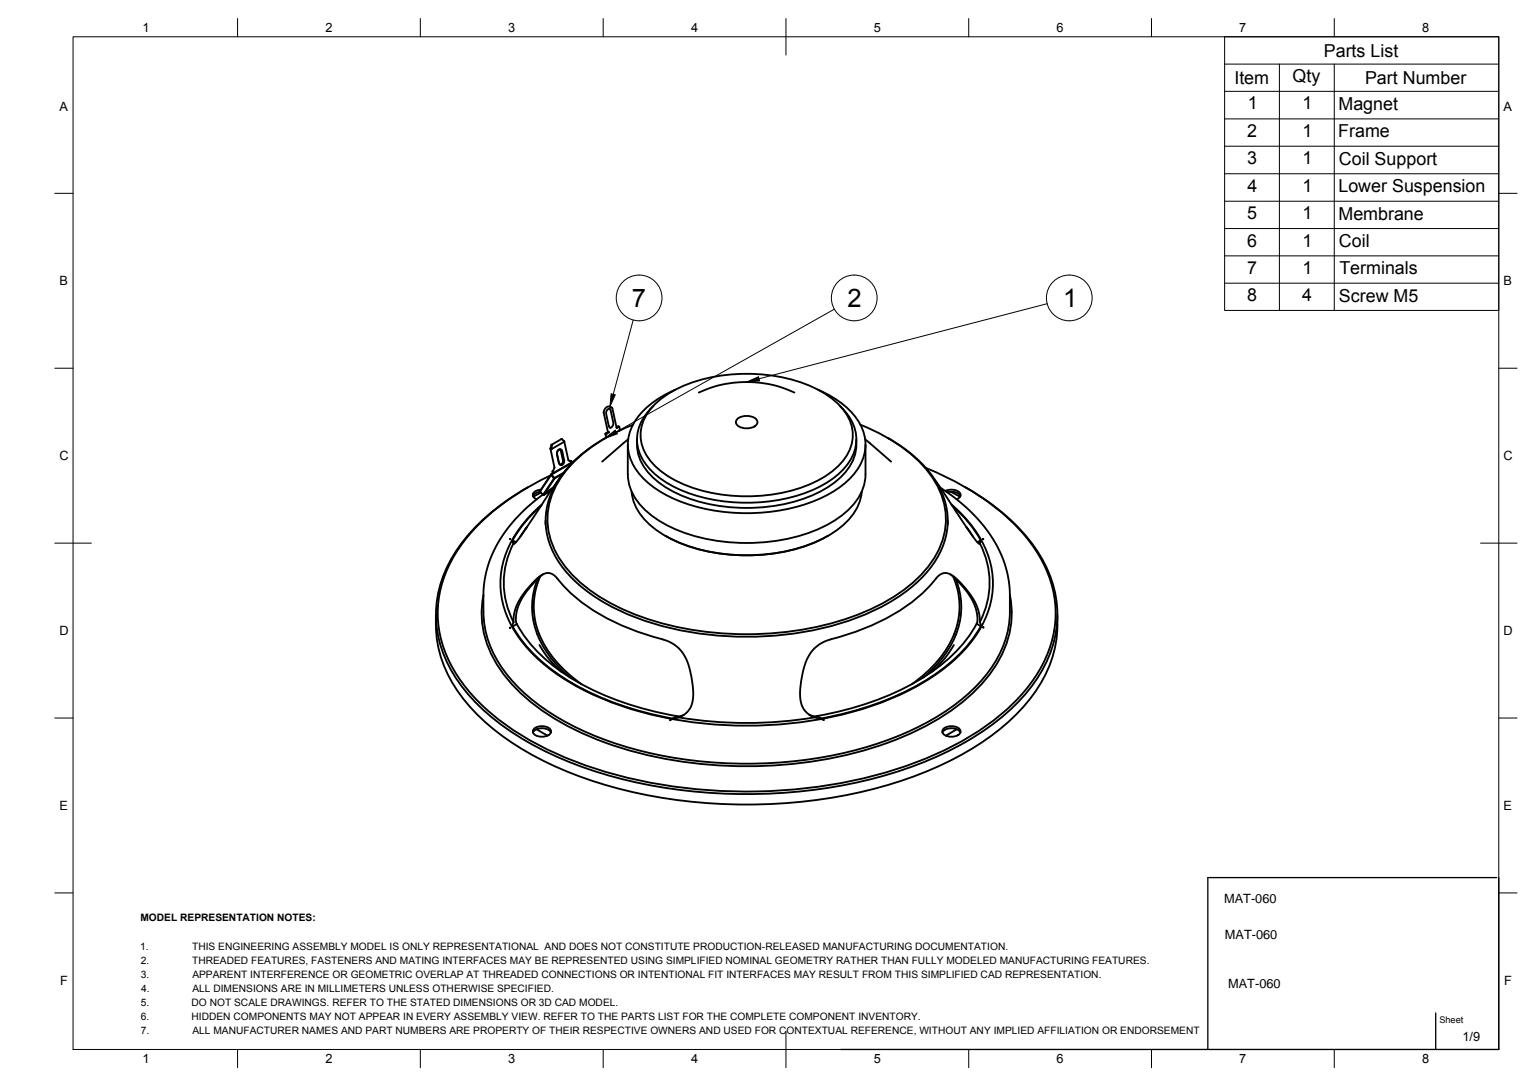
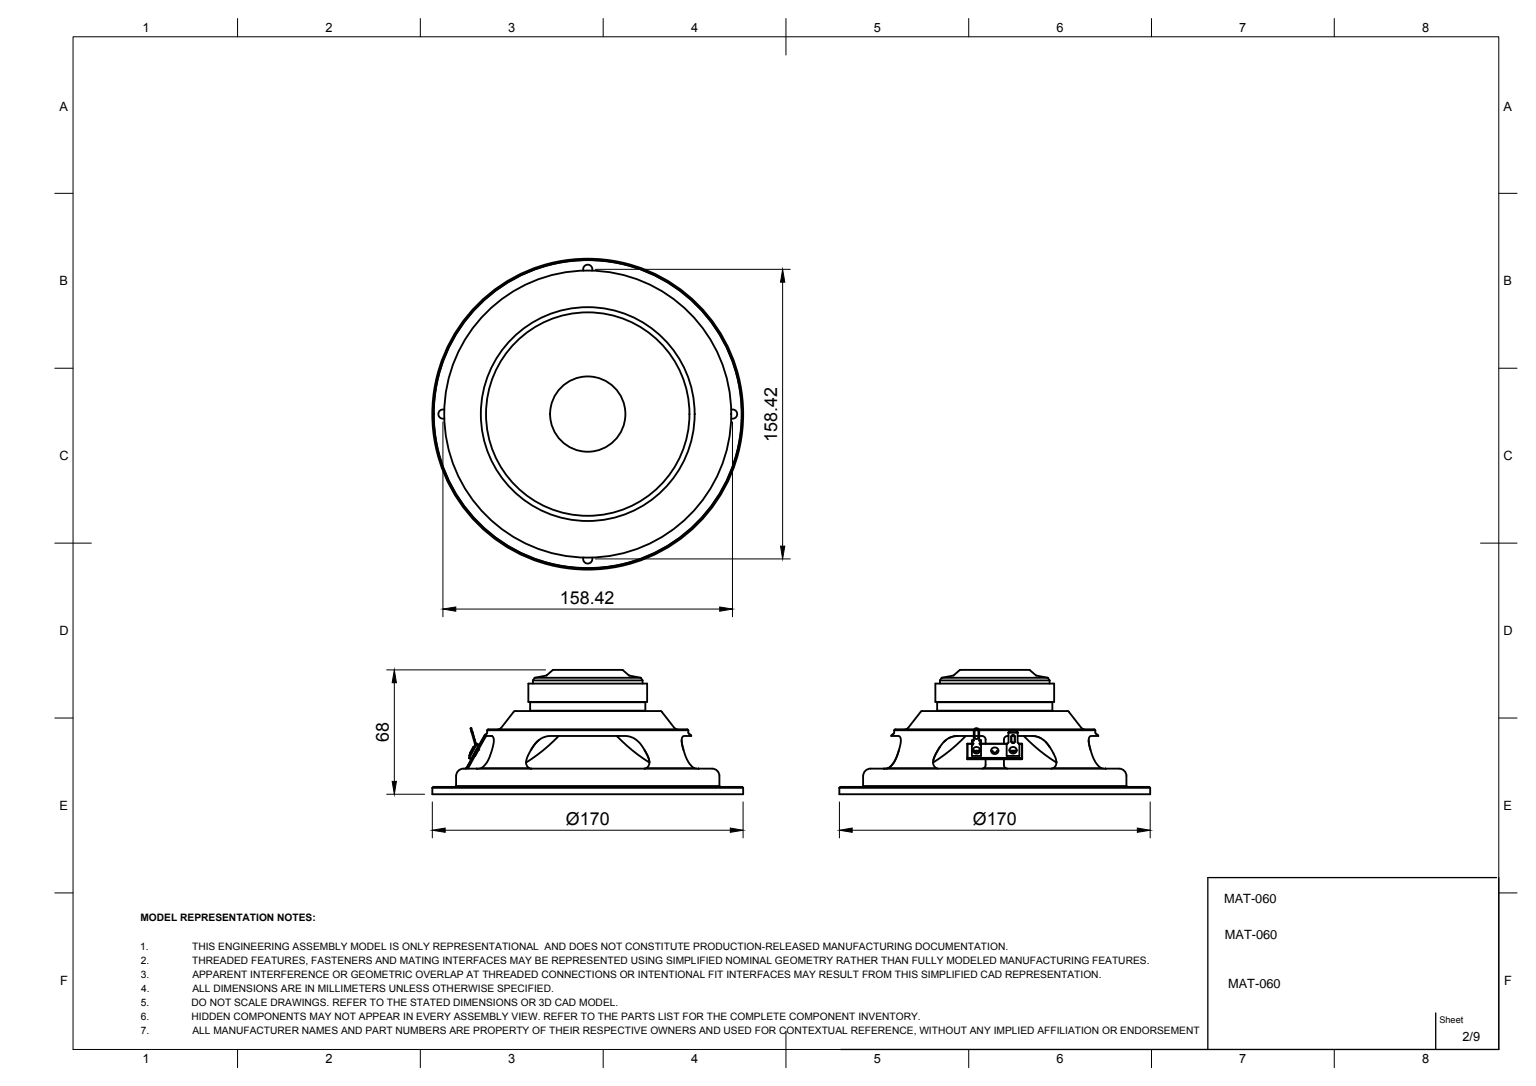
ISO-10303-21;
HEADER;
FILE_DESCRIPTION (('STEP AP214'),
    '1' );
FILE_NAME ('MAT-060',
    '2026-10-29T23:46:56',
    ( '' ),
    ( '' ),
    'SwSTEP 2.0',
    'SolidWorks 2020',
    '' );
FILE_SCHEMA (( 'AUTOMOTIVE_DESIGN' ));
ENDSEC;

DATA;
#1 = ADVANCED_FACE ( 'NONE', ( #23407 ), #603, .F. ) ;
#2 = VECTOR ( 'NONE', #10897, 1000.000000000000000 ) ;
#3 = CARTESIAN_POINT ( 'NONE',  ( -8.402144023942796025, 14.86454579224779948, 47.04930799450052348 ) ) ;
#4 = CIRCLE ( 'NONE', #18333, 0.1250000000000001110 ) ;
#5 = EDGE_CURVE ( 'NONE', #10473, #12904, #9508, .T. ) ;
#6 = ADVANCED_FACE ( 'NONE', ( #18472 ), #27339, .T. ) ;
#7 = DIRECTION ( 'NONE',  ( -0.000000000000000000, -1.000000000000000000, 0.000000000000000000 ) ) ;
#8 = ORIENTED_EDGE ( 'NONE', *, *, #21426, .T. ) ;
#9 = CARTESIAN_POINT ( 'NONE',  ( 52.18344119656808289, -5.936379232154279428, 107.4303245894588628 ) ) ;
#10 = ORIENTED_EDGE ( 'NONE', *, *, #17862, .T. ) ;
#11 = DIRECTION ( 'NONE',  ( 0.000000000000000000, 0.000000000000000000, -1.000000000000000000 ) ) ;
#12 = DIRECTION ( 'NONE',  ( -1.000000000000000000, 0.000000000000000000, 0.000000000000000000 ) ) ;
#13 = VECTOR ( 'NONE', #9862, 1000.000000000000000 ) ;
#14 = CONICAL_SURFACE ( 'NONE', #3681, 2.923537884824412014, 0.6981317007977324574 ) ;
#15 = CARTESIAN_POINT ( 'NONE',  ( 49.15300726216835159, 22.74928388133296764, 45.65942558980532340 ) ) ;
#16 = CIRCLE ( 'NONE', #21997, 37.50000000000000711 ) ;
#17 = AXIS2_PLACEMENT_3D ( 'NONE', #6109, #14151, #26614 ) ;
#18 = EDGE_CURVE ( 'NONE', #23289, #31921, #28501, .T. ) ;
#19 = AXIS2_PLACEMENT_3D ( 'NONE', #29892, #26933, #14470 ) ;
#20 = EDGE_LOOP ( 'NONE', ( #20639, #20304, #9074, #30153 ) ) ;
#21 = ORIENTED_EDGE ( 'NONE', *, *, #19854, .F. ) ;
#22 = DIRECTION ( 'NONE',  ( 7.588956326749211550E-18, -4.206627182996911684E-18, 1.000000000000000000 ) ) ;
#23 = DIRECTION ( 'NONE',  ( 0.000000000000000000, 0.000000000000000000, 1.000000000000000000 ) ) ;
#24 = CARTESIAN_POINT ( 'NONE',  ( 46.00908685603034343, 26.23284706826093071, 44.91496614357595263 ) ) ;
#25 = CONICAL_SURFACE ( 'NONE', #4214, 67.38776620500242132, 0.5061454830783623793 ) ;
#26 = VERTEX_POINT ( 'NONE', #18783 ) ;
#27 = DIRECTION ( 'NONE',  ( 0.9612616959383206705, 0.2756373558169926130, 8.795445018804289444E-19 ) ) ;
#28 = FACE_OUTER_BOUND ( 'NONE', #27332, .T. ) ;
#29 = CARTESIAN_POINT ( 'NONE',  ( -42.41019933908752648, 14.71530103803245915, 55.14139656020049785 ) ) ;
#30 = EDGE_CURVE ( 'NONE', #9758, #27591, #28910, .T. ) ;
#31 = DIRECTION ( 'NONE',  ( -1.101824276508909887E-16, 1.000000000000000000, -0.000000000000000000 ) ) ;
#32 = AXIS2_PLACEMENT_3D ( 'NONE', #27691, #3055, #609 ) ;
#33 = EDGE_CURVE ( 'NONE', #28622, #18652, #13708, .T. ) ;
#34 = CARTESIAN_POINT ( 'NONE',  ( 46.96819297411687444, 27.59253733014356058, 49.54594323136014822 ) ) ;
#35 = CARTESIAN_POINT ( 'NONE',  ( 49.62252444096254322, 24.84787913140503690, 48.68715535708000175 ) ) ;
#36 = DIRECTION ( 'NONE',  ( 0.9612616959383191162, 0.2756373558169986082, 8.795445018805098335E-19 ) ) ;
#37 = CARTESIAN_POINT ( 'NONE',  ( 44.79156314060809763, 22.80400562401889530, 46.92953032342012420 ) ) ;
#38 = FACE_OUTER_BOUND ( 'NONE', #16032, .T. ) ;
#39 = VECTOR ( 'NONE', #4275, 1000.000000000000000 ) ;
#40 = CARTESIAN_POINT ( 'NONE',  ( 21.09785597605719332, 12.26495659406217342, 47.04930799450051637 ) ) ;
#41 = AXIS2_PLACEMENT_3D ( 'NONE', #1077, #13253, #30795 ) ;
#42 = FILL_AREA_STYLE ('',( #30241 ) ) ;
#43 = ORIENTED_EDGE ( 'NONE', *, *, #17117, .T. ) ;
#44 = ORIENTED_EDGE ( 'NONE', *, *, #10247, .F. ) ;
#45 = AXIS2_PLACEMENT_3D ( 'NONE', #7239, #26769, #16743 ) ;
#46 = DIRECTION ( 'NONE',  ( -1.000000000000000000, 0.000000000000000000, 0.000000000000000000 ) ) ;
#47 = VECTOR ( 'NONE', #22684, 1000.000000000000114 ) ;
#48 = DIRECTION ( 'NONE',  ( 1.000000000000000000, -3.756723415560144304E-15, 0.000000000000000000 ) ) ;
#49 = EDGE_CURVE ( 'NONE', #29330, #16793, #26511, .T. ) ;
#50 = DIRECTION ( 'NONE',  ( -1.000000000000000000, 0.000000000000000000, 0.000000000000000000 ) ) ;
#51 = ADVANCED_FACE ( 'NONE', ( #19270 ), #7428, .T. ) ;
#52 = EDGE_LOOP ( 'NONE', ( #4319, #21732, #2975, #7082 ) ) ;
#53 = DIRECTION ( 'NONE',  ( -1.000000000000000000, 0.000000000000000000, 0.000000000000000000 ) ) ;
#54 = CARTESIAN_POINT ( 'NONE',  ( -41.75126335834794133, 15.45321085637654690, 35.55750462089839203 ) ) ;
#55 = ORIENTED_EDGE ( 'NONE', *, *, #8639, .T. ) ;
#56 = ORIENTED_EDGE ( 'NONE', *, *, #16072, .T. ) ;
#57 = CARTESIAN_POINT ( 'NONE',  ( -40.99628586177130529, 8.927770518203464789, 58.05249952744806308 ) ) ;
#58 = CARTESIAN_POINT ( 'NONE',  ( 44.70507715278255745, 27.74951373492759643, 46.92503878583764987 ) ) ;
#59 = AXIS2_PLACEMENT_3D ( 'NONE', #2818, #5773, #10865 ) ;
#60 = LINE ( 'NONE', #27627, #25175 ) ;
#61 = DIRECTION ( 'NONE',  ( -0.000000000000000000, -1.000000000000000000, 0.000000000000000000 ) ) ;
#62 = PLANE ( 'NONE',  #14629 ) ;
#63 = VERTEX_POINT ( 'NONE', #26669 ) ;
#64 = DIRECTION ( 'NONE',  ( -1.101824276508909887E-16, 1.000000000000000000, -0.000000000000000000 ) ) ;
#65 = AXIS2_PLACEMENT_3D ( 'NONE', #14177, #6132, #1197 ) ;
#66 = ORIENTED_EDGE ( 'NONE', *, *, #7414, .F. ) ;
#67 =( BOUNDED_CURVE ( )  B_SPLINE_CURVE ( 3, ( #13523, #18741, #20741, #23527 ),
 .UNSPECIFIED., .F., .F. ) 
 B_SPLINE_CURVE_WITH_KNOTS ( ( 4, 4 ),
 ( 1.099063246724957033, 1.220321128156881318 ),
 .UNSPECIFIED. ) 
 CURVE ( )  GEOMETRIC_REPRESENTATION_ITEM ( )  RATIONAL_B_SPLINE_CURVE ( ( 1.000000000000000000, 0.9987750858034805113, 0.9987750858034805113, 1.000000000000000000 ) ) 
 REPRESENTATION_ITEM ( '' )  );
#68 = FACE_OUTER_BOUND ( 'NONE', #23592, .T. ) ;
#69 = CARTESIAN_POINT ( 'NONE',  ( -40.69193635511749108, 9.347952559758585522, 39.44930799450052206 ) ) ;
#70 = CIRCLE ( 'NONE', #12126, 59.80962967564905597 ) ;
#71 = ORIENTED_EDGE ( 'NONE', *, *, #26696, .T. ) ;
#72 = CARTESIAN_POINT ( 'NONE',  ( -40.77849034781615956, 8.435947495041027366, 34.55508635502627612 ) ) ;
#73 = EDGE_LOOP ( 'NONE', ( #31161, #6796, #19023, #7064 ) ) ;
#74 = CARTESIAN_POINT ( 'NONE',  ( 21.09992658989238734, 38.56284415653841791, 47.04930799450051637 ) ) ;
#75 = CARTESIAN_POINT ( 'NONE',  ( -40.75848109938849717, 9.580021662090986823, 38.54930799450052348 ) ) ;
#76 = DIRECTION ( 'NONE',  ( 0.4848096202463429982, 0.8746197071393925215, 9.920727850371698576E-18 ) ) ;
#77 = ORIENTED_EDGE ( 'NONE', *, *, #10123, .F. ) ;
#78 = CARTESIAN_POINT ( 'NONE',  ( 21.09785597605719332, 15.24673779880127356, 47.04930799450051637 ) ) ;
#79 = DIRECTION ( 'NONE',  ( -1.000000000000000000, 0.000000000000000000, 0.000000000000000000 ) ) ;
#80 = DIRECTION ( 'NONE',  ( -1.000000000000000000, -1.101824276508909887E-16, 0.000000000000000000 ) ) ;
#81 = EDGE_CURVE ( 'NONE', #21567, #17692, #8244, .T. ) ;
#82 = CARTESIAN_POINT ( 'NONE',  ( -39.58809650894544774, 2.596771453999702661, 45.04930799450051637 ) ) ;
#83 = CONICAL_SURFACE ( 'NONE', #4821, 67.99999999999998579, 0.5061454830783623793 ) ;
#84 = ADVANCED_FACE ( 'NONE', ( #31282 ), #25012, .T. ) ;
#85 = DIRECTION ( 'NONE',  ( 0.000000000000000000, 1.000000000000000000, -0.000000000000000000 ) ) ;
#86 = ORIENTED_EDGE ( 'NONE', *, *, #14796, .T. ) ;
#87 = AXIS2_PLACEMENT_3D ( 'NONE', #1243, #25723, #26032 ) ;
#88 = DIRECTION ( 'NONE',  ( 0.000000000000000000, 1.000000000000000000, -0.000000000000000000 ) ) ;
#89 = DIRECTION ( 'NONE',  ( -1.000000000000000000, 0.000000000000000000, 0.000000000000000000 ) ) ;
#90 = VERTEX_POINT ( 'NONE', #16171 ) ;
#91 = AXIS2_PLACEMENT_3D ( 'NONE', #3983, #26796, #16125 ) ;
#92 = CARTESIAN_POINT ( 'NONE',  ( 21.09992658989239089, 30.34164230456639544, 47.04930799450051637 ) ) ;
#93 = APPLICATION_CONTEXT ( 'automotive_design' ) ;
#94 = DIRECTION ( 'NONE',  ( 0.000000000000000000, 0.000000000000000000, 1.000000000000000000 ) ) ;
#95 = ORIENTED_EDGE ( 'NONE', *, *, #26981, .T. ) ;
#96 = CARTESIAN_POINT ( 'NONE',  ( -35.64882101543633297, 9.925589859889722533, 42.04930799450051637 ) ) ;
#97 = ORIENTED_EDGE ( 'NONE', *, *, #2403, .T. ) ;
#98 = CONICAL_SURFACE ( 'NONE', #18421, 11.79999999999997762, 0.7853981633974786991 ) ;
#99 = EDGE_LOOP ( 'NONE', ( #29307, #17559, #4595, #27909 ) ) ;
#100 = VECTOR ( 'NONE', #2675, 1000.000000000000114 ) ;
#101 = LINE ( 'NONE', #30305, #23466 ) ;
#102 = DIRECTION ( 'NONE',  ( 1.000000000000000000, 0.000000000000000000, 0.000000000000000000 ) ) ;
#103 = ORIENTED_EDGE ( 'NONE', *, *, #27267, .F. ) ;
#104 = VERTEX_POINT ( 'NONE', #1886 ) ;
#105 = CYLINDRICAL_SURFACE ( 'NONE', #15721, 33.50000000000000000 ) ;
#106 = DIRECTION ( 'NONE',  ( 0.000000000000000000, 0.000000000000000000, 1.000000000000000000 ) ) ;
#107 = DIRECTION ( 'NONE',  ( 1.000000000000000000, 0.000000000000000000, 0.000000000000000000 ) ) ;
#108 = DIRECTION ( 'NONE',  ( 0.9612616959383206705, 0.2756373558169926130, 8.795445018804289444E-19 ) ) ;
#109 = FACE_OUTER_BOUND ( 'NONE', #5838, .T. ) ;
#110 = VERTEX_POINT ( 'NONE', #16495 ) ;
#111 = DIRECTION ( 'NONE',  ( -0.000000000000000000, 1.000000000000000000, -0.000000000000000000 ) ) ;
#112 = VERTEX_POINT ( 'NONE', #21899 ) ;
#113 = CARTESIAN_POINT ( 'NONE',  ( 8.732853799281732776, 24.72145308207319303, 47.04930799450051637 ) ) ;
#114 = CARTESIAN_POINT ( 'NONE',  ( 80.65492537559437380, -5.936611295272316902, 15.94352045161622655 ) ) ;
#115 = VECTOR ( 'NONE', #2052, 999.9999999999998863 ) ;
#116 = VERTEX_POINT ( 'NONE', #3866 ) ;
#117 = CARTESIAN_POINT ( 'NONE',  ( 8.732853799281729223, 24.47145308207319303, 47.04930799450051637 ) ) ;
#118 = SPHERICAL_SURFACE ( 'NONE', #22577, 0.1000000000000000056 ) ;
#119 = DIRECTION ( 'NONE',  ( -1.101824276508909887E-16, 1.000000000000000000, -0.000000000000000000 ) ) ;
#120 = CYLINDRICAL_SURFACE ( 'NONE', #5324, 12.36707279061065101 ) ;
#121 = FACE_OUTER_BOUND ( 'NONE', #7290, .T. ) ;
#122 = EDGE_CURVE ( 'NONE', #19617, #28878, #29198, .T. ) ;
#123 = EDGE_CURVE ( 'NONE', #13895, #2732, #897, .T. ) ;
#124 = TOROIDAL_SURFACE ( 'NONE', #25795, 12.40141737965280555, 0.1250000000000006939 ) ;
#125 = CARTESIAN_POINT ( 'NONE',  ( 44.70507715278255745, 28.36291119454914877, 46.92503878583765697 ) ) ;
#126 = EDGE_CURVE ( 'NONE', #12313, #19851, #23434, .T. ) ;
#127 = FACE_OUTER_BOUND ( 'NONE', #2532, .T. ) ;
#128 = DIRECTION ( 'NONE',  ( 0.000000000000000000, 0.000000000000000000, -1.000000000000000000 ) ) ;
#129 = ADVANCED_FACE ( 'NONE', ( #26182 ), #24211, .T. ) ;
#130 = ADVANCED_FACE ( 'NONE', ( #9112 ), #21404, .F. ) ;
#131 = EDGE_LOOP ( 'NONE', ( #2067, #16349, #32197, #29803 ) ) ;
#132 = DIRECTION ( 'NONE',  ( 0.000000000000000000, 0.000000000000000000, -1.000000000000000000 ) ) ;
#133 = CARTESIAN_POINT ( 'NONE',  ( 33.72499318558949710, 28.84143805560861296, 47.04930799450051637 ) ) ;
#134 = ORIENTED_EDGE ( 'NONE', *, *, #4627, .F. ) ;
#135 = AXIS2_PLACEMENT_3D ( 'NONE', #30752, #22633, #17877 ) ;
#136 = FACE_OUTER_BOUND ( 'NONE', #14776, .T. ) ;
#137 = ORIENTED_EDGE ( 'NONE', *, *, #30547, .F. ) ;
#138 = CIRCLE ( 'NONE', #18459, 2.500000000000003553 ) ;
#139 = EDGE_LOOP ( 'NONE', ( #10436, #9194, #21125, #26055 ) ) ;
#140 = CARTESIAN_POINT ( 'NONE',  ( 21.09992658989239089, 27.84164230456639544, 47.04930799450051637 ) ) ;
#141 = ORIENTED_EDGE ( 'NONE', *, *, #21145, .F. ) ;
#142 = CIRCLE ( 'NONE', #13264, 12.36707279061065101 ) ;
#143 = ORIENTED_EDGE ( 'NONE', *, *, #20256, .T. ) ;
#144 = AXIS2_PLACEMENT_3D ( 'NONE', #10705, #31040, #25937 ) ;
#145 = CARTESIAN_POINT ( 'NONE',  ( 46.44275705260056242, 23.09557481883486219, 47.38348660136355051 ) ) ;
#146 = EDGE_CURVE ( 'NONE', #7136, #25895, #22084, .T. ) ;
#147 = ORIENTED_EDGE ( 'NONE', *, *, #1574, .F. ) ;
#148 = DIRECTION ( 'NONE',  ( -1.000000000000000000, 0.000000000000000000, 0.000000000000000000 ) ) ;
#149 = AXIS2_PLACEMENT_3D ( 'NONE', #13743, #23739, #24058 ) ;
#150 = FACE_OUTER_BOUND ( 'NONE', #25843, .T. ) ;
#151 = CARTESIAN_POINT ( 'NONE',  ( -9.910881874767294875, -5.936607700120025477, -13.36061728824001804 ) ) ;
#152 = CARTESIAN_POINT ( 'NONE',  ( 45.79384627280941089, 24.97957786121582302, 49.05938063676249072 ) ) ;
#153 = ORIENTED_EDGE ( 'NONE', *, *, #20856, .F. ) ;
#154 = VERTEX_POINT ( 'NONE', #31766 ) ;
#155 = VERTEX_POINT ( 'NONE', #13728 ) ;
#156 = CARTESIAN_POINT ( 'NONE',  ( -40.54018958231235814, 7.005332542891154368, 35.02307665165292150 ) ) ;
#157 = DIRECTION ( 'NONE',  ( -1.000000000000000000, 0.000000000000000000, 0.000000000000000000 ) ) ;
#158 = CARTESIAN_POINT ( 'NONE',  ( -40.76199410932685652, 8.110698076655893374, 59.50788663826320146 ) ) ;
#159 = CARTESIAN_POINT ( 'NONE',  ( 21.09785597605720753, 14.86454579224779948, 47.04930799450052348 ) ) ;
#160 = CARTESIAN_POINT ( 'NONE',  ( 75.19785597605721250, 14.66454579224780019, 47.04930799450051637 ) ) ;
#161 = EDGE_CURVE ( 'NONE', #17230, #26186, #19107, .T. ) ;
#162 = PRODUCT_CONTEXT ( 'NONE', #1750, 'mechanical' ) ;
#163 = VERTEX_POINT ( 'NONE', #26839 ) ;
#164 = ORIENTED_EDGE ( 'NONE', *, *, #2840, .T. ) ;
#165 = DIRECTION ( 'NONE',  ( 0.8907924397839086517, 1.100109291107994064E-16, -0.4544104193609905251 ) ) ;
#166 = FACE_OUTER_BOUND ( 'NONE', #10063, .T. ) ;
#167 = DIRECTION ( 'NONE',  ( -0.000000000000000000, -1.000000000000000000, -0.000000000000000000 ) ) ;
#168 = VECTOR ( 'NONE', #18188, 1000.000000000000114 ) ;
#169 = ORIENTED_EDGE ( 'NONE', *, *, #20266, .F. ) ;
#170 = DIRECTION ( 'NONE',  ( -1.096245967261381435E-16, 0.000000000000000000, 1.000000000000000000 ) ) ;
#171 = AXIS2_PLACEMENT_3D ( 'NONE', #9638, #108, #19631 ) ;
#172 = EDGE_LOOP ( 'NONE', ( #1126, #13141, #16684, #10184 ) ) ;
#173 = CARTESIAN_POINT ( 'NONE',  ( 21.09992658989239089, 24.71664230456639899, 47.04930799450051637 ) ) ;
#174 = DIRECTION ( 'NONE',  ( -1.101824276508909887E-16, 1.000000000000000000, -0.000000000000000000 ) ) ;
#175 = DIRECTION ( 'NONE',  ( 0.3958453973320085195, 0.7141240004913234074, 0.5773502691896251759 ) ) ;
#176 = VECTOR ( 'NONE', #32272, 1000.000000000000114 ) ;
#177 = VECTOR ( 'NONE', #9320, 1000.000000000000114 ) ;
#178 = EDGE_CURVE ( 'NONE', #17205, #26283, #21557, .T. ) ;
#179 = EDGE_CURVE ( 'NONE', #22338, #15550, #10168, .T. ) ;
#180 = VERTEX_POINT ( 'NONE', #22065 ) ;
#181 = ORIENTED_EDGE ( 'NONE', *, *, #20445, .T. ) ;
#182 = DIRECTION ( 'NONE',  ( -1.000000000000000000, 0.000000000000000000, 0.000000000000000000 ) ) ;
#183 = ADVANCED_FACE ( 'NONE', ( #22228 ), #31147, .T. ) ;
#184 = DIRECTION ( 'NONE',  ( 0.8746197071393858602, -0.4848096202463547666, 0.000000000000000000 ) ) ;
#185 = CARTESIAN_POINT ( 'NONE',  ( 49.49063479933183629, 26.69951373492759927, 47.17357720316391578 ) ) ;
#186 = EDGE_CURVE ( 'NONE', #20059, #17152, #210, .T. ) ;
#187 = ORIENTED_EDGE ( 'NONE', *, *, #28945, .F. ) ;
#188 = AXIS2_PLACEMENT_3D ( 'NONE', #771, #25875, #3057 ) ;
#189 = CARTESIAN_POINT ( 'NONE',  ( -29.27613032885505007, 5.786704587343633577, 77.24891569812123748 ) ) ;
#190 = CARTESIAN_POINT ( 'NONE',  ( 21.09992658989238734, 38.56284415653841791, 47.04930799450051637 ) ) ;
#191 = CARTESIAN_POINT ( 'NONE',  ( 8.698509210239514289, 24.84164230456639544, 47.04930799450051637 ) ) ;
#192 = DIRECTION ( 'NONE',  ( -0.9612616959383207815, -0.2756373558169926685, -8.795445018804289444E-19 ) ) ;
#193 = DIRECTION ( 'NONE',  ( -1.000000000000000000, 0.000000000000000000, 0.000000000000000000 ) ) ;
#194 = CARTESIAN_POINT ( 'NONE',  ( 48.28214861297873028, 24.78954579807170333, 49.37090702980594870 ) ) ;
#196 = CIRCLE ( 'NONE', #709, 0.8928932188134561798 ) ;
#195 = CARTESIAN_POINT ( 'NONE',  ( -42.67844523361456766, 15.18734573188464765, 35.55750462089839203 ) ) ;
#197 = DIRECTION ( 'NONE',  ( -0.9612616959383183390, -0.2756373558170014948, -8.795445018805493151E-19 ) ) ;
#198 = CIRCLE ( 'NONE', #29008, 34.00000000000000000 ) ;
#199 = CARTESIAN_POINT ( 'NONE',  ( 42.60793425459065986, 11.86918370369814113, 98.63420711611333047 ) ) ;
#200 = DIRECTION ( 'NONE',  ( -1.000000000000000000, 0.000000000000000000, 0.000000000000000000 ) ) ;
#201 = EDGE_CURVE ( 'NONE', #31745, #29739, #32095, .T. ) ;
#202 = ORIENTED_EDGE ( 'NONE', *, *, #17749, .F. ) ;
#203 = ORIENTED_EDGE ( 'NONE', *, *, #32319, .T. ) ;
#204 = CARTESIAN_POINT ( 'NONE',  ( 33.46699938050303302, 38.56284415653841791, 47.04930799450051637 ) ) ;
#205 = CARTESIAN_POINT ( 'NONE',  ( 49.62266228875127183, 24.94631262459061105, 46.45121837018842825 ) ) ;
#206 = LINE ( 'NONE', #27459, #13028 ) ;
#207 = CARTESIAN_POINT ( 'NONE',  ( 48.66895200406656130, 27.18420399681022914, 44.62753372671561181 ) ) ;
#208 = ORIENTED_EDGE ( 'NONE', *, *, #19172, .F. ) ;
#209 = DIRECTION ( 'NONE',  ( 0.2756373558169961657, -0.9612616959383196713, -2.918609477355923238E-15 ) ) ;
#210 = CIRCLE ( 'NONE', #18531, 55.85791022362053582 ) ;
#211 = CARTESIAN_POINT ( 'NONE',  ( -43.29088418437023478, 1.073429008971243270, 39.44930799450052916 ) ) ;
#212 = CARTESIAN_POINT ( 'NONE',  ( 21.09785597605720753, 15.23835801850285776, 47.04930799450052348 ) ) ;
#213 = ORIENTED_EDGE ( 'NONE', *, *, #21228, .T. ) ;
#214 = ORIENTED_EDGE ( 'NONE', *, *, #14166, .F. ) ;
#215 = CARTESIAN_POINT ( 'NONE',  ( 8.732853799281732776, 31.97145308207317171, 47.04930799450051637 ) ) ;
#216 = CARTESIAN_POINT ( 'NONE',  ( 46.00908685603034343, 25.53284706826093498, 44.91496614357595263 ) ) ;
#217 = DIRECTION ( 'NONE',  ( -1.000000000000000000, 0.000000000000000000, 0.000000000000000000 ) ) ;
#218 = LINE ( 'NONE', #12381, #10663 ) ;
#219 = CARTESIAN_POINT ( 'NONE',  ( 8.823509210239564027, 29.84164230456639899, 47.04930799450051637 ) ) ;
#220 = ADVANCED_FACE ( 'NONE', ( #24531 ), #2050, .F. ) ;
#221 = EDGE_CURVE ( 'NONE', #14341, #26283, #20036, .T. ) ;
#222 = EDGE_LOOP ( 'NONE', ( #26928, #11446, #19601, #18830 ) ) ;
#223 = DIRECTION ( 'NONE',  ( -1.000000000000000000, 0.000000000000000000, 0.000000000000000000 ) ) ;
#224 = EDGE_CURVE ( 'NONE', #23081, #15904, #26859, .T. ) ;
#225 = ORIENTED_EDGE ( 'NONE', *, *, #23042, .T. ) ;
#226 = EDGE_CURVE ( 'NONE', #1958, #14944, #28442, .T. ) ;
#227 = FACE_OUTER_BOUND ( 'NONE', #31629, .T. ) ;
#228 = DIRECTION ( 'NONE',  ( -1.101824276508909887E-16, 1.000000000000000000, -0.000000000000000000 ) ) ;
#229 = VERTEX_POINT ( 'NONE', #19763 ) ;
#230 = CARTESIAN_POINT ( 'NONE',  ( 21.09992658989238734, 31.96183152705962272, 47.04930799450051637 ) ) ;
#231 = VERTEX_POINT ( 'NONE', #9774 ) ;
#232 = CARTESIAN_POINT ( 'NONE',  ( -40.60333149162104860, 7.557375771971046596, 56.04611646155296256 ) ) ;
#233 = DIRECTION ( 'NONE',  ( -1.000000000000000000, 0.000000000000000000, 0.000000000000000000 ) ) ;
#234 = AXIS2_PLACEMENT_3D ( 'NONE', #13203, #26134, #3648 ) ;
#235 = CARTESIAN_POINT ( 'NONE',  ( -3.126678918709510313, 11.18855628041951711, -3.738293121569808086 ) ) ;
#236 = AXIS2_PLACEMENT_3D ( 'NONE', #25222, #28009, #15050 ) ;
#237 = DIRECTION ( 'NONE',  ( -1.101824276508909887E-16, 1.000000000000000000, -0.000000000000000000 ) ) ;
#238 = ORIENTED_EDGE ( 'NONE', *, *, #2347, .F. ) ;
#239 = CARTESIAN_POINT ( 'NONE',  ( 75.35669764717297880, -2.578969365796030200, 80.79736519221168578 ) ) ;
#240 = CARTESIAN_POINT ( 'NONE',  ( -40.59758774925371938, 7.567737757495682338, 34.64930799450051779 ) ) ;
#241 = AXIS2_PLACEMENT_3D ( 'NONE', #30077, #17255, #27274 ) ;
#242 = AXIS2_PLACEMENT_3D ( 'NONE', #2741, #20287, #4883 ) ;
#243 = DIRECTION ( 'NONE',  ( 0.000000000000000000, 0.000000000000000000, 1.000000000000000000 ) ) ;
#244 = VECTOR ( 'NONE', #7734, 1000.000000000000114 ) ;
#245 = CARTESIAN_POINT ( 'NONE',  ( 75.84373340226019877, -1.823725651226874023, 80.73552270632580985 ) ) ;
#246 = ORIENTED_EDGE ( 'NONE', *, *, #15564, .T. ) ;
#247 = CARTESIAN_POINT ( 'NONE',  ( 42.59785597605719687, 13.86454579224779948, 47.04930799450052348 ) ) ;
#248 = DIRECTION ( 'NONE',  ( 0.000000000000000000, -0.000000000000000000, -1.000000000000000000 ) ) ;
#249 = ORIENTED_EDGE ( 'NONE', *, *, #29875, .T. ) ;
#250 = DIRECTION ( 'NONE',  ( -0.9612616959383205595, -0.2756373558169929461, 1.660411357259281952E-16 ) ) ;
#251 = DIRECTION ( 'NONE',  ( -0.000000000000000000, 1.000000000000000000, -0.000000000000000000 ) ) ;
#252 = LINE ( 'NONE', #27506, #6964 ) ;
#253 = VERTEX_POINT ( 'NONE', #29471 ) ;
#254 = DIRECTION ( 'NONE',  ( -1.101824276508909887E-16, 1.000000000000000000, -0.000000000000000000 ) ) ;
#255 = ORIENTED_EDGE ( 'NONE', *, *, #25304, .F. ) ;
#256 = EDGE_CURVE ( 'NONE', #10661, #20619, #16974, .T. ) ;
#257 = VERTEX_POINT ( 'NONE', #4514 ) ;
#258 = AXIS2_PLACEMENT_3D ( 'NONE', #29211, #16405, #11331 ) ;
#259 = CIRCLE ( 'NONE', #4453, 2.500000000000002220 ) ;
#260 = AXIS2_PLACEMENT_3D ( 'NONE', #19965, #12767, #2897 ) ;
#261 = TOROIDAL_SURFACE ( 'NONE', #15443, 0.2000000000000000111, 0.1000000000000000056 ) ;
#262 = EDGE_CURVE ( 'NONE', #32275, #3483, #1780, .T. ) ;
#263 = VECTOR ( 'NONE', #8856, 1000.000000000000000 ) ;
#264 = CARTESIAN_POINT ( 'NONE',  ( 8.732853799281732776, 30.71183152705961916, 47.04930799450051637 ) ) ;
#265 = FACE_OUTER_BOUND ( 'NONE', #5953, .T. ) ;
#266 = ORIENTED_EDGE ( 'NONE', *, *, #15415, .T. ) ;
#267 = ORIENTED_EDGE ( 'NONE', *, *, #8560, .T. ) ;
#268 = CARTESIAN_POINT ( 'NONE',  ( 21.09785597605719332, 14.58544108513610027, 34.31529089466609150 ) ) ;
#269 = DIRECTION ( 'NONE',  ( -1.000000000000000000, 0.000000000000000000, 0.000000000000000000 ) ) ;
#270 = LINE ( 'NONE', #3046, #13238 ) ;
#271 = DIRECTION ( 'NONE',  ( -0.2756373558170082672, 0.9612616959383162296, 0.000000000000000000 ) ) ;
#272 = VERTEX_POINT ( 'NONE', #8893 ) ;
#273 = DIRECTION ( 'NONE',  ( 1.234978253042719660E-16, -1.000000000000000000, -1.109335647967047851E-31 ) ) ;
#274 = ORIENTED_EDGE ( 'NONE', *, *, #5995, .T. ) ;
#275 = CARTESIAN_POINT ( 'NONE',  ( 64.59785597605720397, 13.86454579224779948, 47.04930799450051637 ) ) ;
#276 = CARTESIAN_POINT ( 'NONE',  ( -5.602943079677954685, 9.702389020015065313, -3.412202488244239884 ) ) ;
#277 = ORIENTED_EDGE ( 'NONE', *, *, #29434, .F. ) ;
#278 = CARTESIAN_POINT ( 'NONE',  ( 47.40417757965286683, 23.10527845304106620, 46.57712699531703038 ) ) ;
#279 = CARTESIAN_POINT ( 'NONE',  ( -35.36141981399792655, 11.69881320456492979, 53.11437157513250895 ) ) ;
#280 = DIRECTION ( 'NONE',  ( -0.8746197071393927436, 0.4848096202463423876, 1.277302113040827440E-17 ) ) ;
#281 = DIRECTION ( 'NONE',  ( -1.101824276508909887E-16, 1.000000000000000000, -0.000000000000000000 ) ) ;
#282 = CARTESIAN_POINT ( 'NONE',  ( 48.18662509608405031, 27.19624452788248803, 49.18364984542562013 ) ) ;
#283 = TOROIDAL_SURFACE ( 'NONE', #21230, 1.142135311067127068, 0.1000000000000000056 ) ;
#284 = CARTESIAN_POINT ( 'NONE',  ( -40.04869510400508403, 6.988917179839018168, 35.05065200723174001 ) ) ;
#285 = DIRECTION ( 'NONE',  ( -0.000000000000000000, -1.000000000000000000, 0.000000000000000000 ) ) ;
#286 = VERTEX_POINT ( 'NONE', #26777 ) ;
#287 = CARTESIAN_POINT ( 'NONE',  ( 21.09992658989239089, 24.84164230456639544, 47.04930799450051637 ) ) ;
#288 = AXIS2_PLACEMENT_3D ( 'NONE', #28339, #16328, #21250 ) ;
#289 = ORIENTED_EDGE ( 'NONE', *, *, #14454, .T. ) ;
#290 = VECTOR ( 'NONE', #23726, 1000.000000000000114 ) ;
#291 = AXIS2_PLACEMENT_3D ( 'NONE', #31241, #28293, #23031 ) ;
#292 = PLANE ( 'NONE',  #4320 ) ;
#293 = ORIENTED_EDGE ( 'NONE', *, *, #30810, .T. ) ;
#294 = VERTEX_POINT ( 'NONE', #26940 ) ;
#295 = DIRECTION ( 'NONE',  ( -1.101824276508909887E-16, 1.000000000000000000, -0.000000000000000000 ) ) ;
#296 = AXIS2_PLACEMENT_3D ( 'NONE', #20204, #23316, #10529 ) ;
#297 = ORIENTED_EDGE ( 'NONE', *, *, #25455, .T. ) ;
#298 = EDGE_CURVE ( 'NONE', #8568, #25382, #4926, .T. ) ;
#299 = ADVANCED_FACE ( 'NONE', ( #6919 ), #23984, .F. ) ;
#300 = EDGE_CURVE ( 'NONE', #14294, #4546, #9551, .T. ) ;
#301 = ADVANCED_FACE ( 'NONE', ( #4126 ), #31709, .T. ) ;
#302 = ORIENTED_EDGE ( 'NONE', *, *, #7357, .T. ) ;
#303 = EDGE_CURVE ( 'NONE', #15685, #10922, #5506, .T. ) ;
#304 = CARTESIAN_POINT ( 'NONE',  ( 45.37804019580246973, 22.89977464660286444, 47.76827453631080544 ) ) ;
#305 = CIRCLE ( 'NONE', #9213, 12.27641737965284996 ) ;
#306 = VERTEX_POINT ( 'NONE', #16918 ) ;
#307 = CARTESIAN_POINT ( 'NONE',  ( 21.09785597605720042, -16.63545420775220407, -31.35069200549948221 ) ) ;
#308 = CARTESIAN_POINT ( 'NONE',  ( -10.01358589504979513, -5.935454207834595763, -13.41617548937563598 ) ) ;
#309 = CARTESIAN_POINT ( 'NONE',  ( 45.38854177497844944, 29.72622849631042286, 45.94041160078741370 ) ) ;
#310 = ORIENTED_EDGE ( 'NONE', *, *, #2952, .T. ) ;
#311 = ORIENTED_EDGE ( 'NONE', *, *, #27048, .T. ) ;
#312 = CARTESIAN_POINT ( 'NONE',  ( 21.09992658989239089, 28.46183152705961206, 47.04930799450051637 ) ) ;
#313 = VERTEX_POINT ( 'NONE', #14149 ) ;
#314 = TOROIDAL_SURFACE ( 'NONE', #1339, 12.61792373059896377, 0.1249999999999977518 ) ;
#315 = DIRECTION ( 'NONE',  ( -0.000000000000000000, -1.000000000000000000, 0.000000000000000000 ) ) ;
#316 = CARTESIAN_POINT ( 'NONE',  ( 54.19940832515395357, -4.668720686625173144, 103.9826627183073668 ) ) ;
#317 = DIRECTION ( 'NONE',  ( 2.946248497964555786E-19, 3.001156285468303092E-19, 1.000000000000000000 ) ) ;
#318 = CARTESIAN_POINT ( 'NONE',  ( -40.58856461370174884, 7.499380836222963254, 53.94930799450052206 ) ) ;
#319 = DIRECTION ( 'NONE',  ( -1.224646799147353207E-16, 0.000000000000000000, -1.000000000000000000 ) ) ;
#320 = ORIENTED_EDGE ( 'NONE', *, *, #9164, .F. ) ;
#321 = VERTEX_POINT ( 'NONE', #31552 ) ;
#322 = LINE ( 'NONE', #29718, #31776 ) ;
#323 = CARTESIAN_POINT ( 'NONE',  ( 44.21498992391908445, 28.81753733014356200, 46.89958605635242606 ) ) ;
#324 = CARTESIAN_POINT ( 'NONE',  ( -9.765095477396084078, -5.936631694656546721, 107.5327929641237290 ) ) ;
#325 = CARTESIAN_POINT ( 'NONE',  ( 45.35708200440645044, 27.69118040159426286, 45.92000246470680480 ) ) ;
#326 = ORIENTED_EDGE ( 'NONE', *, *, #9341, .F. ) ;
#327 = CARTESIAN_POINT ( 'NONE',  ( 33.72499318558949710, 27.84184655352419568, 47.04930799450051637 ) ) ;
#328 = CYLINDRICAL_SURFACE ( 'NONE', #6747, 0.1000000000000020595 ) ;
#329 = EDGE_CURVE ( 'NONE', #6215, #18606, #11548, .T. ) ;
#330 = CIRCLE ( 'NONE', #8187, 12.27641737965285529 ) ;
#331 =( GEOMETRIC_REPRESENTATION_CONTEXT ( 3 ) GLOBAL_UNCERTAINTY_ASSIGNED_CONTEXT ( ( #30822 ) ) GLOBAL_UNIT_ASSIGNED_CONTEXT ( ( #10061, #30087, #12694 ) ) REPRESENTATION_CONTEXT ( 'NONE', 'WORKASPACE' ) );
#332 = DIRECTION ( 'NONE',  ( -0.000000000000000000, -1.000000000000000000, 0.000000000000000000 ) ) ;
#333 = ORIENTED_EDGE ( 'NONE', *, *, #7951, .F. ) ;
#334 = ADVANCED_FACE ( 'NONE', ( #16752 ), #23450, .T. ) ;
#335 = EDGE_CURVE ( 'NONE', #25296, #11753, #1955, .T. ) ;
#336 = ORIENTED_EDGE ( 'NONE', *, *, #3292, .T. ) ;
#337 = EDGE_CURVE ( 'NONE', #10189, #17291, #29573, .T. ) ;
#338 = DIRECTION ( 'NONE',  ( -1.101824276508909887E-16, 1.000000000000000000, -0.000000000000000000 ) ) ;
#339 = DIRECTION ( 'NONE',  ( -1.000000000000000000, 0.000000000000000000, 0.000000000000000000 ) ) ;
#340 = DIRECTION ( 'NONE',  ( -1.101824276508909887E-16, 1.000000000000000000, -0.000000000000000000 ) ) ;
#341 = ORIENTED_EDGE ( 'NONE', *, *, #19982, .F. ) ;
#342 = DIRECTION ( 'NONE',  ( 0.4848096202463636484, 0.8746197071393810862, 0.000000000000000000 ) ) ;
#343 = CARTESIAN_POINT ( 'NONE',  ( 81.50778125879762115, -5.936607700120028142, 16.04057014367610989 ) ) ;
#344 = DIRECTION ( 'NONE',  ( -0.000000000000000000, -1.000000000000000000, 0.000000000000000000 ) ) ;
#345 = AXIS2_PLACEMENT_3D ( 'NONE', #21627, #16382, #28696 ) ;
#346 = CARTESIAN_POINT ( 'NONE',  ( 8.698509210239533829, 26.84164230456639899, 47.04930799450051637 ) ) ;
#347 = DIRECTION ( 'NONE',  ( 0.000000000000000000, 0.000000000000000000, 1.000000000000000000 ) ) ;
#348 = DIRECTION ( 'NONE',  ( -0.000000000000000000, -1.000000000000000000, -0.000000000000000000 ) ) ;
#349 = CARTESIAN_POINT ( 'NONE',  ( 21.09992658989239089, 28.46183152705961206, 47.04930799450051637 ) ) ;
#350 = CARTESIAN_POINT ( 'NONE',  ( 44.96133376908166213, 22.84434098701873950, 47.26233605563525941 ) ) ;
#351 = DIRECTION ( 'NONE',  ( 1.000000000000000000, 0.000000000000000000, 0.000000000000000000 ) ) ;
#352 = DIRECTION ( 'NONE',  ( -1.000000000000000000, 0.000000000000000000, 0.000000000000000000 ) ) ;
#353 = CARTESIAN_POINT ( 'NONE',  ( 45.46000861347822308, 28.87287913140503548, 49.57397645940629616 ) ) ;
#354 = SURFACE_STYLE_FILL_AREA ( #4142 ) ;
#355 = ORIENTED_EDGE ( 'NONE', *, *, #11811, .F. ) ;
#356 = ORIENTED_EDGE ( 'NONE', *, *, #17245, .T. ) ;
#357 = CYLINDRICAL_SURFACE ( 'NONE', #3440, 2.000000000000001776 ) ;
#358 = DIRECTION ( 'NONE',  ( -1.101824276508909887E-16, 1.000000000000000000, -0.000000000000000000 ) ) ;
#359 = CARTESIAN_POINT ( 'NONE',  ( -33.78823724555357444, -3.447124724799344175, 13.40102877645825075 ) ) ;
#360 = AXIS2_PLACEMENT_3D ( 'NONE', #25134, #12675, #32035 ) ;
#361 = LINE ( 'NONE', #25479, #15657 ) ;
#362 = ORIENTED_EDGE ( 'NONE', *, *, #4106, .T. ) ;
#363 = CARTESIAN_POINT ( 'NONE',  ( 8.732853799281732776, 31.21183152705961206, 47.04930799450051637 ) ) ;
#364 = DIRECTION ( 'NONE',  ( -1.000000000000000000, 0.000000000000000000, 0.000000000000000000 ) ) ;
#365 = FACE_OUTER_BOUND ( 'NONE', #31359, .T. ) ;
#366 = ORIENTED_EDGE ( 'NONE', *, *, #2554, .T. ) ;
#367 = ORIENTED_EDGE ( 'NONE', *, *, #20650, .T. ) ;
#368 = DIRECTION ( 'NONE',  ( -1.101824276508909887E-16, 1.000000000000000000, -0.000000000000000000 ) ) ;
#369 = CARTESIAN_POINT ( 'NONE',  ( 47.20547626766766314, 27.57451373492759572, 44.97710074790751378 ) ) ;
#370 = EDGE_CURVE ( 'NONE', #26491, #3553, #7732, .T. ) ;
#371 = EDGE_CURVE ( 'NONE', #32203, #7136, #10883, .T. ) ;
#372 = CYLINDRICAL_SURFACE ( 'NONE', #24107, 0.1000000000000012962 ) ;
#373 = DIRECTION ( 'NONE',  ( -1.101824276508909887E-16, 1.000000000000000000, -0.000000000000000000 ) ) ;
#374 = CARTESIAN_POINT ( 'NONE',  ( -25.43703420551703687, 14.86454579224779948, 47.04930799450052348 ) ) ;
#375 = AXIS2_PLACEMENT_3D ( 'NONE', #26320, #1199, #3831 ) ;
#376 = ORIENTED_EDGE ( 'NONE', *, *, #20856, .T. ) ;
#377 = ADVANCED_FACE ( 'NONE', ( #14478 ), #21344, .F. ) ;
#378 = DIRECTION ( 'NONE',  ( 1.313185983435984691E-29, -1.000000000000000000, -3.761114140369702165E-15 ) ) ;
#379 = EDGE_LOOP ( 'NONE', ( #18763, #24620, #4258, #2283 ) ) ;
#380 = CARTESIAN_POINT ( 'NONE',  ( -33.00214402394279745, 14.56454579224780055, 47.04930799450052348 ) ) ;
#381 = LINE ( 'NONE', #32408, #22412 ) ;
#382 = VERTEX_POINT ( 'NONE', #1667 ) ;
#383 = LINE ( 'NONE', #20407, #27548 ) ;
#384 = VECTOR ( 'NONE', #5115, 1000.000000000000114 ) ;
#385 = DIRECTION ( 'NONE',  ( -0.000000000000000000, -1.000000000000000000, 0.000000000000000000 ) ) ;
#386 = CARTESIAN_POINT ( 'NONE',  ( 45.96182992765471909, 25.77822092656774799, 44.82232689504102296 ) ) ;
#387 = EDGE_CURVE ( 'NONE', #272, #6908, #900, .T. ) ;
#388 = CARTESIAN_POINT ( 'NONE',  ( 0.6836613156275053171, 11.92558985988973497, 99.90211174246701376 ) ) ;
#389 = FACE_OUTER_BOUND ( 'NONE', #5612, .T. ) ;
#390 = ORIENTED_EDGE ( 'NONE', *, *, #15587, .T. ) ;
#391 = DIRECTION ( 'NONE',  ( 1.234978253042719660E-16, -1.000000000000000000, -1.109335647967047851E-31 ) ) ;
#393 = DIRECTION ( 'NONE',  ( -0.000000000000000000, -1.000000000000000000, 0.000000000000000000 ) ) ;
#392 = AXIS2_PLACEMENT_3D ( 'NONE', #10385, #24997, #12533 ) ;
#394 = AXIS2_PLACEMENT_3D ( 'NONE', #24259, #4561, #23933 ) ;
#395 = CARTESIAN_POINT ( 'NONE',  ( -37.58300281841709989, 16.01180101885526597, 37.04930799450052348 ) ) ;
#396 = EDGE_CURVE ( 'NONE', #456, #16189, #14313, .T. ) ;
#397 = DIRECTION ( 'NONE',  ( -0.5849755626391566210, -0.8110509177080080789, 7.163884503654653530E-17 ) ) ;
#398 = CARTESIAN_POINT ( 'NONE',  ( 49.32483701613094240, 26.30322093266652672, 45.91328182968236860 ) ) ;
#399 = ORIENTED_EDGE ( 'NONE', *, *, #19336, .T. ) ;
#400 = CARTESIAN_POINT ( 'NONE',  ( -40.68422973805265030, 6.807290781432339344, 39.32248954417796227 ) ) ;
#401 = DIRECTION ( 'NONE',  ( -1.000000000000000000, -1.101824276508909764E-16, 0.000000000000000000 ) ) ;
#402 = VECTOR ( 'NONE', #29431, 1000.000000000000000 ) ;
#403 = ORIENTED_EDGE ( 'NONE', *, *, #28119, .T. ) ;
#404 = DIRECTION ( 'NONE',  ( -1.101824276508909887E-16, 1.000000000000000000, -0.000000000000000000 ) ) ;
#405 = DIRECTION ( 'NONE',  ( -1.000000000000000000, 0.000000000000000000, 0.000000000000000000 ) ) ;
#406 = ADVANCED_FACE ( 'NONE', ( #1831 ), #16107, .T. ) ;
#407 = EDGE_CURVE ( 'NONE', #2291, #14081, #6151, .T. ) ;
#408 = CARTESIAN_POINT ( 'NONE',  ( -38.57628410747783221, -4.281489722201563985, 13.63563177263803894 ) ) ;
#409 = AXIS2_PLACEMENT_3D ( 'NONE', #26501, #24355, #11732 ) ;
#410 = DIRECTION ( 'NONE',  ( -1.000000000000000000, 0.000000000000000000, 0.000000000000000000 ) ) ;
#411 = ADVANCED_FACE ( 'NONE', ( #1587 ), #6674, .T. ) ;
#412 = ORIENTED_EDGE ( 'NONE', *, *, #4110, .T. ) ;
#413 = CARTESIAN_POINT ( 'NONE',  ( -40.08841711228579641, 7.575633567407562552, 60.54930799450051637 ) ) ;
#414 = VERTEX_POINT ( 'NONE', #16673 ) ;
#415 = EDGE_LOOP ( 'NONE', ( #28557, #12550, #27414, #27034 ) ) ;
#416 = ADVANCED_FACE ( 'NONE', ( #13916 ), #14557, .T. ) ;
#417 = VECTOR ( 'NONE', #31540, 999.9999999999998863 ) ;
#418 = AXIS2_PLACEMENT_3D ( 'NONE', #18138, #28164, #5678 ) ;
#419 = CIRCLE ( 'NONE', #21369, 34.00000000000000000 ) ;
#420 = TOROIDAL_SURFACE ( 'NONE', #8282, 12.61792373059898154, 0.1249999999999967248 ) ;
#421 = CARTESIAN_POINT ( 'NONE',  ( 49.52052953415556402, 8.310461108307681144, -3.337848843846767721 ) ) ;
#422 = CARTESIAN_POINT ( 'NONE',  ( -9.880272688099118739, -5.935454078358227470, 107.6100695915628478 ) ) ;
#423 = CARTESIAN_POINT ( 'NONE',  ( -40.11967773290336226, 9.763195579837789850, 38.54930799450052348 ) ) ;
#424 = ORIENTED_EDGE ( 'NONE', *, *, #23042, .F. ) ;
#425 = ORIENTED_EDGE ( 'NONE', *, *, #23403, .T. ) ;
#426 = CARTESIAN_POINT ( 'NONE',  ( -14.15471437217249218, -3.295808585244886402, 97.43646483284780402 ) ) ;
#427 = DIRECTION ( 'NONE',  ( 0.000000000000000000, 0.000000000000000000, 1.000000000000000000 ) ) ;
#428 = CARTESIAN_POINT ( 'NONE',  ( -34.67891837790644871, -3.387818899234932513, 80.71006381137655694 ) ) ;
#429 = EDGE_CURVE ( 'NONE', #5692, #16617, #5104, .T. ) ;
#430 = CARTESIAN_POINT ( 'NONE',  ( 33.50134396954523197, 28.09164230456639544, 47.04930799450051637 ) ) ;
#431 = ORIENTED_EDGE ( 'NONE', *, *, #27668, .F. ) ;
#432 = CARTESIAN_POINT ( 'NONE',  ( -11.20938414847590003, 2.044662169668923113, 99.18612600487385578 ) ) ;
#433 = DIRECTION ( 'NONE',  ( -0.8746197071393805311, 0.4848096202463645921, 8.676864087101954631E-18 ) ) ;
#434 = DIRECTION ( 'NONE',  ( -1.101824276508909887E-16, 1.000000000000000000, -0.000000000000000000 ) ) ;
#435 = EDGE_LOOP ( 'NONE', ( #10154, #19210, #8973, #1783 ) ) ;
#436 = CARTESIAN_POINT ( 'NONE',  ( 47.74496780842034127, 22.93328494799376571, 45.45767897490919296 ) ) ;
#437 = EDGE_CURVE ( 'NONE', #1880, #13059, #22878, .T. ) ;
#438 = LINE ( 'NONE', #30167, #5287 ) ;
#439 = CARTESIAN_POINT ( 'NONE',  ( 21.09785597605719332, -5.986312001188950127, 47.04930799450051637 ) ) ;
#440 = CARTESIAN_POINT ( 'NONE',  ( 21.09785597605719332, -19.93545420775220123, 47.04930799450051637 ) ) ;
#441 = CARTESIAN_POINT ( 'NONE',  ( 49.49063479933183629, 25.21291119454915730, 47.17357720316391578 ) ) ;
#442 = DIRECTION ( 'NONE',  ( -1.101824276508909887E-16, 1.000000000000000000, -0.000000000000000000 ) ) ;
#443 = DIRECTION ( 'NONE',  ( -1.000000000000000000, 0.000000000000000000, 0.000000000000000000 ) ) ;
#444 = ORIENTED_EDGE ( 'NONE', *, *, #23203, .F. ) ;
#445 = CARTESIAN_POINT ( 'NONE',  ( 21.09992658989239089, 28.09164230456639544, 47.04930799450051637 ) ) ;
#446 = AXIS2_PLACEMENT_3D ( 'NONE', #4993, #15161, #2997 ) ;
#447 = ORIENTED_EDGE ( 'NONE', *, *, #29161, .T. ) ;
#448 = AXIS2_PLACEMENT_3D ( 'NONE', #832, #23322, #20846 ) ;
#449 = ADVANCED_FACE ( 'NONE', ( #28848 ), #6361, .F. ) ;
#450 = AXIS2_PLACEMENT_3D ( 'NONE', #12001, #14627, #24141 ) ;
#451 = CARTESIAN_POINT ( 'NONE',  ( -40.90015969217747482, 8.955334253785164123, 57.04930799450051637 ) ) ;
#452 = VECTOR ( 'NONE', #29063, 1000.000000000000000 ) ;
#453 = ORIENTED_EDGE ( 'NONE', *, *, #7859, .T. ) ;
#454 =( BOUNDED_CURVE ( )  B_SPLINE_CURVE ( 2, ( #26958, #22195, #9573, #207, #14829, #27460, #32382, #4482, #2504 ),
 .UNSPECIFIED., .F., .F. ) 
 B_SPLINE_CURVE_WITH_KNOTS ( ( 3, 2, 2, 2, 3 ),
 ( 0.4642857154469869352, 0.4761904761904761640, 0.5000000000000000000, 0.5238095238095238360, 0.5357142868755583320 ),
 .UNSPECIFIED. ) 
 CURVE ( )  GEOMETRIC_REPRESENTATION_ITEM ( )  RATIONAL_B_SPLINE_CURVE ( ( 0.9330127018922200755, 0.9330127084266228721, 1.000000000000000000, 0.8660254037844388186, 1.000000000000000000, 0.8660254037844388186, 1.000000000000000000, 0.9330126953578163906, 0.9330127018922200755 ) ) 
 REPRESENTATION_ITEM ( '' )  );
#455 = CIRCLE ( 'NONE', #23507, 1.290569415042103207 ) ;
#456 = VERTEX_POINT ( 'NONE', #6680 ) ;
#457 = DIRECTION ( 'NONE',  ( -1.101824276508909887E-16, 1.000000000000000000, -0.000000000000000000 ) ) ;
#458 = AXIS2_PLACEMENT_3D ( 'NONE', #16097, #21670, #13655 ) ;
#459 = ORIENTED_EDGE ( 'NONE', *, *, #23712, .T. ) ;
#460 = VERTEX_POINT ( 'NONE', #16358 ) ;
#461 = DIRECTION ( 'NONE',  ( -0.000000000000000000, -1.000000000000000000, -0.000000000000000000 ) ) ;
#462 = AXIS2_PLACEMENT_3D ( 'NONE', #31638, #14558, #26541 ) ;
#463 = CIRCLE ( 'NONE', #20375, 0.3999999999999975797 ) ;
#464 = EDGE_LOOP ( 'NONE', ( #6672, #7321, #19519, #30159 ) ) ;
#465 = AXIS2_PLACEMENT_3D ( 'NONE', #20669, #30697, #8207 ) ;
#466 = DIRECTION ( 'NONE',  ( 0.000000000000000000, 0.000000000000000000, -1.000000000000000000 ) ) ;
#467 = CARTESIAN_POINT ( 'NONE',  ( 47.48234838051382667, 29.55343750245331336, 44.96782160785550531 ) ) ;
#468 = CARTESIAN_POINT ( 'NONE',  ( 52.49730020886497783, -5.900224301042255703, 106.3086101802585404 ) ) ;
#469 = CARTESIAN_POINT ( 'NONE',  ( 45.38854177497844944, 25.52622849631043422, 45.94041160078741370 ) ) ;
#470 = EDGE_LOOP ( 'NONE', ( #9443, #11981, #20479, #1663 ) ) ;
#471 = ORIENTED_EDGE ( 'NONE', *, *, #842, .F. ) ;
#472 = DIRECTION ( 'NONE',  ( -0.8746197071393926326, 0.4848096202463430537, 8.676864087101709653E-18 ) ) ;
#473 = EDGE_LOOP ( 'NONE', ( #24500, #19436, #2603, #32349 ) ) ;
#474 = AXIS2_PLACEMENT_3D ( 'NONE', #27244, #4772, #14789 ) ;
#475 = LINE ( 'NONE', #30528, #22010 ) ;
#476 = CARTESIAN_POINT ( 'NONE',  ( 54.28735269144078757, -4.535950511381776629, 103.8461761130624694 ) ) ;
#477 = CARTESIAN_POINT ( 'NONE',  ( 21.09992658989239089, 25.72145308207319303, 47.04930799450051637 ) ) ;
#478 = LINE ( 'NONE', #7396, #21500 ) ;
#479 = DIRECTION ( 'NONE',  ( -0.9612616959383175619, -0.2756373558170036597, -8.795445018805799373E-19 ) ) ;
#480 = ORIENTED_EDGE ( 'NONE', *, *, #9764, .F. ) ;
#481 = DIRECTION ( 'NONE',  ( -1.101824276508909887E-16, 1.000000000000000000, -0.000000000000000000 ) ) ;
#482 = EDGE_CURVE ( 'NONE', #26626, #155, #15829, .T. ) ;
#483 = ADVANCED_FACE ( 'NONE', ( #7004 ), #4048, .T. ) ;
#484 = CARTESIAN_POINT ( 'NONE',  ( 48.18662509608405742, 25.88284706826093284, 49.18364984542562013 ) ) ;
#485 = ORIENTED_EDGE ( 'NONE', *, *, #11437, .T. ) ;
#486 = CYLINDRICAL_SURFACE ( 'NONE', #31413, 2.499999999999997335 ) ;
#487 = CARTESIAN_POINT ( 'NONE',  ( 21.09785597605719332, 24.86454579224779948, 73.04930799450052348 ) ) ;
#488 = AXIS2_PLACEMENT_3D ( 'NONE', #13721, #10934, #17987 ) ;
#489 = CARTESIAN_POINT ( 'NONE',  ( -31.01957187155556639, 11.71410389684668552, 24.52077559777409732 ) ) ;
#490 = VERTEX_POINT ( 'NONE', #19471 ) ;
#491 = AXIS2_PLACEMENT_3D ( 'NONE', #9371, #11504, #4285 ) ;
#492 = AXIS2_PLACEMENT_3D ( 'NONE', #30621, #8133, #15667 ) ;
#493 = ORIENTED_EDGE ( 'NONE', *, *, #32444, .F. ) ;
#494 = VECTOR ( 'NONE', #29690, 1000.000000000000000 ) ;
#495 = ORIENTED_EDGE ( 'NONE', *, *, #28799, .T. ) ;
#496 = LINE ( 'NONE', #32361, #244 ) ;
#497 = CIRCLE ( 'NONE', #8889, 0.1000000000000018235 ) ;
#498 = CARTESIAN_POINT ( 'NONE',  ( 33.46699938050303302, 38.56284415653841791, 47.04930799450051637 ) ) ;
#499 = FACE_OUTER_BOUND ( 'NONE', #20854, .T. ) ;
#500 = EDGE_LOOP ( 'NONE', ( #31319, #977, #18838, #21612 ) ) ;
#501 = CARTESIAN_POINT ( 'NONE',  ( -29.27613032885505007, -3.086612947480494196, 80.82450247980625591 ) ) ;
#502 = DIRECTION ( 'NONE',  ( 0.000000000000000000, 0.000000000000000000, 1.000000000000000000 ) ) ;
#503 = DIRECTION ( 'NONE',  ( 0.2756373558169932236, -0.9612616959383206705, 3.214564189377567398E-15 ) ) ;
#504 = FACE_OUTER_BOUND ( 'NONE', #24476, .T. ) ;
#505 = AXIS2_PLACEMENT_3D ( 'NONE', #21570, #21893, #31922 ) ;
#506 = CARTESIAN_POINT ( 'NONE',  ( 21.09785597605719332, 14.77310068074637961, 33.81390520620020368 ) ) ;
#507 = DIRECTION ( 'NONE',  ( -0.8746197071393926326, 0.4848096202463430537, 8.676864087101709653E-18 ) ) ;
#508 = FACE_OUTER_BOUND ( 'NONE', #6579, .T. ) ;
#509 = DIRECTION ( 'NONE',  ( 0.000000000000000000, 0.000000000000000000, -1.000000000000000000 ) ) ;
#510 = DIRECTION ( 'NONE',  ( 0.000000000000000000, 0.000000000000000000, 1.000000000000000000 ) ) ;
#511 = DIRECTION ( 'NONE',  ( -1.101824276508909887E-16, 1.000000000000000000, -0.000000000000000000 ) ) ;
#512 = CARTESIAN_POINT ( 'NONE',  ( 49.41945501136223839, 28.46454579807170759, 45.86501535757901848 ) ) ;
#513 = ORIENTED_EDGE ( 'NONE', *, *, #26307, .F. ) ;
#514 = ORIENTED_EDGE ( 'NONE', *, *, #26124, .F. ) ;
#515 = DIRECTION ( 'NONE',  ( -1.224646799147353207E-16, -1.349345573449484691E-32, 1.000000000000000000 ) ) ;
#516 = LINE ( 'NONE', #23004, #15630 ) ;
#517 = CIRCLE ( 'NONE', #11031, 0.1249999999999966416 ) ;
#518 = CIRCLE ( 'NONE', #27799, 12.62506659569710266 ) ;
#519 = EDGE_CURVE ( 'NONE', #12816, #17665, #21603, .T. ) ;
#520 = DIRECTION ( 'NONE',  ( -1.101824276508909887E-16, 1.000000000000000000, -0.000000000000000000 ) ) ;
#521 = EDGE_CURVE ( 'NONE', #13589, #18578, #21569, .T. ) ;
#522 = EDGE_CURVE ( 'NONE', #10117, #4981, #8501, .T. ) ;
#523 = ORIENTED_EDGE ( 'NONE', *, *, #9183, .T. ) ;
#524 = FACE_OUTER_BOUND ( 'NONE', #6231, .T. ) ;
#525 = VECTOR ( 'NONE', #14979, 1000.000000000000114 ) ;
#526 = CARTESIAN_POINT ( 'NONE',  ( 48.22970226119645076, 23.04411657098542676, 46.95810019591398543 ) ) ;
#527 = CARTESIAN_POINT ( 'NONE',  ( -40.19935072163752210, 7.013056605096603668, 39.22629476879045285 ) ) ;
#528 = ORIENTED_EDGE ( 'NONE', *, *, #976, .F. ) ;
#529 = VERTEX_POINT ( 'NONE', #29166 ) ;
#530 = CARTESIAN_POINT ( 'NONE',  ( 21.09785597605719332, 15.56454579224779877, 47.04930799450051637 ) ) ;
#531 = EDGE_CURVE ( 'NONE', #4270, #19118, #14239, .T. ) ;
#532 = CIRCLE ( 'NONE', #18851, 65.75844861871132707 ) ;
#533 = CARTESIAN_POINT ( 'NONE',  ( 45.24946171279598417, 25.70784706826093569, 47.99220971130007030 ) ) ;
#534 = AXIS2_PLACEMENT_3D ( 'NONE', #12377, #29269, #2022 ) ;
#535 = CARTESIAN_POINT ( 'NONE',  ( 47.20547626766766314, 28.18791119454915162, 44.97710074790751378 ) ) ;
#536 = CARTESIAN_POINT ( 'NONE',  ( -39.42404159773660410, -5.935581334357459937, 77.97933121608268436 ) ) ;
#537 = VECTOR ( 'NONE', #21856, 1000.000000000000000 ) ;
#538 = ORIENTED_EDGE ( 'NONE', *, *, #31344, .T. ) ;
#539 = DIRECTION ( 'NONE',  ( 0.000000000000000000, 9.185193130005556732E-17, 1.000000000000000000 ) ) ;
#540 = CARTESIAN_POINT ( 'NONE',  ( 33.46699938050303302, 30.47145308207317882, 47.04930799450050927 ) ) ;
#541 = CIRCLE ( 'NONE', #29390, 39.69941114636694124 ) ;
#542 = CIRCLE ( 'NONE', #23088, 12.27641737965281266 ) ;
#543 = ORIENTED_EDGE ( 'NONE', *, *, #8534, .F. ) ;
#544 = CIRCLE ( 'NONE', #9998, 12.36707279061065101 ) ;
#545 = CARTESIAN_POINT ( 'NONE',  ( 45.36511207810797686, 26.63213139976340571, 45.12672418911604666 ) ) ;
#546 = CARTESIAN_POINT ( 'NONE',  ( 21.09785597605719332, 25.56454579224779877, 73.04930799450052348 ) ) ;
#547 = AXIS2_PLACEMENT_3D ( 'NONE', #22754, #7337, #22261 ) ;
#548 = VECTOR ( 'NONE', #4777, 1000.000000000000000 ) ;
#549 = ADVANCED_FACE ( 'NONE', ( #24556 ), #24396, .T. ) ;
#550 = EDGE_CURVE ( 'NONE', #4992, #17225, #25775, .T. ) ;
#551 = AXIS2_PLACEMENT_3D ( 'NONE', #843, #30240, #2664 ) ;
#552 = ORIENTED_EDGE ( 'NONE', *, *, #8175, .T. ) ;
#553 = DIRECTION ( 'NONE',  ( 0.000000000000000000, 0.000000000000000000, -1.000000000000000000 ) ) ;
#554 = FACE_OUTER_BOUND ( 'NONE', #4438, .T. ) ;
#555 = DIRECTION ( 'NONE',  ( -1.101824276508909887E-16, 1.000000000000000000, -0.000000000000000000 ) ) ;
#556 = DIRECTION ( 'NONE',  ( -1.101824276508909887E-16, 1.000000000000000000, -0.000000000000000000 ) ) ;
#557 = CARTESIAN_POINT ( 'NONE',  ( -40.69574609830256406, 6.786514717574567257, 39.44982113259668211 ) ) ;
#558 = ORIENTED_EDGE ( 'NONE', *, *, #25899, .F. ) ;
#559 = CARTESIAN_POINT ( 'NONE',  ( 73.65314367107050941, 0.8961463385898641443, 79.88877559804848261 ) ) ;
#560 = FACE_OUTER_BOUND ( 'NONE', #13717, .T. ) ;
#561 = AXIS2_PLACEMENT_3D ( 'NONE', #7178, #14738, #4059 ) ;
#562 = CARTESIAN_POINT ( 'NONE',  ( 21.09992658989239089, 25.09143805560860940, 47.04930799450051637 ) ) ;
#563 = CARTESIAN_POINT ( 'NONE',  ( -40.11286833322907341, 2.887657226147505973, 35.84930799450052064 ) ) ;
#564 = DIRECTION ( 'NONE',  ( -2.779292025043186357E-18, 1.288349127009862211E-17, -1.000000000000000000 ) ) ;
#565 = ORIENTED_EDGE ( 'NONE', *, *, #7783, .F. ) ;
#566 = CARTESIAN_POINT ( 'NONE',  ( 49.73184169360587248, 24.88249584856351149, 46.46638833876414765 ) ) ;
#567 = DIRECTION ( 'NONE',  ( 0.000000000000000000, 0.000000000000000000, 1.000000000000000000 ) ) ;
#568 = EDGE_LOOP ( 'NONE', ( #14512, #13383, #25114, #14670 ) ) ;
#569 = CARTESIAN_POINT ( 'NONE',  ( -40.29992972011127961, 7.980862958756435255, 40.07149053519532345 ) ) ;
#570 = ADVANCED_FACE ( 'NONE', ( #26865 ), #5884, .T. ) ;
#571 = CARTESIAN_POINT ( 'NONE',  ( 21.09785597605719332, 7.237299147902269247, 47.04930799450051637 ) ) ;
#572 = DIRECTION ( 'NONE',  ( -0.000000000000000000, -1.000000000000000000, 0.000000000000000000 ) ) ;
#573 = CIRCLE ( 'NONE', #3187, 12.36707279061065101 ) ;
#574 = CARTESIAN_POINT ( 'NONE',  ( 21.09992658989238734, 32.59164230456639899, 47.04930799450051637 ) ) ;
#575 = ORIENTED_EDGE ( 'NONE', *, *, #29988, .T. ) ;
#576 = CARTESIAN_POINT ( 'NONE',  ( 8.823509210239508960, 24.34164230456639544, 47.04930799450051637 ) ) ;
#577 = AXIS2_PLACEMENT_3D ( 'NONE', #24916, #30008, #25240 ) ;
#578 = CIRCLE ( 'NONE', #23109, 12.62506659569710266 ) ;
#579 = EDGE_LOOP ( 'NONE', ( #28790, #1429, #13483, #28688 ) ) ;
#580 = CIRCLE ( 'NONE', #21523, 12.27641737965287660 ) ;
#581 = AXIS2_PLACEMENT_3D ( 'NONE', #5824, #5343, #30613 ) ;
#582 = ORIENTED_EDGE ( 'NONE', *, *, #11719, .F. ) ;
#583 = EDGE_CURVE ( 'NONE', #20144, #2267, #11926, .T. ) ;
#584 = AXIS2_PLACEMENT_3D ( 'NONE', #31750, #4338, #1712 ) ;
#585 = ADVANCED_FACE ( 'NONE', ( #17503 ), #25657, .T. ) ;
#586 = CARTESIAN_POINT ( 'NONE',  ( -40.39697993529618714, 8.288924485351975235, 59.57859731638185963 ) ) ;
#587 = CARTESIAN_POINT ( 'NONE',  ( 47.92322045604424119, 23.24793988701932435, 47.55508673835812772 ) ) ;
#588 = FACE_OUTER_BOUND ( 'NONE', #2822, .T. ) ;
#589 = EDGE_CURVE ( 'NONE', #28974, #110, #24896, .T. ) ;
#590 = EDGE_CURVE ( 'NONE', #21064, #20430, #26831, .T. ) ;
#591 = ORIENTED_EDGE ( 'NONE', *, *, #5712, .T. ) ;
#592 = CARTESIAN_POINT ( 'NONE',  ( -34.60289125444462854, 11.64119122789693961, 41.11328754109207040 ) ) ;
#593 = VERTEX_POINT ( 'NONE', #10739 ) ;
#594 = EDGE_CURVE ( 'NONE', #3250, #802, #20731, .T. ) ;
#595 = CARTESIAN_POINT ( 'NONE',  ( -14.15471437217249218, -3.295808585244886402, 106.8025418868326284 ) ) ;
#596 = CIRCLE ( 'NONE', #27333, 0.1000000000000016709 ) ;
#597 = FACE_OUTER_BOUND ( 'NONE', #26506, .T. ) ;
#598 = CARTESIAN_POINT ( 'NONE',  ( -32.75748891819321074, -0.01103702217111705332, 80.26537595473334363 ) ) ;
#599 = DIRECTION ( 'NONE',  ( -1.101824276508909887E-16, 1.000000000000000000, -0.000000000000000000 ) ) ;
#600 = CIRCLE ( 'NONE', #24713, 1.199999999999999734 ) ;
#601 = ORIENTED_EDGE ( 'NONE', *, *, #27122, .F. ) ;
#602 = CARTESIAN_POINT ( 'NONE',  ( 21.09992658989238734, 32.34143805560860585, 47.04930799450051637 ) ) ;
#603 = CYLINDRICAL_SURFACE ( 'NONE', #6358, 2.500000000000002220 ) ;
#604 = PLANE ( 'NONE',  #25960 ) ;
#605 = DIRECTION ( 'NONE',  ( 0.000000000000000000, -1.000000000000000000, 0.000000000000000000 ) ) ;
#606 = AXIS2_PLACEMENT_3D ( 'NONE', #30004, #14570, #19486 ) ;
#607 = VERTEX_POINT ( 'NONE', #27519 ) ;
#608 = DIRECTION ( 'NONE',  ( 0.000000000000000000, 0.000000000000000000, -1.000000000000000000 ) ) ;
#609 = DIRECTION ( 'NONE',  ( -1.000000000000000000, 0.000000000000000000, 0.000000000000000000 ) ) ;
#610 = FACE_OUTER_BOUND ( 'NONE', #4229, .T. ) ;
#611 = CARTESIAN_POINT ( 'NONE',  ( 21.09992658989238734, 31.34164230456639544, 47.04930799450051637 ) ) ;
#612 = DIRECTION ( 'NONE',  ( 1.234978253042719660E-16, -1.000000000000000000, -1.109335647967047851E-31 ) ) ;
#613 = CARTESIAN_POINT ( 'NONE',  ( 48.78406556707242459, 22.93807716476589675, 47.13688154746046166 ) ) ;
#614 = CARTESIAN_POINT ( 'NONE',  ( -40.46704362897354201, 7.411062716778210380, 35.30013894732506685 ) ) ;
#615 = ORIENTED_EDGE ( 'NONE', *, *, #10584, .T. ) ;
#616 = ADVANCED_FACE ( 'NONE', ( #14724 ), #105, .F. ) ;
#617 = DIRECTION ( 'NONE',  ( -1.000000000000000000, 0.000000000000000000, 0.000000000000000000 ) ) ;
#618 = DIRECTION ( 'NONE',  ( 0.000000000000000000, -0.000000000000000000, -1.000000000000000000 ) ) ;
#619 = ORIENTED_EDGE ( 'NONE', *, *, #25170, .T. ) ;
#620 = EDGE_LOOP ( 'NONE', ( #3859, #30417, #14895, #17526 ) ) ;
#621 = CARTESIAN_POINT ( 'NONE',  ( -9.326276492376491589, 5.308358430270105899, 99.14268250727589304 ) ) ;
#622 = CIRCLE ( 'NONE', #1640, 30.00000000000000000 ) ;
#623 = ORIENTED_EDGE ( 'NONE', *, *, #14827, .F. ) ;
#624 = AXIS2_PLACEMENT_3D ( 'NONE', #9247, #9083, #9410 ) ;
#625 = ADVANCED_FACE ( 'NONE', ( #9634 ), #30756, .F. ) ;
#626 = EDGE_CURVE ( 'NONE', #32106, #27773, #16758, .T. ) ;
#627 = ORIENTED_EDGE ( 'NONE', *, *, #27698, .T. ) ;
#628 = DIRECTION ( 'NONE',  ( -1.101824276508909887E-16, 1.000000000000000000, -0.000000000000000000 ) ) ;
#629 = TOROIDAL_SURFACE ( 'NONE', #20027, 35.50000000000000711, 2.000000000000001776 ) ;
#630 = ADVANCED_FACE ( 'NONE', ( #2411 ), #30939, .T. ) ;
#631 = VERTEX_POINT ( 'NONE', #4872 ) ;
#632 = EDGE_CURVE ( 'NONE', #253, #29537, #8270, .T. ) ;
#633 = AXIS2_PLACEMENT_3D ( 'NONE', #24321, #29422, #19555 ) ;
#634 = DIRECTION ( 'NONE',  ( 0.000000000000000000, 0.000000000000000000, 1.000000000000000000 ) ) ;
#635 = CARTESIAN_POINT ( 'NONE',  ( 33.50134396954526750, 24.84164230456639544, 47.04930799450051637 ) ) ;
#636 = FACE_OUTER_BOUND ( 'NONE', #28736, .T. ) ;
#637 = CARTESIAN_POINT ( 'NONE',  ( 48.37829923888483563, 26.05122849631043280, 45.07556196625585443 ) ) ;
#638 = ORIENTED_EDGE ( 'NONE', *, *, #25897, .T. ) ;
#639 = EDGE_LOOP ( 'NONE', ( #24316, #16511, #2227, #514, #31883, #2232, #9018, #10673 ) ) ;
#640 = DIRECTION ( 'NONE',  ( -2.779292025043186357E-18, 1.288349127009862211E-17, -1.000000000000000000 ) ) ;
#641 = ORIENTED_EDGE ( 'NONE', *, *, #13247, .T. ) ;
#642 = CIRCLE ( 'NONE', #30013, 12.36707279061065101 ) ;
#643 = DIRECTION ( 'NONE',  ( 1.000000000000000000, 0.000000000000000000, 0.000000000000000000 ) ) ;
#644 = CARTESIAN_POINT ( 'NONE',  ( 51.92833871100798149, 4.638969541771024829, 99.33413526210576094 ) ) ;
#645 = DIRECTION ( 'NONE',  ( -1.000000000000000000, -1.101824276508910010E-16, 0.000000000000000000 ) ) ;
#646 = VECTOR ( 'NONE', #22286, 1000.000000000000000 ) ;
#647 = DIRECTION ( 'NONE',  ( 1.234978253042719660E-16, -1.000000000000000000, -1.109335647967047851E-31 ) ) ;
#648 = DIRECTION ( 'NONE',  ( 1.101824276508909887E-16, -1.000000000000000000, 0.000000000000000000 ) ) ;
#649 = VERTEX_POINT ( 'NONE', #13679 ) ;
#650 = DIRECTION ( 'NONE',  ( 1.000000000000000000, 0.000000000000000000, 0.000000000000000000 ) ) ;
#651 = B_SPLINE_CURVE_WITH_KNOTS ( 'NONE', 3,
 ( #1890, #31770, #9282, #29302, #27005, #12076, #21904, #22069 ),
 .UNSPECIFIED., .F., .F.,
 ( 4, 2, 2, 4 ),
 ( 0.000000000000000000, 0.0005021167140330338053, 0.0007531750710495593816, 0.001004233428066084958 ),
 .UNSPECIFIED. ) ;
#652 = DIRECTION ( 'NONE',  ( -0.9612616959383221138, -0.2756373558169876170, 0.000000000000000000 ) ) ;
#653 = CARTESIAN_POINT ( 'NONE',  ( 21.09785597605719332, 6.717634499306958773, 26.77287239547234066 ) ) ;
#654 = CARTESIAN_POINT ( 'NONE',  ( 48.53603344299159517, 25.21410780737789281, 48.64505250420380378 ) ) ;
#655 = VERTEX_POINT ( 'NONE', #26463 ) ;
#656 = DIRECTION ( 'NONE',  ( 7.588956326749211550E-18, -4.206627182996912454E-18, 1.000000000000000000 ) ) ;
#657 = CARTESIAN_POINT ( 'NONE',  ( 21.09992658989238734, 38.56284415653841791, 47.04930799450051637 ) ) ;
#658 = DIRECTION ( 'NONE',  ( 0.000000000000000000, -0.000000000000000000, -1.000000000000000000 ) ) ;
#659 = ORIENTED_EDGE ( 'NONE', *, *, #25819, .T. ) ;
#660 = AXIS2_PLACEMENT_3D ( 'NONE', #13969, #11830, #16569 ) ;
#661 = AXIS2_PLACEMENT_3D ( 'NONE', #13637, #15449, #25779 ) ;
#662 = AXIS2_PLACEMENT_3D ( 'NONE', #7675, #4884, #7833 ) ;
#663 = VERTEX_POINT ( 'NONE', #19058 ) ;
#664 = CIRCLE ( 'NONE', #5918, 5.499019513592785735 ) ;
#665 = VERTEX_POINT ( 'NONE', #23832 ) ;
#666 = DIRECTION ( 'NONE',  ( 0.8746197071393925215, -0.4848096202463429982, -8.676864087101709653E-18 ) ) ;
#667 = DIRECTION ( 'NONE',  ( -1.101824276508909887E-16, 1.000000000000000000, -0.000000000000000000 ) ) ;
#668 = CARTESIAN_POINT ( 'NONE',  ( 48.81241343884743600, 22.91413368675619111, 46.49136847324655974 ) ) ;
#669 = ADVANCED_FACE ( 'NONE', ( #28451, #21524, #18734, #1349, #11366, #13363 ), #3978, .T. ) ;
#670 = ORIENTED_EDGE ( 'NONE', *, *, #24310, .T. ) ;
#671 = EDGE_CURVE ( 'NONE', #28587, #29229, #2630, .T. ) ;
#672 = ADVANCED_FACE ( 'NONE', ( #28602 ), #22535, .T. ) ;
#673 = CARTESIAN_POINT ( 'NONE',  ( -3.635677172050030048, -13.30632128221581212, 97.21573990761679340 ) ) ;
#674 = CARTESIAN_POINT ( 'NONE',  ( 81.53764425905508517, -5.935454354499444918, 15.93786951028389254 ) ) ;
#675 = DIRECTION ( 'NONE',  ( 0.000000000000000000, 0.000000000000000000, -1.000000000000000000 ) ) ;
#676 = DIRECTION ( 'NONE',  ( -1.000000000000000000, 0.000000000000000000, 0.000000000000000000 ) ) ;
#677 = FACE_OUTER_BOUND ( 'NONE', #17845, .T. ) ;
#678 = DIRECTION ( 'NONE',  ( -0.000000000000000000, -1.000000000000000000, 0.000000000000000000 ) ) ;
#679 = DIRECTION ( 'NONE',  ( -1.101824276508909887E-16, 1.000000000000000000, -0.000000000000000000 ) ) ;
#680 = CARTESIAN_POINT ( 'NONE',  ( 33.62634396954528171, 23.59164230456639544, 47.04930799450050927 ) ) ;
#681 = CYLINDRICAL_SURFACE ( 'NONE', #3691, 19.99999999999999645 ) ;
#682 = CIRCLE ( 'NONE', #19008, 12.62506659569710266 ) ;
#683 = CARTESIAN_POINT ( 'NONE',  ( -43.64647580959332629, 1.256990871545142774, 53.54930799450051637 ) ) ;
#684 = VECTOR ( 'NONE', #2246, 1000.000000000000000 ) ;
#685 = CARTESIAN_POINT ( 'NONE',  ( -41.08785830660042393, 9.277514380576530328, 34.69072935073783981 ) ) ;
#686 = ORIENTED_EDGE ( 'NONE', *, *, #11571, .F. ) ;
#687 = ORIENTED_EDGE ( 'NONE', *, *, #2527, .F. ) ;
#688 = CARTESIAN_POINT ( 'NONE',  ( -42.38687957179150345, 4.148162238788004608, 55.04930799450051637 ) ) ;
#689 = FACE_OUTER_BOUND ( 'NONE', #3946, .T. ) ;
#690 = CARTESIAN_POINT ( 'NONE',  ( 51.67081420511490819, 5.053071141216423534, 98.28906612357258155 ) ) ;
#691 = ORIENTED_EDGE ( 'NONE', *, *, #20114, .F. ) ;
#692 = VECTOR ( 'NONE', #11554, 1000.000000000000000 ) ;
#693 = DIRECTION ( 'NONE',  ( -1.224646799147353207E-16, -1.349345573449484691E-32, 1.000000000000000000 ) ) ;
#694 = CARTESIAN_POINT ( 'NONE',  ( 8.823509210239512512, 24.59164230456639544, 47.04930799450051637 ) ) ;
#695 = EDGE_LOOP ( 'NONE', ( #23280, #30142, #10297, #134 ) ) ;
#696 = EDGE_LOOP ( 'NONE', ( #17955, #23554, #928, #3207 ) ) ;
#697 = LINE ( 'NONE', #20231, #30952 ) ;
#698 = CARTESIAN_POINT ( 'NONE',  ( 48.40186567930498285, 26.81618040159426641, 45.03923535223908203 ) ) ;
#699 = CARTESIAN_POINT ( 'NONE',  ( -43.38408989745150990, 1.111547985471239786, 60.54930799450051637 ) ) ;
#700 = CARTESIAN_POINT ( 'NONE',  ( -39.43735134593180902, -5.935500344420906238, 77.98272432681935129 ) ) ;
#701 = EDGE_LOOP ( 'NONE', ( #9890, #30769 ) ) ;
#702 = TOROIDAL_SURFACE ( 'NONE', #15402, 12.40141737965284108, 0.1249999999999997918 ) ;
#703 = VECTOR ( 'NONE', #2894, 1000.000000000000000 ) ;
#704 = DIRECTION ( 'NONE',  ( -1.000000000000000000, 0.000000000000000000, 0.000000000000000000 ) ) ;
#705 = APPLICATION_CONTEXT ( 'automotive_design' ) ;
#706 = CARTESIAN_POINT ( 'NONE',  ( 21.09785597605720753, 14.86454579224779948, 47.04930799450052348 ) ) ;
#707 = EDGE_CURVE ( 'NONE', #18016, #21157, #8900, .T. ) ;
#708 = ORIENTED_EDGE ( 'NONE', *, *, #2194, .T. ) ;
#709 = AXIS2_PLACEMENT_3D ( 'NONE', #18125, #3351, #11077 ) ;
#710 = EDGE_CURVE ( 'NONE', #26545, #16815, #18901, .T. ) ;
#711 = EDGE_CURVE ( 'NONE', #20645, #17250, #26734, .T. ) ;
#712 = CIRCLE ( 'NONE', #19588, 0.6000000000000033085 ) ;
#713 = AXIS2_PLACEMENT_3D ( 'NONE', #13100, #30498, #10310 ) ;
#714 = EDGE_CURVE ( 'NONE', #24189, #27727, #5769, .T. ) ;
#715 = DIRECTION ( 'NONE',  ( 0.000000000000000000, 0.000000000000000000, -1.000000000000000000 ) ) ;
#716 = DIRECTION ( 'NONE',  ( 0.000000000000000000, -1.000000000000000000, 0.000000000000000000 ) ) ;
#717 = ADVANCED_FACE ( 'NONE', ( #868 ), #14154, .T. ) ;
#718 = DIRECTION ( 'NONE',  ( -0.1949050434465282311, 0.6797146636928673713, -0.7071067811865470176 ) ) ;
#719 = ORIENTED_EDGE ( 'NONE', *, *, #22379, .T. ) ;
#720 = DIRECTION ( 'NONE',  ( 0.000000000000000000, 0.000000000000000000, 1.000000000000000000 ) ) ;
#721 = DIRECTION ( 'NONE',  ( 3.761114140369701376E-15, 1.000000000000000000, 0.000000000000000000 ) ) ;
#722 = CARTESIAN_POINT ( 'NONE',  ( 21.09785597605719332, 7.237299147902269247, 27.58963108451947832 ) ) ;
#723 = DIRECTION ( 'NONE',  ( 1.234978253042719660E-16, -1.000000000000000000, -1.109335647967047851E-31 ) ) ;
#724 = DIRECTION ( 'NONE',  ( -7.588956326749211550E-18, 4.206627182996912454E-18, -1.000000000000000000 ) ) ;
#725 = ORIENTED_EDGE ( 'NONE', *, *, #20436, .T. ) ;
#726 = DIRECTION ( 'NONE',  ( 0.000000000000000000, 0.000000000000000000, -1.000000000000000000 ) ) ;
#727 = CARTESIAN_POINT ( 'NONE',  ( 21.09785597605720042, -5.935454207752337119, 114.2361189024295527 ) ) ;
#728 = DIRECTION ( 'NONE',  ( -0.4848096202463391680, -0.8746197071393946310, 0.000000000000000000 ) ) ;
#729 = DIRECTION ( 'NONE',  ( -1.000000000000000000, 0.000000000000000000, 0.000000000000000000 ) ) ;
#730 = AXIS2_PLACEMENT_3D ( 'NONE', #24703, #6978, #12237 ) ;
#731 = CARTESIAN_POINT ( 'NONE',  ( -40.56956524039852496, 6.944624558150293225, 39.15224832543683675 ) ) ;
#732 = ORIENTED_EDGE ( 'NONE', *, *, #12775, .F. ) ;
#733 = CARTESIAN_POINT ( 'NONE',  ( -4.402144023942796025, 14.86454579224779948, 47.04930799450052348 ) ) ;
#734 = DIRECTION ( 'NONE',  ( -0.9612616959383221138, -0.2756373558169876170, 0.000000000000000000 ) ) ;
#735 = ORIENTED_EDGE ( 'NONE', *, *, #14856, .T. ) ;
#736 = CARTESIAN_POINT ( 'NONE',  ( 21.09992658989239089, 26.59184655352419568, 47.04930799450051637 ) ) ;
#737 = FACE_OUTER_BOUND ( 'NONE', #17782, .T. ) ;
#738 = CARTESIAN_POINT ( 'NONE',  ( 47.03138641870017977, 22.86454579224779948, 49.04855133162938330 ) ) ;
#739 = CARTESIAN_POINT ( 'NONE',  ( 50.61496291931489111, 6.662067023026866153, -4.700640528948444086 ) ) ;
#740 = VECTOR ( 'NONE', #4684, 1000.000000000000000 ) ;
#741 = ORIENTED_EDGE ( 'NONE', *, *, #31620, .T. ) ;
#742 = DIRECTION ( 'NONE',  ( -1.000000000000000000, 0.000000000000000000, 0.000000000000000000 ) ) ;
#743 = EDGE_LOOP ( 'NONE', ( #3761, #27026, #1718, #13814 ) ) ;
#744 = EDGE_CURVE ( 'NONE', #30931, #20832, #4, .T. ) ;
#745 = ORIENTED_EDGE ( 'NONE', *, *, #29770, .T. ) ;
#746 = AXIS2_PLACEMENT_3D ( 'NONE', #5481, #25814, #3329 ) ;
#747 = EDGE_CURVE ( 'NONE', #17034, #3050, #21468, .T. ) ;
#748 = DIRECTION ( 'NONE',  ( -1.101824276508909887E-16, 1.000000000000000000, -0.000000000000000000 ) ) ;
#749 = CARTESIAN_POINT ( 'NONE',  ( 33.46699938050304013, 25.21183152705960140, 47.04930799450051637 ) ) ;
#750 = CIRCLE ( 'NONE', #26968, 0.1250000000000001110 ) ;
#751 = LINE ( 'NONE', #3040, #15627 ) ;
#752 = ADVANCED_FACE ( 'NONE', ( #26303 ), #3814, .T. ) ;
#753 = AXIS2_PLACEMENT_3D ( 'NONE', #2967, #13000, #25623 ) ;
#754 = ORIENTED_EDGE ( 'NONE', *, *, #20425, .F. ) ;
#755 = CARTESIAN_POINT ( 'NONE',  ( -35.36966210123092225, 10.42011316249520370, 42.00355930600723298 ) ) ;
#756 = VERTEX_POINT ( 'NONE', #30915 ) ;
#757 = CIRCLE ( 'NONE', #4954, 0.1250000000000001110 ) ;
#758 = DIRECTION ( 'NONE',  ( -0.4544104659272754088, -1.796165296417912609E-16, -0.8907924160295463967 ) ) ;
#759 = PLANE ( 'NONE',  #9679 ) ;
#760 = CARTESIAN_POINT ( 'NONE',  ( -30.89539544812951277, 5.684769981030545871, 77.22998724337006138 ) ) ;
#761 = CARTESIAN_POINT ( 'NONE',  ( 45.18933221474103590, 20.36454579224780304, 43.30797974740836764 ) ) ;
#762 = EDGE_LOOP ( 'NONE', ( #6005, #7688, #10808, #3142 ) ) ;
#763 = DIRECTION ( 'NONE',  ( -1.101824276508909887E-16, 1.000000000000000000, -0.000000000000000000 ) ) ;
#764 = EDGE_LOOP ( 'NONE', ( #11253, #25732, #6784, #15942 ) ) ;
#765 = CARTESIAN_POINT ( 'NONE',  ( 21.09785597605719332, 30.56454579224779522, 47.04930799450051637 ) ) ;
#766 = CARTESIAN_POINT ( 'NONE',  ( 21.09992658989238734, 38.56284415653841791, 47.04930799450051637 ) ) ;
#767 = ORIENTED_EDGE ( 'NONE', *, *, #12081, .F. ) ;
#768 = DIRECTION ( 'NONE',  ( -0.000000000000000000, -1.000000000000000000, -0.000000000000000000 ) ) ;
#769 = CARTESIAN_POINT ( 'NONE',  ( 21.09785597605719332, 17.36451738380053555, 59.83349819502753775 ) ) ;
#770 = DIRECTION ( 'NONE',  ( -1.000000000000000000, -1.101824276508909887E-16, 0.000000000000000000 ) ) ;
#771 = CARTESIAN_POINT ( 'NONE',  ( -40.28779227465695811, 2.984619150196779813, 57.04930799450051637 ) ) ;
#772 = DIRECTION ( 'NONE',  ( -1.224646799147353207E-16, 0.000000000000000000, -1.000000000000000000 ) ) ;
#773 = FACE_OUTER_BOUND ( 'NONE', #16679, .T. ) ;
#774 = ORIENTED_EDGE ( 'NONE', *, *, #26425, .F. ) ;
#775 = DIRECTION ( 'NONE',  ( -0.000000000000000000, -1.000000000000000000, 0.000000000000000000 ) ) ;
#776 = EDGE_CURVE ( 'NONE', #22267, #18307, #27310, .T. ) ;
#777 = VERTEX_POINT ( 'NONE', #26786 ) ;
#778 = AXIS2_PLACEMENT_3D ( 'NONE', #28726, #16083, #11486 ) ;
#779 = ORIENTED_EDGE ( 'NONE', *, *, #30659, .T. ) ;
#780 = CARTESIAN_POINT ( 'NONE',  ( -12.63151429458831743, -2.181906231262896068, 102.0018054233023577 ) ) ;
#781 = AXIS2_PLACEMENT_3D ( 'NONE', #5119, #12351, #22344 ) ;
#782 = EDGE_CURVE ( 'NONE', #6039, #26, #8963, .T. ) ;
#783 = AXIS2_PLACEMENT_3D ( 'NONE', #18069, #31044, #28097 ) ;
#784 = ADVANCED_FACE ( 'NONE', ( #24816 ), #9558, .T. ) ;
#785 = CIRCLE ( 'NONE', #19101, 12.62506659569710266 ) ;
#786 = ORIENTED_EDGE ( 'NONE', *, *, #27395, .F. ) ;
#787 = ORIENTED_EDGE ( 'NONE', *, *, #4701, .T. ) ;
#788 = CARTESIAN_POINT ( 'NONE',  ( 8.732853799281738105, 29.21183152705961206, 47.04930799450051637 ) ) ;
#789 = ADVANCED_FACE ( 'NONE', ( #32368 ), #21852, .F. ) ;
#790 = EDGE_LOOP ( 'NONE', ( #28035, #4033, #21933, #28843 ) ) ;
#791 = VECTOR ( 'NONE', #10665, 1000.000000000000114 ) ;
#792 = CARTESIAN_POINT ( 'NONE',  ( 21.09992658989238734, 30.96183152705961206, 47.04930799450051637 ) ) ;
#793 = DIRECTION ( 'NONE',  ( 0.000000000000000000, 0.000000000000000000, -1.000000000000000000 ) ) ;
#794 = CARTESIAN_POINT ( 'NONE',  ( 52.07598125554711999, -5.935454207752202116, 106.6682925056943958 ) ) ;
#795 = TOROIDAL_SURFACE ( 'NONE', #23343, 14.00178401536290806, 0.5000000000000004441 ) ;
#796 = CARTESIAN_POINT ( 'NONE',  ( 45.28286642839709231, 28.44289516297709142, 47.97516931882780966 ) ) ;
#797 = ORIENTED_EDGE ( 'NONE', *, *, #29579, .T. ) ;
#798 = ORIENTED_EDGE ( 'NONE', *, *, #992, .F. ) ;
#800 = CARTESIAN_POINT ( 'NONE',  ( 21.09992658989239089, 28.34164230456639544, 47.04930799450051637 ) ) ;
#799 = AXIS2_PLACEMENT_3D ( 'NONE', #9111, #29139, #16645 ) ;
#801 = AXIS2_PLACEMENT_3D ( 'NONE', #9771, #4184, #12401 ) ;
#802 = VERTEX_POINT ( 'NONE', #6762 ) ;
#803 = CARTESIAN_POINT ( 'NONE',  ( 41.78490141557333004, 11.92558985988973497, 99.79672416560200077 ) ) ;
#804 = CIRCLE ( 'NONE', #9739, 1.199999999999999734 ) ;
#805 = CARTESIAN_POINT ( 'NONE',  ( -40.60722745863126448, 9.415333058485025219, 39.54930799450052348 ) ) ;
#806 = DIRECTION ( 'NONE',  ( 0.000000000000000000, 0.000000000000000000, 1.000000000000000000 ) ) ;
#807 = CARTESIAN_POINT ( 'NONE',  ( 33.46699938050304013, 27.47145308207318593, 47.04930799450050927 ) ) ;
#808 = DIRECTION ( 'NONE',  ( 0.8643320973212949010, -0.2419218955996661480, -0.4409124878812526460 ) ) ;
#809 = EDGE_CURVE ( 'NONE', #2831, #29664, #6340, .T. ) ;
#810 = ORIENTED_EDGE ( 'NONE', *, *, #8618, .F. ) ;
#811 = CARTESIAN_POINT ( 'NONE',  ( -40.08841711228579641, 7.575633567407562552, 53.64930799450051779 ) ) ;
#812 = CARTESIAN_POINT ( 'NONE',  ( 21.09992658989238734, 31.09164230456639544, 47.04930799450051637 ) ) ;
#813 = ADVANCED_FACE ( 'NONE', ( #24319 ), #1838, .T. ) ;
#814 = CYLINDRICAL_SURFACE ( 'NONE', #19867, 2.499999999999998668 ) ;
#815 = CARTESIAN_POINT ( 'NONE',  ( 46.99023568444673771, 26.52451373492759856, 49.12151524109405898 ) ) ;
#816 = EDGE_LOOP ( 'NONE', ( #11067, #9782, #2400, #22463 ) ) ;
#817 = DIRECTION ( 'NONE',  ( -0.000000000000000000, -1.000000000000000000, 0.000000000000000000 ) ) ;
#818 = CARTESIAN_POINT ( 'NONE',  ( 46.05411555189323991, 22.80670247275590867, 45.00323677929942079 ) ) ;
#819 = ADVANCED_FACE ( 'NONE', ( #7090 ), #4794, .F. ) ;
#820 = EDGE_CURVE ( 'NONE', #7388, #14290, #12583, .T. ) ;
#821 = ORIENTED_EDGE ( 'NONE', *, *, #29239, .F. ) ;
#822 = AXIS2_PLACEMENT_3D ( 'NONE', #1912, #19630, #21767 ) ;
#823 = AXIS2_PLACEMENT_3D ( 'NONE', #3985, #9075, #29100 ) ;
#824 =( GEOMETRIC_REPRESENTATION_CONTEXT ( 3 ) GLOBAL_UNCERTAINTY_ASSIGNED_CONTEXT ( ( #14065 ) ) GLOBAL_UNIT_ASSIGNED_CONTEXT ( ( #9888, #7594, #28105 ) ) REPRESENTATION_CONTEXT ( 'NONE', 'WORKASPACE' ) );
#825 = ORIENTED_EDGE ( 'NONE', *, *, #300, .F. ) ;
#826 = ORIENTED_EDGE ( 'NONE', *, *, #5317, .F. ) ;
#827 = CARTESIAN_POINT ( 'NONE',  ( 48.01680169312755453, 22.93807716476589675, 45.63279442905645311 ) ) ;
#828 = CARTESIAN_POINT ( 'NONE',  ( -44.53739698818294102, -4.628387878568079650, 52.16470011384033967 ) ) ;
#829 = DIRECTION ( 'NONE',  ( -1.224646799147353207E-16, 0.000000000000000000, -1.000000000000000000 ) ) ;
#830 = VECTOR ( 'NONE', #28891, 1000.000000000000000 ) ;
#831 = ORIENTED_EDGE ( 'NONE', *, *, #27020, .F. ) ;
#832 = CARTESIAN_POINT ( 'NONE',  ( 47.09785597605719687, 25.56454579224779877, 47.04930799450042400 ) ) ;
#833 = CARTESIAN_POINT ( 'NONE',  ( -42.22510282758591416, 14.66434666503944051, 60.44930799450051495 ) ) ;
#834 = DIRECTION ( 'NONE',  ( 0.000000000000000000, 0.000000000000000000, -1.000000000000000000 ) ) ;
#835 = ORIENTED_EDGE ( 'NONE', *, *, #12736, .T. ) ;
#836 = DIRECTION ( 'NONE',  ( 0.000000000000000000, 0.000000000000000000, -1.000000000000000000 ) ) ;
#837 = CARTESIAN_POINT ( 'NONE',  ( -38.10732830366966084, -5.882756053366322568, 78.42076464377196032 ) ) ;
#838 = DIRECTION ( 'NONE',  ( 0.000000000000000000, 0.000000000000000000, -1.000000000000000000 ) ) ;
#839 = DIRECTION ( 'NONE',  ( -0.9612616959383193382, -0.2756373558169973870, -8.795445018804928853E-19 ) ) ;
#840 = DIRECTION ( 'NONE',  ( -0.000000000000000000, 1.000000000000000000, -0.000000000000000000 ) ) ;
#841 = CARTESIAN_POINT ( 'NONE',  ( -40.60722745863126448, 9.415333058485023443, 38.60788663826321709 ) ) ;
#842 = EDGE_CURVE ( 'NONE', #16822, #14722, #27927, .T. ) ;
#843 = CARTESIAN_POINT ( 'NONE',  ( -40.50720532202722524, 7.584939507552746818, 54.01510846932454513 ) ) ;
#844 = ORIENTED_EDGE ( 'NONE', *, *, #2452, .T. ) ;
#845 = ORIENTED_EDGE ( 'NONE', *, *, #14632, .T. ) ;
#846 = CARTESIAN_POINT ( 'NONE',  ( 75.12562691325334185, -13.30632128221581212, 61.52060788219942822 ) ) ;
#847 = CARTESIAN_POINT ( 'NONE',  ( 61.09785597605719687, 13.86454579224779948, 47.04930799450051637 ) ) ;
#848 = EDGE_CURVE ( 'NONE', #30210, #4768, #22672, .T. ) ;
#849 = CARTESIAN_POINT ( 'NONE',  ( 50.74134730670688498, 6.496515553941725862, 97.90908627297329758 ) ) ;
#850 = ORIENTED_EDGE ( 'NONE', *, *, #29495, .F. ) ;
#851 = CARTESIAN_POINT ( 'NONE',  ( 21.09785597605720042, -14.04221034894631615, -11.81388374861560386 ) ) ;
#852 = CARTESIAN_POINT ( 'NONE',  ( 45.96182992765472619, 28.57822092656774160, 44.82232689504103007 ) ) ;
#853 = ORIENTED_EDGE ( 'NONE', *, *, #19976, .F. ) ;
#854 = DIRECTION ( 'NONE',  ( -0.2756373558170082672, 0.9612616959383162296, 0.000000000000000000 ) ) ;
#855 = CARTESIAN_POINT ( 'NONE',  ( 49.41945501136223839, 28.46454579807170759, 45.86501535757901848 ) ) ;
#856 = CARTESIAN_POINT ( 'NONE',  ( 47.20547626766765603, 29.58791119454915020, 44.97710074790751378 ) ) ;
#857 = ADVANCED_FACE ( 'NONE', ( #10211 ), #16281, .F. ) ;
#858 = CIRCLE ( 'NONE', #22872, 12.62506659569710266 ) ;
#859 = CARTESIAN_POINT ( 'NONE',  ( -39.50719276739945229, -5.935457263800389960, 77.87558390080170057 ) ) ;
#860 = EDGE_CURVE ( 'NONE', #13790, #27623, #578, .T. ) ;
#861 = EDGE_LOOP ( 'NONE', ( #24263, #7176, #5578, #9165 ) ) ;
#862 = CARTESIAN_POINT ( 'NONE',  ( -39.58809650894544774, 2.596771453999702661, 45.54930799450051637 ) ) ;
#863 = CIRCLE ( 'NONE', #13468, 0.1250000000000001110 ) ;
#864 = DIRECTION ( 'NONE',  ( -0.4848096202463430537, -0.8746197071393926326, -9.920727850371701658E-18 ) ) ;
#865 = ORIENTED_EDGE ( 'NONE', *, *, #20443, .F. ) ;
#866 = CARTESIAN_POINT ( 'NONE',  ( 44.21498992391908445, 26.71753733014355703, 46.89958605635242606 ) ) ;
#867 = FACE_OUTER_BOUND ( 'NONE', #19263, .T. ) ;
#868 = FACE_OUTER_BOUND ( 'NONE', #17054, .T. ) ;
#869 = AXIS2_PLACEMENT_3D ( 'NONE', #29737, #14966, #29905 ) ;
#870 = ORIENTED_EDGE ( 'NONE', *, *, #17750, .F. ) ;
#871 = CARTESIAN_POINT ( 'NONE',  ( -41.07560527903737579, 9.385057823277964673, 38.64930799450052490 ) ) ;
#872 = CARTESIAN_POINT ( 'NONE',  ( 47.79865503179234310, 9.702389020015065313, 97.51081847724526597 ) ) ;
#873 = SPHERICAL_SURFACE ( 'NONE', #13622, 0.1000000000000000056 ) ;
#874 = CARTESIAN_POINT ( 'NONE',  ( -5.602943079677954685, 9.702389020015065313, 98.41455612196619995 ) ) ;
#875 = ORIENTED_EDGE ( 'NONE', *, *, #31987, .T. ) ;
#876 = DIRECTION ( 'NONE',  ( 0.8746197071393926326, -0.4848096202463430537, -8.676864087101709653E-18 ) ) ;
#877 = CARTESIAN_POINT ( 'NONE',  ( -39.67555847965937943, 2.645252416024337361, 45.14930799450051779 ) ) ;
#878 = CARTESIAN_POINT ( 'NONE',  ( 67.13598395589038148, 13.95840365082257151, 47.04930799450051637 ) ) ;
#879 = CARTESIAN_POINT ( 'NONE',  ( -40.13135354151336998, 6.899777549362540618, 34.56234534340313758 ) ) ;
#880 = CARTESIAN_POINT ( 'NONE',  ( 76.87534014094269708, -3.386628651589064898, 80.70757180512225659 ) ) ;
#881 = ORIENTED_EDGE ( 'NONE', *, *, #31352, .F. ) ;
#882 = DIRECTION ( 'NONE',  ( -0.7141240004913198547, 0.3958453973320100738, -0.5773502691896283956 ) ) ;
#883 = CARTESIAN_POINT ( 'NONE',  ( 21.09785597605719332, 30.56454579224779522, 47.04930799450051637 ) ) ;
#884 = CARTESIAN_POINT ( 'NONE',  ( 47.09785597605719687, 25.16454579224780019, 47.04930799450078638 ) ) ;
#885 = ORIENTED_EDGE ( 'NONE', *, *, #17568, .F. ) ;
#886 = FACE_OUTER_BOUND ( 'NONE', #15333, .T. ) ;
#887 = DIRECTION ( 'NONE',  ( 0.6184495258776567805, -0.3428121700606641120, -0.7071067811865474617 ) ) ;
#888 = CIRCLE ( 'NONE', #30776, 12.27641737965288726 ) ;
#889 = DIRECTION ( 'NONE',  ( -1.000000000000000000, 0.000000000000000000, 0.000000000000000000 ) ) ;
#890 = EDGE_CURVE ( 'NONE', #8606, #20520, #3192, .T. ) ;
#891 = CARTESIAN_POINT ( 'NONE',  ( 49.40414881150629611, 22.86454579224779948, 47.16908566558144855 ) ) ;
#892 = ADVANCED_FACE ( 'NONE', ( #20693 ), #17421, .F. ) ;
#893 = VERTEX_POINT ( 'NONE', #12685 ) ;
#894 = EDGE_CURVE ( 'NONE', #7034, #9970, #12106, .T. ) ;
#895 = DIRECTION ( 'NONE',  ( -0.8746197071393926326, 0.4848096202463430537, 8.676864087101709653E-18 ) ) ;
#896 = ORIENTED_EDGE ( 'NONE', *, *, #11025, .F. ) ;
#897 = CIRCLE ( 'NONE', #5101, 0.09999999999999815981 ) ;
#898 = ORIENTED_EDGE ( 'NONE', *, *, #17976, .F. ) ;
#899 = AXIS2_PLACEMENT_3D ( 'NONE', #30878, #1312, #5929 ) ;
#900 = CIRCLE ( 'NONE', #31833, 12.62506659569710266 ) ;
#901 = CARTESIAN_POINT ( 'NONE',  ( 49.32483701613094240, 27.70322093266652175, 45.91328182968236860 ) ) ;
#902 = CARTESIAN_POINT ( 'NONE',  ( -36.15844848744088580, -5.643691937041874773, 79.05968474335206508 ) ) ;
#903 = CARTESIAN_POINT ( 'NONE',  ( 8.573509210239501854, 23.59164230456639544, 47.04930799450051637 ) ) ;
#904 = TOROIDAL_SURFACE ( 'NONE', #1959, 20.49999999999999645, 0.9999999999999974465 ) ;
#905 = ORIENTED_EDGE ( 'NONE', *, *, #16478, .F. ) ;
#906 = LINE ( 'NONE', #10621, #25046 ) ;
#907 = ORIENTED_EDGE ( 'NONE', *, *, #16677, .T. ) ;
#908 = CARTESIAN_POINT ( 'NONE',  ( 46.53577443378190281, 23.10527845304106620, 47.02011620365084354 ) ) ;
#909 = DIRECTION ( 'NONE',  ( 2.779292025043186357E-18, -1.288349127009862211E-17, 1.000000000000000000 ) ) ;
#910 = DIRECTION ( 'NONE',  ( -1.000000000000000000, -1.101824276508909764E-16, 0.000000000000000000 ) ) ;
#911 = AXIS2_PLACEMENT_3D ( 'NONE', #20744, #10594, #20099 ) ;
#912 = CARTESIAN_POINT ( 'NONE',  ( -40.63136629056263160, 9.462201496834364178, 35.46931185928404773 ) ) ;
#913 = EDGE_CURVE ( 'NONE', #25724, #15900, #27600, .T. ) ;
#914 = ORIENTED_EDGE ( 'NONE', *, *, #23784, .T. ) ;
#915 = DIRECTION ( 'NONE',  ( -0.2756373558169954441, 0.9612616959383198934, -1.479773560108263451E-16 ) ) ;
#916 = EDGE_LOOP ( 'NONE', ( #23883, #16207, #15273, #30027 ) ) ;
#917 = CARTESIAN_POINT ( 'NONE',  ( 33.50134396954528171, 23.84164230456639544, 47.04930799450051637 ) ) ;
#918 = DIRECTION ( 'NONE',  ( -1.000000000000000000, 0.000000000000000000, 0.000000000000000000 ) ) ;
#919 = ORIENTED_EDGE ( 'NONE', *, *, #1291, .F. ) ;
#920 = PLANE ( 'NONE',  #8989 ) ;
#921 = CARTESIAN_POINT ( 'NONE',  ( 49.40414881150629611, 19.96454579224779380, 47.16908566558144855 ) ) ;
#922 = CARTESIAN_POINT ( 'NONE',  ( 21.09992658989239089, 28.46664230456639899, 47.04930799450051637 ) ) ;
#923 = CARTESIAN_POINT ( 'NONE',  ( 21.09785597605719332, -5.935454207752083988, -18.70914062421081425 ) ) ;
#924 = CARTESIAN_POINT ( 'NONE',  ( 33.37634396954526750, 25.09164230456639899, 47.04930799450051637 ) ) ;
#925 = ORIENTED_EDGE ( 'NONE', *, *, #15668, .F. ) ;
#926 = DIRECTION ( 'NONE',  ( -1.101824276508909887E-16, 1.000000000000000000, -0.000000000000000000 ) ) ;
#927 = DIRECTION ( 'NONE',  ( 0.000000000000000000, 0.000000000000000000, 1.000000000000000000 ) ) ;
#928 = ORIENTED_EDGE ( 'NONE', *, *, #23814, .T. ) ;
#929 = CARTESIAN_POINT ( 'NONE',  ( 33.46699938050304013, 28.72145308207318237, 47.04930799450050927 ) ) ;
#930 = CYLINDRICAL_SURFACE ( 'NONE', #149, 0.1000000000000028644 ) ;
#931 = EDGE_CURVE ( 'NONE', #23264, #20995, #14972, .T. ) ;
#932 = ORIENTED_EDGE ( 'NONE', *, *, #25282, .F. ) ;
#933 = EDGE_CURVE ( 'NONE', #14507, #21242, #22832, .T. ) ;
#934 = ORIENTED_EDGE ( 'NONE', *, *, #16622, .F. ) ;
#935 = CARTESIAN_POINT ( 'NONE',  ( -12.30971848159242121, -4.161241697801305151, 103.4774498197331667 ) ) ;
#936 = EDGE_CURVE ( 'NONE', #20447, #14398, #15132, .T. ) ;
#937 = AXIS2_PLACEMENT_3D ( 'NONE', #13718, #3858, #21243 ) ;
#938 = UNCERTAINTY_MEASURE_WITH_UNIT (LENGTH_MEASURE( 1.000000000000000082E-05 ), #1682, 'distance_accuracy_value', 'NONE');
#939 = AXIS2_PLACEMENT_3D ( 'NONE', #4537, #12591, #24892 ) ;
#940 = ORIENTED_EDGE ( 'NONE', *, *, #29043, .F. ) ;
#941 = CIRCLE ( 'NONE', #31356, 12.62506659569710266 ) ;
#942 = AXIS2_PLACEMENT_3D ( 'NONE', #17620, #12882, #24854 ) ;
#943 = ORIENTED_EDGE ( 'NONE', *, *, #25202, .T. ) ;
#944 = DIRECTION ( 'NONE',  ( -0.3958453973319808195, -0.7141240004913296247, 0.5773502691896363892 ) ) ;
#945 = ORIENTED_EDGE ( 'NONE', *, *, #16041, .F. ) ;
#946 = LINE ( 'NONE', #24559, #9376 ) ;
#947 = DIRECTION ( 'NONE',  ( -1.101824276508909887E-16, 1.000000000000000000, -0.000000000000000000 ) ) ;
#948 = CYLINDRICAL_SURFACE ( 'NONE', #21641, 0.1000000000000006301 ) ;
#949 = CARTESIAN_POINT ( 'NONE',  ( 48.80717017713595141, 25.87622849631043920, 48.15820438821415195 ) ) ;
#950 = ADVANCED_FACE ( 'NONE', ( #2490 ), #25622, .F. ) ;
#951 = ORIENTED_EDGE ( 'NONE', *, *, #18687, .F. ) ;
#952 = VECTOR ( 'NONE', #28444, 1000.000000000000114 ) ;
#953 = EDGE_LOOP ( 'NONE', ( #21634, #23029, #10824, #21413 ) ) ;
#954 = DIRECTION ( 'NONE',  ( 1.188208965918165239E-16, 1.880121038077813132E-16, 1.000000000000000000 ) ) ;
#955 = EDGE_CURVE ( 'NONE', #13402, #21770, #9293, .T. ) ;
#956 = CIRCLE ( 'NONE', #32436, 40.00000000000000711 ) ;
#957 = EDGE_LOOP ( 'NONE', ( #2500, #18429, #8067, #18740 ) ) ;
#958 = AXIS2_PLACEMENT_3D ( 'NONE', #20676, #5430, #2476 ) ;
#959 = CARTESIAN_POINT ( 'NONE',  ( -43.64073206722599707, 1.267352857069778516, 34.64930799450052490 ) ) ;
#960 = CARTESIAN_POINT ( 'NONE',  ( 47.79865503179234310, 9.702389020015065313, 98.41455612196619995 ) ) ;
#961 = CARTESIAN_POINT ( 'NONE',  ( 48.99785660077486682, 22.86454579224780304, 47.79536686733754181 ) ) ;
#962 = AXIS2_PLACEMENT_3D ( 'NONE', #395, #15181, #10105 ) ;
#963 = AXIS2_PLACEMENT_3D ( 'NONE', #7486, #14707, #4524 ) ;
#964 = DIRECTION ( 'NONE',  ( 0.9612616959383207815, 0.2756373558169926685, 8.795445018804289444E-19 ) ) ;
#965 = CARTESIAN_POINT ( 'NONE',  ( 33.50134396954524618, 26.59164230456639899, 47.04930799450051637 ) ) ;
#966 = EDGE_LOOP ( 'NONE', ( #8106, #14529, #18674, #26585 ) ) ;
#967 = FACE_BOUND ( 'NONE', #5368, .T. ) ;
#968 = CARTESIAN_POINT ( 'NONE',  ( 21.09992658989239089, 26.59164230456639899, 47.04930799450051637 ) ) ;
#969 = CARTESIAN_POINT ( 'NONE',  ( 48.96093869543725674, 24.86454579224779593, 50.70155699761480861 ) ) ;
#970 = AXIS2_PLACEMENT_3D ( 'NONE', #17910, #29911, #17740 ) ;
#971 = CARTESIAN_POINT ( 'NONE',  ( 45.96182992765471909, 25.77822092656774799, 44.82232689504102296 ) ) ;
#972 = CARTESIAN_POINT ( 'NONE',  ( 48.83862994770794330, 26.64118040159426570, 48.17861352429476796 ) ) ;
#973 = ORIENTED_EDGE ( 'NONE', *, *, #15561, .T. ) ;
#974 = CARTESIAN_POINT ( 'NONE',  ( -41.77464577679392477, 3.808795504615564820, 61.94930799450052206 ) ) ;
#975 = CARTESIAN_POINT ( 'NONE',  ( -40.59307404304409772, 7.534955414378393002, 53.83739922958098134 ) ) ;
#976 = EDGE_CURVE ( 'NONE', #27344, #24538, #26061, .T. ) ;
#977 = ORIENTED_EDGE ( 'NONE', *, *, #26692, .T. ) ;
#978 = AXIS2_PLACEMENT_3D ( 'NONE', #23436, #30997, #9473 ) ;
#979 = VECTOR ( 'NONE', #254, 1000.000000000000000 ) ;
#980 = VECTOR ( 'NONE', #29388, 1000.000000000000114 ) ;
#981 = EDGE_LOOP ( 'NONE', ( #5763, #6597, #9287, #17362, #5522 ) ) ;
#982 = EDGE_CURVE ( 'NONE', #12544, #14642, #19707, .T. ) ;
#983 = CARTESIAN_POINT ( 'NONE',  ( 45.96182992765471909, 25.90087065737812466, 44.82232689504102296 ) ) ;
#984 = CARTESIAN_POINT ( 'NONE',  ( 21.09992658989239089, 25.34184655352419213, 47.04930799450051637 ) ) ;
#985 = DIRECTION ( 'NONE',  ( -1.000000000000000000, 0.000000000000000000, 0.000000000000000000 ) ) ;
#986 = ADVANCED_FACE ( 'NONE', ( #5446, #504 ), #31042, .F. ) ;
#987 = AXIS2_PLACEMENT_3D ( 'NONE', #4935, #14949, #9537 ) ;
#988 = EDGE_LOOP ( 'NONE', ( #24346, #13936, #21488, #25413 ) ) ;
#989 = CARTESIAN_POINT ( 'NONE',  ( -29.06857593705904108, -13.30632128221581212, 71.78284114260779347 ) ) ;
#990 = DIRECTION ( 'NONE',  ( 0.2756373558169961657, -0.9612616959383196713, 1.479773560108262218E-16 ) ) ;
#991 = CARTESIAN_POINT ( 'NONE',  ( 46.99747725352182925, 22.88065857334294861, 48.98207832244369087 ) ) ;
#992 = EDGE_CURVE ( 'NONE', #10697, #9081, #30273, .T. ) ;
#993 = ORIENTED_EDGE ( 'NONE', *, *, #1703, .F. ) ;
#994 = CARTESIAN_POINT ( 'NONE',  ( 21.09785597605719332, 17.16451738380053271, 59.83349819502753775 ) ) ;
#995 = ADVANCED_FACE ( 'NONE', ( #18386 ), #31829, .T. ) ;
#996 = ORIENTED_EDGE ( 'NONE', *, *, #8934, .T. ) ;
#997 = DIRECTION ( 'NONE',  ( -1.101824276508909887E-16, 1.000000000000000000, -0.000000000000000000 ) ) ;
#998 = EDGE_CURVE ( 'NONE', #28668, #3984, #20301, .T. ) ;
#999 = CARTESIAN_POINT ( 'NONE',  ( 21.09785597605719332, 12.39166260509097484, 47.04930799450051637 ) ) ;
#1000 = DIRECTION ( 'NONE',  ( -1.101824276508909887E-16, 1.000000000000000000, -0.000000000000000000 ) ) ;
#1001 = CARTESIAN_POINT ( 'NONE',  ( 8.732853799281734553, 38.56284415653841791, 47.04930799450051637 ) ) ;
#1002 = FACE_OUTER_BOUND ( 'NONE', #23225, .T. ) ;
#1003 = ORIENTED_EDGE ( 'NONE', *, *, #7201, .T. ) ;
#1004 = ORIENTED_EDGE ( 'NONE', *, *, #5227, .F. ) ;
#1005 = DIRECTION ( 'NONE',  ( -0.2756373558169945559, 0.9612616959383202264, 0.000000000000000000 ) ) ;
#1006 = TOROIDAL_SURFACE ( 'NONE', #23517, 12.40141737965281088, 0.1249999999999987788 ) ;
#1007 = CARTESIAN_POINT ( 'NONE',  ( -58.11219453028166981, -15.93545420775219945, 49.54930799450023926 ) ) ;
#1008 = VECTOR ( 'NONE', #28478, 1000.000000000000000 ) ;
#1009 = CARTESIAN_POINT ( 'NONE',  ( -10.63512168728995100, -5.773219817368564044, 105.6277383086626145 ) ) ;
#1010 = EDGE_LOOP ( 'NONE', ( #6505, #21848, #23375, #10940 ) ) ;
#1011 = CARTESIAN_POINT ( 'NONE',  ( 21.09785597605719687, 43.75535478762431296, 76.06768081105269630 ) ) ;
#1012 = CARTESIAN_POINT ( 'NONE',  ( -40.07989290236489666, 6.890692649785590262, 39.18555621625623075 ) ) ;
#1013 = VERTEX_POINT ( 'NONE', #8550 ) ;
#1014 = CARTESIAN_POINT ( 'NONE',  ( -40.50792392543508669, 7.569031714560849444, 60.24719206080857958 ) ) ;
#1015 = CARTESIAN_POINT ( 'NONE',  ( 48.73570333863616355, 27.12287913140504259, 44.52463952959527660 ) ) ;
#1016 = EDGE_CURVE ( 'NONE', #17357, #30739, #19231, .T. ) ;
#1017 = AXIS2_PLACEMENT_3D ( 'NONE', #653, #5424, #10682 ) ;
#1018 = DIRECTION ( 'NONE',  ( 1.000000000000000000, -3.761114140369701376E-15, 0.000000000000000000 ) ) ;
#1019 = AXIS2_PLACEMENT_3D ( 'NONE', #16547, #14431, #19660 ) ;
#1020 = ORIENTED_EDGE ( 'NONE', *, *, #10985, .T. ) ;
#1021 = ADVANCED_FACE ( 'NONE', ( #1151 ), #13482, .T. ) ;
#1022 = CARTESIAN_POINT ( 'NONE',  ( -40.22018024869837660, 7.672350704644241404, 53.87859731638185679 ) ) ;
#1023 = DIRECTION ( 'NONE',  ( -0.000000000000000000, -1.000000000000000000, 0.000000000000000000 ) ) ;
#1024 = TOROIDAL_SURFACE ( 'NONE', #17777, 12.61792373059896732, 0.1249999999999974604 ) ;
#1025 = AXIS2_PLACEMENT_3D ( 'NONE', #1697, #21378, #8608 ) ;
#1026 = EDGE_CURVE ( 'NONE', #18648, #5411, #27388, .T. ) ;
#1027 = VERTEX_POINT ( 'NONE', #26268 ) ;
#1028 = DIRECTION ( 'NONE',  ( -0.000000000000000000, 1.000000000000000000, -0.000000000000000000 ) ) ;
#1029 = DIRECTION ( 'NONE',  ( 0.000000000000000000, -1.000000000000000000, -1.251509963831984395E-16 ) ) ;
#1030 = DIRECTION ( 'NONE',  ( -1.000000000000000000, 0.000000000000000000, 0.000000000000000000 ) ) ;
#1031 = EDGE_CURVE ( 'NONE', #23957, #25242, #18699, .T. ) ;
#1032 = AXIS2_PLACEMENT_3D ( 'NONE', #27247, #9702, #19534 ) ;
#1033 = ORIENTED_EDGE ( 'NONE', *, *, #20379, .T. ) ;
#1034 = VECTOR ( 'NONE', #9749, 1000.000000000000000 ) ;
#1035 = DIRECTION ( 'NONE',  ( -1.101824276508909887E-16, 1.000000000000000000, -0.000000000000000000 ) ) ;
#1036 = EDGE_CURVE ( 'NONE', #1567, #17902, #25780, .T. ) ;
#1037 = DIRECTION ( 'NONE',  ( -1.101824276508909887E-16, 1.000000000000000000, -0.000000000000000000 ) ) ;
#1038 = CARTESIAN_POINT ( 'NONE',  ( -63.90214402394282445, -3.935454207752203892, 40.04930799450051637 ) ) ;
#1039 = AXIS2_PLACEMENT_3D ( 'NONE', #6070, #23305, #5912 ) ;
#1040 = CARTESIAN_POINT ( 'NONE',  ( 47.63716429968716426, 25.51960992152948293, 49.58068632438585865 ) ) ;
#1041 = ORIENTED_EDGE ( 'NONE', *, *, #21183, .F. ) ;
#1042 = CIRCLE ( 'NONE', #18832, 1.500000000000001332 ) ;
#1043 = CYLINDRICAL_SURFACE ( 'NONE', #25449, 1.199999999999999734 ) ;
#1044 = DIRECTION ( 'NONE',  ( 1.000000000000000000, 0.000000000000000000, 0.000000000000000000 ) ) ;
#1045 = CARTESIAN_POINT ( 'NONE',  ( -40.38481129770396194, 8.639635153120075017, 34.64781247685129273 ) ) ;
#1046 = CARTESIAN_POINT ( 'NONE',  ( 21.09785597605720042, -16.73545420775220194, 47.04930799450051637 ) ) ;
#1047 = DIRECTION ( 'NONE',  ( 0.000000000000000000, 0.000000000000000000, -1.000000000000000000 ) ) ;
#1048 = VERTEX_POINT ( 'NONE', #26098 ) ;
#1049 = CARTESIAN_POINT ( 'NONE',  ( 21.09785597605720753, 13.86454579224779948, 47.04930799450052348 ) ) ;
#1050 = CARTESIAN_POINT ( 'NONE',  ( 21.09785597605719332, -16.72540370141334520, 131.3493079945005491 ) ) ;
#1051 = DIRECTION ( 'NONE',  ( -0.000000000000000000, -1.000000000000000000, 0.000000000000000000 ) ) ;
#1052 = ORIENTED_EDGE ( 'NONE', *, *, #17154, .F. ) ;
#1053 = DIRECTION ( 'NONE',  ( 0.000000000000000000, 0.000000000000000000, 1.000000000000000000 ) ) ;
#1054 = DIRECTION ( 'NONE',  ( -1.101824276508909887E-16, 1.000000000000000000, -0.000000000000000000 ) ) ;
#1055 = TOROIDAL_SURFACE ( 'NONE', #17283, 12.40141737965287838, 0.1249999999999998335 ) ;
#1056 = LINE ( 'NONE', #3025, #19895 ) ;
#1057 = FACE_OUTER_BOUND ( 'NONE', #25387, .T. ) ;
#1058 = ORIENTED_EDGE ( 'NONE', *, *, #4110, .F. ) ;
#1059 = DIRECTION ( 'NONE',  ( -0.000000000000000000, -1.000000000000000000, -0.000000000000000000 ) ) ;
#1060 = ORIENTED_EDGE ( 'NONE', *, *, #12224, .F. ) ;
#1061 = CIRCLE ( 'NONE', #21472, 0.1250000000000001110 ) ;
#1062 = ORIENTED_EDGE ( 'NONE', *, *, #8099, .F. ) ;
#1063 = AXIS2_PLACEMENT_3D ( 'NONE', #8082, #7920, #27934 ) ;
#1064 = VECTOR ( 'NONE', #6334, 1000.000000000000000 ) ;
#1065 = VECTOR ( 'NONE', #30419, 1000.000000000000000 ) ;
#1066=STYLED_ITEM('',(#32522),#12454);
#1067 = FACE_OUTER_BOUND ( 'NONE', #17197, .T. ) ;
#1068 = DIRECTION ( 'NONE',  ( -1.000000000000000000, 0.000000000000000000, 0.000000000000000000 ) ) ;
#1069 = CARTESIAN_POINT ( 'NONE',  ( 49.98072202819531640, 26.94488759933318534, 47.19902993264913960 ) ) ;
#1070 = EDGE_CURVE ( 'NONE', #20704, #4372, #13505, .T. ) ;
#1071 = ORIENTED_EDGE ( 'NONE', *, *, #23936, .F. ) ;
#1072 = CARTESIAN_POINT ( 'NONE',  ( 48.23388202445966755, 26.82822092656774515, 49.27628909396054979 ) ) ;
#1073 = VERTEX_POINT ( 'NONE', #6245 ) ;
#1074 = EDGE_CURVE ( 'NONE', #15332, #31848, #11178, .T. ) ;
#1075 = FACE_OUTER_BOUND ( 'NONE', #20162, .T. ) ;
#1076 = DIRECTION ( 'NONE',  ( -1.101824276508909887E-16, 1.000000000000000000, -0.000000000000000000 ) ) ;
#1077 = CARTESIAN_POINT ( 'NONE',  ( -40.98031486389898248, 9.265261353013489298, 39.44930799450052206 ) ) ;
#1078 = EDGE_LOOP ( 'NONE', ( #3257, #10108, #20186, #1551 ) ) ;
#1079 = CARTESIAN_POINT ( 'NONE',  ( 49.09785597605720397, 13.86454579224779948, 47.04930799450052348 ) ) ;
#1080 = ORIENTED_EDGE ( 'NONE', *, *, #16476, .F. ) ;
#1081 = PLANE ( 'NONE',  #5494 ) ;
#1082 = CARTESIAN_POINT ( 'NONE',  ( 21.09785597605719332, 40.56454579224780588, 47.04930799450051637 ) ) ;
#1083 = EDGE_LOOP ( 'NONE', ( #28239, #21597, #8161, #3992, #26206 ) ) ;
#1084 = DIRECTION ( 'NONE',  ( -1.224646799147353207E-16, -1.349345573449484691E-32, 1.000000000000000000 ) ) ;
#1085 = AXIS2_PLACEMENT_3D ( 'NONE', #29474, #7145, #12406 ) ;
#1086 = PLANE ( 'NONE',  #19421 ) ;
#1087 = CARTESIAN_POINT ( 'NONE',  ( -41.52218637998914375, 11.15499190493234671, 37.04930799450052348 ) ) ;
#1088 = CARTESIAN_POINT ( 'NONE',  ( 47.20547626766766314, 25.38791119454915801, 44.97710074790751378 ) ) ;
#1089 = EDGE_LOOP ( 'NONE', ( #31480, #28380, #1599, #4895 ) ) ;
#1090 = VECTOR ( 'NONE', #2299, 1000.000000000000114 ) ;
#1091 = CARTESIAN_POINT ( 'NONE',  ( 47.63716429968715005, 28.89696019071909916, 49.58068632438585155 ) ) ;
#1092 = CARTESIAN_POINT ( 'NONE',  ( 21.09785597605719332, 40.06454579224778456, 47.04930799450051637 ) ) ;
#1093 = ORIENTED_EDGE ( 'NONE', *, *, #29693, .T. ) ;
#1094 = VECTOR ( 'NONE', #21735, 1000.000000000000114 ) ;
#1095 = AXIS2_PLACEMENT_3D ( 'NONE', #18592, #20746, #15506 ) ;
#1096 = DIRECTION ( 'NONE',  ( 0.000000000000000000, -1.000000000000000000, 0.000000000000000000 ) ) ;
#1097 = ORIENTED_EDGE ( 'NONE', *, *, #11165, .T. ) ;
#1098 = ORIENTED_EDGE ( 'NONE', *, *, #936, .F. ) ;
#1099 = AXIS2_PLACEMENT_3D ( 'NONE', #10139, #25067, #9972 ) ;
#1100 = ORIENTED_EDGE ( 'NONE', *, *, #7352, .F. ) ;
#1101 = AXIS2_PLACEMENT_3D ( 'NONE', #12283, #32466, #15389 ) ;
#1102 = ORIENTED_EDGE ( 'NONE', *, *, #890, .T. ) ;
#1103 = CIRCLE ( 'NONE', #12667, 2.499999999999997335 ) ;
#1104 = DIRECTION ( 'NONE',  ( -0.4848096202463424431, -0.8746197071393927436, 2.220446049250312588E-16 ) ) ;
#1105 = AXIS2_PLACEMENT_3D ( 'NONE', #19154, #12280, #17014 ) ;
#1106 = ORIENTED_EDGE ( 'NONE', *, *, #28798, .F. ) ;
#1107 = ADVANCED_FACE ( 'NONE', ( #13328 ), #31202, .T. ) ;
#1108 = EDGE_CURVE ( 'NONE', #22169, #9593, #15435, .T. ) ;
#1109 = CARTESIAN_POINT ( 'NONE',  ( 48.33536759636189828, 22.98765316579147111, 47.85212840585852234 ) ) ;
#1110 = EDGE_CURVE ( 'NONE', #4462, #25249, #21007, .T. ) ;
#1111 =( BOUNDED_CURVE ( )  B_SPLINE_CURVE ( 3, ( #18107, #6123, #11062, #15965 ),
 .UNSPECIFIED., .F., .F. ) 
 B_SPLINE_CURVE_WITH_KNOTS ( ( 4, 4 ),
 ( 1.048273564425898918, 1.570796326794896558 ),
 .UNSPECIFIED. ) 
 CURVE ( )  GEOMETRIC_REPRESENTATION_ITEM ( )  RATIONAL_B_SPLINE_CURVE ( ( 1.000000000000000000, 0.9773766218976414066, 0.9773766218976414066, 1.000000000000000000 ) ) 
 REPRESENTATION_ITEM ( '' )  );
#1112 = CARTESIAN_POINT ( 'NONE',  ( 21.09992658989239089, 25.84164230456639899, 47.04930799450051637 ) ) ;
#1113 = DIRECTION ( 'NONE',  ( -0.000000000000000000, -1.000000000000000000, -0.000000000000000000 ) ) ;
#1114 = EDGE_CURVE ( 'NONE', #116, #23509, #31166, .T. ) ;
#1115 = ADVANCED_FACE ( 'NONE', ( #11018 ), #18219, .F. ) ;
#1116 = CARTESIAN_POINT ( 'NONE',  ( 46.99218062947583974, 25.05956182964376922, 49.08406571254116102 ) ) ;
#1117 = EDGE_LOOP ( 'NONE', ( #3032, #2932, #25525, #9085 ) ) ;
#1118 = EDGE_LOOP ( 'NONE', ( #1286, #26031, #11888, #26251 ) ) ;
#1119 = DIRECTION ( 'NONE',  ( -0.8746197071393858602, 0.4848096202463547666, 0.000000000000000000 ) ) ;
#1120 = CIRCLE ( 'NONE', #24168, 15.28675991284684343 ) ;
#1121 = VERTEX_POINT ( 'NONE', #10860 ) ;
#1122 = DIRECTION ( 'NONE',  ( -0.4848096202463636484, -0.8746197071393810862, 0.000000000000000000 ) ) ;
#1123 = DIRECTION ( 'NONE',  ( -0.9612616959383205595, -0.2756373558169932236, 1.660411357259282445E-16 ) ) ;
#1124 = DIRECTION ( 'NONE',  ( 1.177206059073964094E-16, -0.2756373558165849391, 0.9612616959384376880 ) ) ;
#1125 = CARTESIAN_POINT ( 'NONE',  ( -40.54828680531407770, 6.846271790121643441, 39.54930799450052348 ) ) ;
#1126 = ORIENTED_EDGE ( 'NONE', *, *, #29812, .T. ) ;
#1127 = DIRECTION ( 'NONE',  ( -1.101824276508909887E-16, 1.000000000000000000, -0.000000000000000000 ) ) ;
#1128 = AXIS2_PLACEMENT_3D ( 'NONE', #27328, #4847, #17796 ) ;
#1129 = FACE_OUTER_BOUND ( 'NONE', #695, .T. ) ;
#1130 = CARTESIAN_POINT ( 'NONE',  ( 48.23388214087538017, 25.42822093266651606, 49.27628903457465270 ) ) ;
#1131 = CARTESIAN_POINT ( 'NONE',  ( 44.70507715278255034, 26.34951373492759430, 46.92503878583765697 ) ) ;
#1132 = AXIS2_PLACEMENT_3D ( 'NONE', #16655, #9285, #24220 ) ;
#1133 = ORIENTED_EDGE ( 'NONE', *, *, #146, .T. ) ;
#1134 = DIRECTION ( 'NONE',  ( -1.101824276508909887E-16, 1.000000000000000000, -0.000000000000000000 ) ) ;
#1135 = CIRCLE ( 'NONE', #4276, 56.47014401861810029 ) ;
#1136 = CARTESIAN_POINT ( 'NONE',  ( 33.46699938050303302, 38.56284415653841791, 47.04930799450051637 ) ) ;
#1137 = EDGE_LOOP ( 'NONE', ( #12110, #26077, #7283, #32320, #17994, #20024 ) ) ;
#1138 = EDGE_CURVE ( 'NONE', #155, #26626, #23818, .T. ) ;
#1139 = AXIS2_PLACEMENT_3D ( 'NONE', #16369, #23761, #6373 ) ;
#1140 = VERTEX_POINT ( 'NONE', #29378 ) ;
#1141 = CARTESIAN_POINT ( 'NONE',  ( -4.902144023942810236, 25.56454579224779877, 47.04930799450078638 ) ) ;
#1142 = LINE ( 'NONE', #11172, #830 ) ;
#1143 = CARTESIAN_POINT ( 'NONE',  ( 33.50134396954523908, 27.09164230456639899, 47.04930799450051637 ) ) ;
#1144 = ORIENTED_EDGE ( 'NONE', *, *, #5166, .F. ) ;
#1145 = CARTESIAN_POINT ( 'NONE',  ( -27.33830150920369206, -13.30632128221581389, 19.07865907559173380 ) ) ;
#1146 = CIRCLE ( 'NONE', #29981, 12.50000000000001776 ) ;
#1147 = CARTESIAN_POINT ( 'NONE',  ( -36.31353488181962064, 10.17485700342523458, 42.04930799450051637 ) ) ;
#1148 = CARTESIAN_POINT ( 'NONE',  ( 21.09992658989239089, 26.59143805560860940, 47.04930799450051637 ) ) ;
#1149 = EDGE_CURVE ( 'NONE', #32468, #456, #2131, .T. ) ;
#1150 = ORIENTED_EDGE ( 'NONE', *, *, #15975, .T. ) ;
#1151 = FACE_OUTER_BOUND ( 'NONE', #1860, .T. ) ;
#1152 = VERTEX_POINT ( 'NONE', #19517 ) ;
#1153 = DIRECTION ( 'NONE',  ( -1.101824276508909887E-16, 1.000000000000000000, -0.000000000000000000 ) ) ;
#1154 = DIRECTION ( 'NONE',  ( -1.000000000000000000, 0.000000000000000000, 0.000000000000000000 ) ) ;
#1155 = CARTESIAN_POINT ( 'NONE',  ( -40.66789130039685318, 6.810915939861079238, 34.59928685681251181 ) ) ;
#1156 =( NAMED_UNIT ( * ) SI_UNIT ( $, .STERADIAN. ) SOLID_ANGLE_UNIT ( ) );
#1157 = VERTEX_POINT ( 'NONE', #4269 ) ;
#1158 = VERTEX_POINT ( 'NONE', #19679 ) ;
#1159 = DIRECTION ( 'NONE',  ( -0.000000000000000000, -1.000000000000000000, 0.000000000000000000 ) ) ;
#1160 = AXIS2_PLACEMENT_3D ( 'NONE', #19272, #11903, #31929 ) ;
#1161 = FACE_OUTER_BOUND ( 'NONE', #5845, .T. ) ;
#1162 = TOROIDAL_SURFACE ( 'NONE', #11675, 12.40141737965283042, 0.1249999999999995420 ) ;
#1163 = EDGE_LOOP ( 'NONE', ( #13477, #4955, #25769, #255 ) ) ;
#1164 = LINE ( 'NONE', #18085, #25026 ) ;
#1165 = CARTESIAN_POINT ( 'NONE',  ( -40.23397449525940317, 6.794506605641760899, 39.54930799450052348 ) ) ;
#1166 = EDGE_CURVE ( 'NONE', #14445, #6352, #14609, .T. ) ;
#1167 = ORIENTED_EDGE ( 'NONE', *, *, #23303, .F. ) ;
#1168 = FACE_OUTER_BOUND ( 'NONE', #32182, .T. ) ;
#1169 = CARTESIAN_POINT ( 'NONE',  ( 49.28428300279882990, 27.64787913140504116, 48.46772541801551171 ) ) ;
#1171 = ADVANCED_FACE ( 'NONE', ( #12149 ), #27233, .F. ) ;
#1170 = CIRCLE ( 'NONE', #24754, 0.1000000000000011019 ) ;
#1172 = CARTESIAN_POINT ( 'NONE',  ( 21.09785597605720042, -14.54791319078308653, -11.41466734444011877 ) ) ;
#1173 = VECTOR ( 'NONE', #9327, 1000.000000000000000 ) ;
#1174 = EDGE_CURVE ( 'NONE', #16189, #7375, #1691, .T. ) ;
#1175 = ADVANCED_FACE ( 'NONE', ( #19187 ), #14452, .F. ) ;
#1176 = ORIENTED_EDGE ( 'NONE', *, *, #19284, .F. ) ;
#1177 = DIRECTION ( 'NONE',  ( -1.101824276508909887E-16, 1.000000000000000000, -0.000000000000000000 ) ) ;
#1178 = DIRECTION ( 'NONE',  ( 1.000000000000000000, -0.000000000000000000, -0.000000000000000000 ) ) ;
#1179 = DIRECTION ( 'NONE',  ( -1.431146867680865853E-17, -2.558717127065790464E-17, -1.000000000000000000 ) ) ;
#1180 = ORIENTED_EDGE ( 'NONE', *, *, #4567, .T. ) ;
#1181 = AXIS2_PLACEMENT_3D ( 'NONE', #4062, #6693, #31807 ) ;
#1182 = LINE ( 'NONE', #16926, #17529 ) ;
#1184 = DIRECTION ( 'NONE',  ( 0.8746197071393926326, -0.4848096202463430537, -8.676864087101709653E-18 ) ) ;
#1183 = AXIS2_PLACEMENT_3D ( 'NONE', #22137, #14606, #32166 ) ;
#1185 = ADVANCED_FACE ( 'NONE', ( #16721 ), #7215, .T. ) ;
#1186 = DIRECTION ( 'NONE',  ( -1.000000000000000000, 0.000000000000000000, 0.000000000000000000 ) ) ;
#1187 = VERTEX_POINT ( 'NONE', #1804 ) ;
#1188 = DIRECTION ( 'NONE',  ( 0.8746197071393926326, -0.4848096202463430537, -8.676864087101709653E-18 ) ) ;
#1189 = DIRECTION ( 'NONE',  ( 0.1949050434465272041, -0.6797146636928682595, 0.7071067811865464625 ) ) ;
#1190 = CARTESIAN_POINT ( 'NONE',  ( 21.09992658989238734, 31.34184655352422766, 47.04930799450051637 ) ) ;
#1191 = EDGE_LOOP ( 'NONE', ( #20839, #14385, #18300, #16135 ) ) ;
#1192 = CARTESIAN_POINT ( 'NONE',  ( 60.59785597605720397, 14.86454579224779948, 47.04930799450051637 ) ) ;
#1193 = CARTESIAN_POINT ( 'NONE',  ( 48.40186567930497574, 26.72957786121581947, 45.03923535223907493 ) ) ;
#1194 = DIRECTION ( 'NONE',  ( 0.000000000000000000, 1.000000000000000000, 0.000000000000000000 ) ) ;
#1195 = CARTESIAN_POINT ( 'NONE',  ( -40.11708823821336267, 6.803395581744677401, 34.64878293746919979 ) ) ;
#1196 = MANIFOLD_SOLID_BREP ( 'Stock-MAT-060-1', #11089 ) ;
#1197 = DIRECTION ( 'NONE',  ( 0.4544104193609900810, 0.000000000000000000, 0.8907924397839089847 ) ) ;
#1198 = ORIENTED_EDGE ( 'NONE', *, *, #25045, .T. ) ;
#1199 = DIRECTION ( 'NONE',  ( 0.000000000000000000, -0.000000000000000000, -1.000000000000000000 ) ) ;
#1200 = CARTESIAN_POINT ( 'NONE',  ( 47.09785597605719687, 23.12036939723557083, 47.04930799450080059 ) ) ;
#1201 = CARTESIAN_POINT ( 'NONE',  ( -40.13606231985500017, 7.635531802539802904, 53.64930799450051779 ) ) ;
#1202 = EDGE_CURVE ( 'NONE', #5096, #18712, #24777, .T. ) ;
#1203 = EDGE_LOOP ( 'NONE', ( #5817, #15284, #10647, #19677 ) ) ;
#1204 = CARTESIAN_POINT ( 'NONE',  ( -40.02540636251513462, 2.839176264122873050, 37.04930799450052348 ) ) ;
#1205 = DIRECTION ( 'NONE',  ( 1.000000000000000000, 0.000000000000000000, 0.000000000000000000 ) ) ;
#1206 = LINE ( 'NONE', #30777, #8886 ) ;
#1207 = EDGE_CURVE ( 'NONE', #14676, #24757, #29053, .T. ) ;
#1208 = CARTESIAN_POINT ( 'NONE',  ( 53.51600554467332671, -5.395280703882722406, -10.73892745771225599 ) ) ;
#1209 = TOROIDAL_SURFACE ( 'NONE', #13804, 12.61792373059897621, 0.1249999999999970163 ) ;
#1210 = ORIENTED_EDGE ( 'NONE', *, *, #8305, .T. ) ;
#1211 = DIRECTION ( 'NONE',  ( 1.000000000000000000, 0.000000000000000000, 0.000000000000000000 ) ) ;
#1212 = ORIENTED_EDGE ( 'NONE', *, *, #28402, .T. ) ;
#1213 = TOROIDAL_SURFACE ( 'NONE', #10659, 0.2000000000000000111, 0.1000000000000000056 ) ;
#1214 = EDGE_CURVE ( 'NONE', #30342, #31925, #15331, .T. ) ;
#1215 = VERTEX_POINT ( 'NONE', #17056 ) ;
#1216 = EDGE_CURVE ( 'NONE', #21033, #23633, #1170, .T. ) ;
#1217 = VECTOR ( 'NONE', #18449, 1000.000000000000000 ) ;
#1218 = CONICAL_SURFACE ( 'NONE', #30581, 13.20165371409683708, 1.570144820418440945 ) ;
#1219 = CARTESIAN_POINT ( 'NONE',  ( 21.09785597605719332, 17.16451738380053271, 47.04930799450051637 ) ) ;
#1220 = CARTESIAN_POINT ( 'NONE',  ( -33.86637752982123573, -3.544489376609568421, 80.67335282074090230 ) ) ;
#1221 = DIRECTION ( 'NONE',  ( -1.101824276508909887E-16, 1.000000000000000000, -0.000000000000000000 ) ) ;
#1222 = EDGE_LOOP ( 'NONE', ( #3505, #5373, #3575, #27729 ) ) ;
#1223 = CARTESIAN_POINT ( 'NONE',  ( -34.46767470602752326, 11.80860034638430989, 40.73713547295701431 ) ) ;
#1224 = VERTEX_POINT ( 'NONE', #15093 ) ;
#1225 = CIRCLE ( 'NONE', #32177, 46.53489018157424084 ) ;
#1226 = CARTESIAN_POINT ( 'NONE',  ( 21.09785597605719332, 30.36454579224779238, 47.04930799450051637 ) ) ;
#1227 = FACE_OUTER_BOUND ( 'NONE', #10320, .T. ) ;
#1228 = DIRECTION ( 'NONE',  ( -1.000000000000000000, 0.000000000000000000, 0.000000000000000000 ) ) ;
#1229 = VERTEX_POINT ( 'NONE', #17703 ) ;
#1230 = CARTESIAN_POINT ( 'NONE',  ( 21.09785597605719332, -15.93545420775219945, 47.04930799450051637 ) ) ;
#1231 = CARTESIAN_POINT ( 'NONE',  ( 61.09785597605721108, -5.098646251524523443, 47.04930799450051637 ) ) ;
#1232 = DIRECTION ( 'NONE',  ( 1.000000000000000000, 0.000000000000000000, 0.000000000000000000 ) ) ;
#1233 = DIRECTION ( 'NONE',  ( -1.000000000000000000, 0.000000000000000000, 0.000000000000000000 ) ) ;
#1234 = ORIENTED_EDGE ( 'NONE', *, *, #29026, .F. ) ;
#1235 = DIRECTION ( 'NONE',  ( 0.000000000000000000, 0.000000000000000000, 1.000000000000000000 ) ) ;
#1236 = DIRECTION ( 'NONE',  ( 0.7141240004913222972, -0.3958453973320028019, -0.5773502691896303940 ) ) ;
#1237 = DIRECTION ( 'NONE',  ( 0.7936353835927094647, -0.4399192766786362285, -0.4202545751282172337 ) ) ;
#1238 = DIRECTION ( 'NONE',  ( -0.9097384655268496711, -0.4151817967359032746, -2.820562191637069417E-18 ) ) ;
#1239 = AXIS2_PLACEMENT_3D ( 'NONE', #3672, #18277, #16138 ) ;
#1240 = DIRECTION ( 'NONE',  ( -0.4544104193609990738, 0.000000000000000000, -0.8907924397839043218 ) ) ;
#1241 = AXIS2_PLACEMENT_3D ( 'NONE', #4451, #6592, #13985 ) ;
#1242 = ORIENTED_EDGE ( 'NONE', *, *, #28098, .T. ) ;
#1243 = CARTESIAN_POINT ( 'NONE',  ( 21.09785597605720753, -16.03545420775219910, 111.5493079945005235 ) ) ;
#1244 = CARTESIAN_POINT ( 'NONE',  ( -40.57119026524449623, 6.941393190192507667, 34.94194090914223949 ) ) ;
#1245 = EDGE_CURVE ( 'NONE', #18233, #24509, #5247, .T. ) ;
#1246 = ORIENTED_EDGE ( 'NONE', *, *, #10469, .T. ) ;
#1247 = DIRECTION ( 'NONE',  ( -1.101824276508909887E-16, 1.000000000000000000, -0.000000000000000000 ) ) ;
#1248 = CARTESIAN_POINT ( 'NONE',  ( -10.01616728275229740, -5.935340315990530691, -13.32263710021335612 ) ) ;
#1249 = ORIENTED_EDGE ( 'NONE', *, *, #26072, .T. ) ;
#1250 = ORIENTED_EDGE ( 'NONE', *, *, #9597, .F. ) ;
#1251 = UNCERTAINTY_MEASURE_WITH_UNIT (LENGTH_MEASURE( 1.000000000000000082E-05 ), #14331, 'distance_accuracy_value', 'NONE');
#1252 = B_SPLINE_CURVE_WITH_KNOTS ( 'NONE', 3,
 ( #26867, #9304, #29325, #14400, #1911, #29502 ),
 .UNSPECIFIED., .F., .F.,
 ( 4, 2, 4 ),
 ( 0.000000000000000000, 0.5000000000000000000, 1.000000000000000000 ),
 .UNSPECIFIED. ) ;
#1253 = ADVANCED_FACE ( 'NONE', ( #12805 ), #10093, .T. ) ;
#1254 = ORIENTED_EDGE ( 'NONE', *, *, #21788, .F. ) ;
#1255 = AXIS2_PLACEMENT_3D ( 'NONE', #6118, #23513, #31074 ) ;
#1256 = ORIENTED_EDGE ( 'NONE', *, *, #4300, .T. ) ;
#1257 = DIRECTION ( 'NONE',  ( 0.9612616959383206705, 0.2756373558169926130, 8.795445018804289444E-19 ) ) ;
#1258 = ORIENTED_EDGE ( 'NONE', *, *, #11197, .F. ) ;
#1259 = CARTESIAN_POINT ( 'NONE',  ( 48.43832450663380484, 22.91413368675619111, 48.25518855289821119 ) ) ;
#1260 = CARTESIAN_POINT ( 'NONE',  ( -40.68422973805265030, 6.807290781432339344, 39.32248954417796227 ) ) ;
#1261 = CARTESIAN_POINT ( 'NONE',  ( -40.50737503712689147, 7.561449354142130375, 53.83005649861389941 ) ) ;
#1262 = PRODUCT_RELATED_PRODUCT_CATEGORY ( 'part', '', ( #20053 ) ) ;
#1263 = CARTESIAN_POINT ( 'NONE',  ( 47.20353132263855400, 28.95286309983297812, 45.01455027646041174 ) ) ;
#1264 = EDGE_LOOP ( 'NONE', ( #23405, #5716, #4879, #844 ) ) ;
#1265 = VERTEX_POINT ( 'NONE', #20497 ) ;
#1266 = DIRECTION ( 'NONE',  ( -1.224646799147353207E-16, -1.349345573449484691E-32, 1.000000000000000000 ) ) ;
#1267 = ORIENTED_EDGE ( 'NONE', *, *, #2115, .T. ) ;
#1268 = DIRECTION ( 'NONE',  ( 1.234978253042719660E-16, -1.000000000000000000, -1.109335647967047851E-31 ) ) ;
#1269 = CARTESIAN_POINT ( 'NONE',  ( 21.09992658989239089, 24.96183152705960140, 47.04930799450051637 ) ) ;
#1270 = CARTESIAN_POINT ( 'NONE',  ( -40.69571722278731585, 6.786566810383049209, 39.44930799450052206 ) ) ;
#1271 = AXIS2_PLACEMENT_3D ( 'NONE', #17739, #12013, #20208 ) ;
#1272 = AXIS2_PLACEMENT_3D ( 'NONE', #3616, #28729, #21163 ) ;
#1273 = CARTESIAN_POINT ( 'NONE',  ( 0.6836613156275053171, 11.92558985988973497, -5.803495753465989893 ) ) ;
#1274 = DIRECTION ( 'NONE',  ( -1.000000000000000000, 0.000000000000000000, 0.000000000000000000 ) ) ;
#1275 = CIRCLE ( 'NONE', #11247, 46.03812797983318461 ) ;
#1276 = ITEM_DEFINED_TRANSFORMATION ( 'NONE', 'NONE', #13954,  #8172 ) ;
#1277 = ORIENTED_EDGE ( 'NONE', *, *, #711, .T. ) ;
#1278 = FACE_OUTER_BOUND ( 'NONE', #27742, .T. ) ;
#1279 = DIRECTION ( 'NONE',  ( 2.779292025043186357E-18, -1.288349127009862211E-17, 1.000000000000000000 ) ) ;
#1280 = CIRCLE ( 'NONE', #5493, 0.1250000000000001110 ) ;
#1281 = CARTESIAN_POINT ( 'NONE',  ( 21.09785597605720753, 14.86454579224779948, 47.04930799450052348 ) ) ;
#1282 = AXIS2_PLACEMENT_3D ( 'NONE', #25712, #30968, #2899 ) ;
#1283 = AXIS2_PLACEMENT_3D ( 'NONE', #2957, #27434, #10201 ) ;
#1284 = DIRECTION ( 'NONE',  ( -1.101824276508909887E-16, 1.000000000000000000, -0.000000000000000000 ) ) ;
#1285 = FACE_OUTER_BOUND ( 'NONE', #3726, .T. ) ;
#1286 = ORIENTED_EDGE ( 'NONE', *, *, #27316, .F. ) ;
#1287 = DIRECTION ( 'NONE',  ( -1.000000000000000000, 0.000000000000000000, 0.000000000000000000 ) ) ;
#1288 = EDGE_LOOP ( 'NONE', ( #27758, #29000, #14380, #13174 ) ) ;
#1289 = AXIS2_PLACEMENT_3D ( 'NONE', #1498, #12009, #32033 ) ;
#1290 = LINE ( 'NONE', #23943, #31888 ) ;
#1291 = EDGE_CURVE ( 'NONE', #10579, #24958, #20556, .T. ) ;
#1292 = EDGE_LOOP ( 'NONE', ( #17485, #2942, #9544, #30462 ) ) ;
#1293 = EDGE_CURVE ( 'NONE', #25363, #13517, #18029, .T. ) ;
#1294 = EDGE_CURVE ( 'NONE', #19345, #18749, #642, .T. ) ;
#1295 = EDGE_CURVE ( 'NONE', #19780, #23334, #28946, .T. ) ;
#1296 = EDGE_CURVE ( 'NONE', #19168, #20299, #21078, .T. ) ;
#1297 = TOROIDAL_SURFACE ( 'NONE', #778, 12.40141737965288904, 0.1249999999999998612 ) ;
#1298 =( BOUNDED_CURVE ( )  B_SPLINE_CURVE ( 3, ( #6678, #1749, #21433, #31949 ),
 .UNSPECIFIED., .F., .F. ) 
 B_SPLINE_CURVE_WITH_KNOTS ( ( 4, 4 ),
 ( 2.001968580199905201, 2.533845118315130041 ),
 .UNSPECIFIED. ) 
 CURVE ( )  GEOMETRIC_REPRESENTATION_ITEM ( )  RATIONAL_B_SPLINE_CURVE ( ( 1.000000000000000000, 0.9765642231641245008, 0.9765642231641245008, 1.000000000000000000 ) ) 
 REPRESENTATION_ITEM ( '' )  );
#1299 = EDGE_LOOP ( 'NONE', ( #8915, #25452, #7300, #565, #2321, #17317 ) ) ;
#1300 = AXIS2_PLACEMENT_3D ( 'NONE', #24449, #4434, #31842 ) ;
#1301 = CARTESIAN_POINT ( 'NONE',  ( 49.32483701613094240, 25.72587066347689699, 45.91328182968236860 ) ) ;
#1302 = CARTESIAN_POINT ( 'NONE',  ( -42.22138300640814634, 14.68176690255379491, 37.04930799450052348 ) ) ;
#1304 = DIRECTION ( 'NONE',  ( -1.224646799147353207E-16, -1.349345573449484691E-32, 1.000000000000000000 ) ) ;
#1303 = AXIS2_PLACEMENT_3D ( 'NONE', #29470, #27000, #4513 ) ;
#1305 = AXIS2_PLACEMENT_3D ( 'NONE', #9730, #19722, #27116 ) ;
#1306 = VECTOR ( 'NONE', #4417, 1000.000000000000000 ) ;
#1307 = ORIENTED_EDGE ( 'NONE', *, *, #13757, .F. ) ;
#1308 = DIRECTION ( 'NONE',  ( -0.9612616959383200044, -0.2756373558169954996, 1.660411357259285896E-16 ) ) ;
#1309 = CARTESIAN_POINT ( 'NONE',  ( -35.14417515838577089, 11.92558985988973674, 40.19270369045111124 ) ) ;
#1310 = CARTESIAN_POINT ( 'NONE',  ( -40.01185171578376298, 7.339011093366010208, 38.76026362135365844 ) ) ;
#1311 = VERTEX_POINT ( 'NONE', #2458 ) ;
#1312 = DIRECTION ( 'NONE',  ( 0.8746197071393928546, -0.4848096202463424431, -1.277302113040829905E-17 ) ) ;
#1313 = EDGE_LOOP ( 'NONE', ( #3808, #4252, #18593, #32168 ) ) ;
#1314 = CYLINDRICAL_SURFACE ( 'NONE', #9732, 12.36707279061065279 ) ;
#1315 = CYLINDRICAL_SURFACE ( 'NONE', #22680, 0.1000000000000012962 ) ;
#1316 = DIRECTION ( 'NONE',  ( 0.4848096202463429982, 0.8746197071393925215, 9.920727850371698576E-18 ) ) ;
#1317 = PRESENTATION_STYLE_ASSIGNMENT (( #30729 ) ) ;
#1318 = ORIENTED_EDGE ( 'NONE', *, *, #9258, .F. ) ;
#1319 = VERTEX_POINT ( 'NONE', #12964 ) ;
#1320 = EDGE_CURVE ( 'NONE', #31644, #4648, #25806, .T. ) ;
#1321 = DIRECTION ( 'NONE',  ( -0.000000000000000000, -1.000000000000000000, 0.000000000000000000 ) ) ;
#1322 = DIRECTION ( 'NONE',  ( -0.000000000000000000, -1.000000000000000000, -0.000000000000000000 ) ) ;
#1323 = FACE_OUTER_BOUND ( 'NONE', #17617, .T. ) ;
#1324 = AXIS2_PLACEMENT_3D ( 'NONE', #22136, #32165, #7208 ) ;
#1325 = ORIENTED_EDGE ( 'NONE', *, *, #1420, .F. ) ;
#1326 = DIRECTION ( 'NONE',  ( 0.8746197071393925215, -0.4848096202463429982, -8.676864087101708112E-18 ) ) ;
#1327 = CARTESIAN_POINT ( 'NONE',  ( 39.85850837550805892, -13.74047052604243113, -8.200871005067009278 ) ) ;
#1328 = VERTEX_POINT ( 'NONE', #10013 ) ;
#1330 = TOROIDAL_SURFACE ( 'NONE', #4473, 12.40141737965281621, 0.1250000000000009159 ) ;
#1329 = CARTESIAN_POINT ( 'NONE',  ( -40.50735885958352611, 7.561537692508191633, 60.26824376325151889 ) ) ;
#1331 = CARTESIAN_POINT ( 'NONE',  ( 44.91142894931555674, 27.99787913140503903, 45.63089057098605394 ) ) ;
#1332 = AXIS2_PLACEMENT_3D ( 'NONE', #5299, #12197, #17433 ) ;
#1333 = COLOUR_RGB ( '',0.7921568627450980005, 0.8196078431372548767, 0.9333333333333333481 ) ;
#1334 = FACE_OUTER_BOUND ( 'NONE', #579, .T. ) ;
#1335 = AXIS2_PLACEMENT_3D ( 'NONE', #21891, #19595, #19435 ) ;
#1336 = EDGE_CURVE ( 'NONE', #25136, #28530, #5568, .T. ) ;
#1337 = ADVANCED_FACE ( 'NONE', ( #7876 ), #23185, .T. ) ;
#1338 = EDGE_CURVE ( 'NONE', #15696, #1073, #15847, .T. ) ;
#1339 = AXIS2_PLACEMENT_3D ( 'NONE', #28718, #16558, #6237 ) ;
#1340 = VERTEX_POINT ( 'NONE', #27894 ) ;
#1341 = DIRECTION ( 'NONE',  ( -1.000000000000000000, 0.000000000000000000, 0.000000000000000000 ) ) ;
#1342 = CARTESIAN_POINT ( 'NONE',  ( 21.09785597605719332, 30.56454579224779522, 15.74930799450053520 ) ) ;
#1343 = DIRECTION ( 'NONE',  ( 1.000000000000000000, 0.000000000000000000, 0.000000000000000000 ) ) ;
#1344 = CARTESIAN_POINT ( 'NONE',  ( 46.00908685603034343, 29.73284706826092361, 44.91496614357595263 ) ) ;
#1345 = EDGE_LOOP ( 'NONE', ( #24023, #10334, #14732, #11651 ) ) ;
#1346 = DIRECTION ( 'NONE',  ( 0.9612616959383194493, 0.2756373558169974980, 8.795445018804946186E-19 ) ) ;
#1347 = DIRECTION ( 'NONE',  ( -1.000000000000000000, -1.101824276508910010E-16, 0.000000000000000000 ) ) ;
#1348 = CIRCLE ( 'NONE', #5561, 12.36707279061065101 ) ;
#1349 = FACE_BOUND ( 'NONE', #4250, .T. ) ;
#1350 = DIRECTION ( 'NONE',  ( 0.8746197071393926326, -0.4848096202463430537, -8.676864087101709653E-18 ) ) ;
#1351 = DIRECTION ( 'NONE',  ( 0.7141240004913222972, -0.3958453973320028019, -0.5773502691896303940 ) ) ;
#1352 = DIRECTION ( 'NONE',  ( -0.2756373558169932236, 0.9612616959383204485, -1.479773560108267395E-16 ) ) ;
#1353 = CARTESIAN_POINT ( 'NONE',  ( 45.52675994804781112, 25.43420399681022914, 49.47108226228596806 ) ) ;
#1354 = DIRECTION ( 'NONE',  ( 0.000000000000000000, 0.000000000000000000, 1.000000000000000000 ) ) ;
#1355 = ORIENTED_EDGE ( 'NONE', *, *, #7152, .T. ) ;
#1356 = ADVANCED_FACE ( 'NONE', ( #15568 ), #5410, .T. ) ;
#1357 = CARTESIAN_POINT ( 'NONE',  ( -39.59792565122570096, 7.943629834091022524, 39.54930799450052348 ) ) ;
#1358 = CARTESIAN_POINT ( 'NONE',  ( 45.24946171279598417, 28.42124452788248234, 47.99220971130007030 ) ) ;
#1359 = EDGE_CURVE ( 'NONE', #12063, #12175, #10176, .T. ) ;
#1360 = DIRECTION ( 'NONE',  ( -1.000000000000000000, -1.101824276508909887E-16, 0.000000000000000000 ) ) ;
#1361 = DIRECTION ( 'NONE',  ( -1.000000000000000000, 0.000000000000000000, 0.000000000000000000 ) ) ;
#1362 = VECTOR ( 'NONE', #6802, 1000.000000000000114 ) ;
#1363 = CARTESIAN_POINT ( 'NONE',  ( 21.09785597605720753, 15.11603238453479037, 47.04930799450052348 ) ) ;
#1364 = ORIENTED_EDGE ( 'NONE', *, *, #21443, .T. ) ;
#1365 = CARTESIAN_POINT ( 'NONE',  ( -41.40774006177731081, 10.72547736613775626, 57.28220823191252720 ) ) ;
#1366 = DIRECTION ( 'NONE',  ( -1.000000000000000000, -0.000000000000000000, -3.491481338843133355E-15 ) ) ;
#1367 = CARTESIAN_POINT ( 'NONE',  ( 21.09785597605719332, -19.93545420775220123, 47.04930799450051637 ) ) ;
#1368 = ORIENTED_EDGE ( 'NONE', *, *, #22630, .F. ) ;
#1369 = CARTESIAN_POINT ( 'NONE',  ( 8.474859994195282908, 38.56284415653841791, 47.04930799450051637 ) ) ;
#1370 = DIRECTION ( 'NONE',  ( -0.000000000000000000, -0.000000000000000000, -1.000000000000000000 ) ) ;
#1371 = CARTESIAN_POINT ( 'NONE',  ( -40.47970302497625994, 7.463434137431150361, 53.64930799450051779 ) ) ;
#1372 = CARTESIAN_POINT ( 'NONE',  ( 51.66808379569695830, 5.388785998227650254, 106.7232700815558957 ) ) ;
#1373 = ORIENTED_EDGE ( 'NONE', *, *, #20000, .F. ) ;
#1374 = DIRECTION ( 'NONE',  ( 0.000000000000000000, 0.000000000000000000, -1.000000000000000000 ) ) ;
#1375 = VERTEX_POINT ( 'NONE', #25582 ) ;
#1376 = ADVANCED_FACE ( 'NONE', ( #20171 ), #28437, .T. ) ;
#1377 = CIRCLE ( 'NONE', #13975, 33.50000000000000000 ) ;
#1378 = ORIENTED_EDGE ( 'NONE', *, *, #31391, .F. ) ;
#1379 = ORIENTED_EDGE ( 'NONE', *, *, #26631, .F. ) ;
#1380 = CIRCLE ( 'NONE', #19729, 54.10000000000000142 ) ;
#1381 = ADVANCED_FACE ( 'NONE', ( #30196 ), #7984, .T. ) ;
#1382 = CARTESIAN_POINT ( 'NONE',  ( -40.75848109938849717, 9.580021662090986823, 38.54930799450052348 ) ) ;
#1383 = DIRECTION ( 'NONE',  ( -1.101824276508909887E-16, 1.000000000000000000, -0.000000000000000000 ) ) ;
#1384 = DIRECTION ( 'NONE',  ( -1.000000000000000000, 0.000000000000000000, 0.000000000000000000 ) ) ;
#1385 = EDGE_CURVE ( 'NONE', #10661, #15368, #9022, .T. ) ;
#1386 = ORIENTED_EDGE ( 'NONE', *, *, #2719, .F. ) ;
#1387 = DIRECTION ( 'NONE',  ( -1.000000000000000000, 0.000000000000000000, 0.000000000000000000 ) ) ;
#1388 = ORIENTED_EDGE ( 'NONE', *, *, #25283, .F. ) ;
#1389 = CARTESIAN_POINT ( 'NONE',  ( 21.09785597605719332, 30.56454579224779522, 33.84930799450050642 ) ) ;
#1390 = CARTESIAN_POINT ( 'NONE',  ( -40.50726676055796105, 7.559560307024983494, 60.29072935073781991 ) ) ;
#1391 = LINE ( 'NONE', #21247, #8965 ) ;
#1392 = VERTEX_POINT ( 'NONE', #20817 ) ;
#1393 = EDGE_CURVE ( 'NONE', #7595, #2858, #1686, .T. ) ;
#1394 = SPHERICAL_SURFACE ( 'NONE', #7627, 0.1000000000000000056 ) ;
#1395 = DIRECTION ( 'NONE',  ( -1.101824276508909887E-16, 1.000000000000000000, -0.000000000000000000 ) ) ;
#1396 = DIRECTION ( 'NONE',  ( 0.000000000000000000, 0.000000000000000000, 1.000000000000000000 ) ) ;
#1398 = CARTESIAN_POINT ( 'NONE',  ( 45.46177120706448704, 22.89977464660286444, 46.15605224449101485 ) ) ;
#1397 = AXIS2_PLACEMENT_3D ( 'NONE', #3502, #11227, #21372 ) ;
#1399 = EDGE_CURVE ( 'NONE', #18054, #15162, #3087, .T. ) ;
#1400 = VERTEX_POINT ( 'NONE', #11298 ) ;
#1401 = CARTESIAN_POINT ( 'NONE',  ( 47.03932003404746354, 22.95310733321322161, 45.41014739348889862 ) ) ;
#1402 = DIRECTION ( 'NONE',  ( -0.8746197071393810862, 0.4848096202463637039, 8.676864087101942305E-18 ) ) ;
#1403 = CARTESIAN_POINT ( 'NONE',  ( 59.59785597605720397, 13.86454579224779948, 47.04930799450051637 ) ) ;
#1404 = DIRECTION ( 'NONE',  ( -0.9612616959383207815, -0.2756373558169927795, 2.080984688351791594E-17 ) ) ;
#1405 = EDGE_CURVE ( 'NONE', #14676, #10661, #3261, .T. ) ;
#1406 = DIRECTION ( 'NONE',  ( 0.000000000000000000, -0.000000000000000000, -1.000000000000000000 ) ) ;
#1407 = ORIENTED_EDGE ( 'NONE', *, *, #7950, .F. ) ;
#1408 = DIRECTION ( 'NONE',  ( -0.000000000000000000, 1.000000000000000000, -0.000000000000000000 ) ) ;
#1409 = DIRECTION ( 'NONE',  ( 0.000000000000000000, 0.000000000000000000, -1.000000000000000000 ) ) ;
#1410 = ORIENTED_EDGE ( 'NONE', *, *, #5755, .F. ) ;
#1411 = LINE ( 'NONE', #23580, #3582 ) ;
#1412 = AXIS2_PLACEMENT_3D ( 'NONE', #13319, #28407, #7736 ) ;
#1413 = FACE_OUTER_BOUND ( 'NONE', #29852, .T. ) ;
#1414 = ORIENTED_EDGE ( 'NONE', *, *, #955, .T. ) ;
#1415 = ORIENTED_EDGE ( 'NONE', *, *, #9403, .T. ) ;
#1416 = EDGE_CURVE ( 'NONE', #25267, #14096, #7468, .T. ) ;
#1417 = EDGE_LOOP ( 'NONE', ( #27072, #20083, #10401, #7399 ) ) ;
#1418 = AXIS2_PLACEMENT_3D ( 'NONE', #22607, #24582, #5059 ) ;
#1419 = AXIS2_PLACEMENT_3D ( 'NONE', #21368, #5980, #13693 ) ;
#1420 = EDGE_CURVE ( 'NONE', #20658, #19118, #20031, .T. ) ;
#1421 = DIRECTION ( 'NONE',  ( -1.000000000000000000, 0.000000000000000000, 0.000000000000000000 ) ) ;
#1422 = EDGE_CURVE ( 'NONE', #90, #22267, #8822, .T. ) ;
#1423 = ORIENTED_EDGE ( 'NONE', *, *, #26261, .F. ) ;
#1424 = CARTESIAN_POINT ( 'NONE',  ( 47.09785597605719687, 24.86874180309281712, 47.04930799450078638 ) ) ;
#1425 = DIRECTION ( 'NONE',  ( 0.4848096202463673676, 0.8746197071393789768, 0.000000000000000000 ) ) ;
#1426 = CYLINDRICAL_SURFACE ( 'NONE', #18100, 34.00000000000000000 ) ;
#1427 = CARTESIAN_POINT ( 'NONE',  ( 21.09785597605720042, -13.37218737171702543, 47.04930799450051637 ) ) ;
#1428 = CARTESIAN_POINT ( 'NONE',  ( 47.20353132263855400, 28.25286309983298239, 45.01455027646040463 ) ) ;
#1429 = ORIENTED_EDGE ( 'NONE', *, *, #23635, .F. ) ;
#1430 = ORIENTED_EDGE ( 'NONE', *, *, #12094, .F. ) ;
#1431 = CARTESIAN_POINT ( 'NONE',  ( -10.77327584252841675, 2.854128177266956445, -4.829733788720330878 ) ) ;
#1432 = ADVANCED_FACE ( 'NONE', ( #21127 ), #14282, .T. ) ;
#1433 = ORIENTED_EDGE ( 'NONE', *, *, #18374, .T. ) ;
#1434 = CARTESIAN_POINT ( 'NONE',  ( -33.20214402394279318, 14.66454579224779842, 47.04930799450052348 ) ) ;
#1435 = CARTESIAN_POINT ( 'NONE',  ( -40.63900869798943205, 6.896661531574880044, 39.10715606024436397 ) ) ;
#1436 = CARTESIAN_POINT ( 'NONE',  ( -42.47434154250544225, 4.196643200812637531, 57.04930799450051637 ) ) ;
#1437 = CARTESIAN_POINT ( 'NONE',  ( 21.09785597605720753, 14.86454579224779948, 47.04930799450052348 ) ) ;
#1438 = ADVANCED_FACE ( 'NONE', ( #28215 ), #22118, .T. ) ;
#1439 = CARTESIAN_POINT ( 'NONE',  ( 49.41945501136223839, 25.66454579807171399, 45.86501535757901848 ) ) ;
#1440 = CARTESIAN_POINT ( 'NONE',  ( 47.05971367727331511, 23.09557481883486574, 47.78372960763746136 ) ) ;
#1441 = ORIENTED_EDGE ( 'NONE', *, *, #179, .F. ) ;
#1442 = DIRECTION ( 'NONE',  ( 0.000000000000000000, 0.000000000000000000, 1.000000000000000000 ) ) ;
#1443 = ADVANCED_FACE ( 'NONE', ( #6369 ), #23288, .T. ) ;
#1444 = AXIS2_PLACEMENT_3D ( 'NONE', #20383, #7445, #27619 ) ;
#1445 = DIRECTION ( 'NONE',  ( 1.234978253042719660E-16, -1.000000000000000000, -1.109335647967047851E-31 ) ) ;
#1446 = CIRCLE ( 'NONE', #24577, 0.1000000000000018235 ) ;
#1447 = CARTESIAN_POINT ( 'NONE',  ( -40.41647043964083252, 8.356895951721261540, 54.64930799450051069 ) ) ;
#1448 = DIRECTION ( 'NONE',  ( -1.101824276508909887E-16, 1.000000000000000000, -0.000000000000000000 ) ) ;
#1449 = EDGE_LOOP ( 'NONE', ( #4769, #28960 ) ) ;
#1450 = DIRECTION ( 'NONE',  ( 0.000000000000000000, 0.000000000000000000, -1.000000000000000000 ) ) ;
#1451 = TOROIDAL_SURFACE ( 'NONE', #31866, 12.40141737965288904, 0.1249999999999998612 ) ;
#1452 = ORIENTED_EDGE ( 'NONE', *, *, #25684, .F. ) ;
#1453 = DIRECTION ( 'NONE',  ( 0.2756373558169932236, -0.9612616959383205595, -1.211836997745615998E-14 ) ) ;
#1454 = B_SPLINE_CURVE_WITH_KNOTS ( 'NONE', 3,
 ( #14906, #12614, #22766, #24749, #284, #20140, #30497, #30172 ),
 .UNSPECIFIED., .F., .F.,
 ( 4, 2, 2, 4 ),
 ( 4.148501517905142282E-16, 0.0002713365654423687142, 0.0005426731308843225042, 0.001085346261768216532 ),
 .UNSPECIFIED. ) ;
#1455 = DIRECTION ( 'NONE',  ( 0.000000000000000000, 1.000000000000000000, -0.000000000000000000 ) ) ;
#1456 = CIRCLE ( 'NONE', #7745, 59.44168675549763492 ) ;
#1457 = ORIENTED_EDGE ( 'NONE', *, *, #28527, .F. ) ;
#1458 = ORIENTED_EDGE ( 'NONE', *, *, #25398, .T. ) ;
#1459 = CARTESIAN_POINT ( 'NONE',  ( 33.72499318558949710, 31.59184655352418503, 47.04930799450051637 ) ) ;
#1460 = TOROIDAL_SURFACE ( 'NONE', #937, 1.299999999999999822, 0.1000000000000000056 ) ;
#1461 = DIRECTION ( 'NONE',  ( 0.9612616959383198934, 0.2756373558169956106, 0.000000000000000000 ) ) ;
#1462 = DIRECTION ( 'NONE',  ( 0.000000000000000000, 0.000000000000000000, -1.000000000000000000 ) ) ;
#1463 = EDGE_LOOP ( 'NONE', ( #32458, #3921, #4900, #4428 ) ) ;
#1464 = MANIFOLD_SOLID_BREP ( 'Stock-MAT-060-1', #18928 ) ;
#1465 = TOROIDAL_SURFACE ( 'NONE', #8296, 12.61792373059898331, 0.1249999999999965583 ) ;
#1466 = FACE_OUTER_BOUND ( 'NONE', #15993, .T. ) ;
#1467 = VECTOR ( 'NONE', #28994, 1000.000000000000227 ) ;
#1468 = CARTESIAN_POINT ( 'NONE',  ( -43.64073206722599707, 1.267352857069778960, 34.64930799450052490 ) ) ;
#1469 = CARTESIAN_POINT ( 'NONE',  ( 76.12931116418575073, -2.304636120132655286, 13.31869760836049466 ) ) ;
#1470 = ORIENTED_EDGE ( 'NONE', *, *, #18966, .F. ) ;
#1471 = CARTESIAN_POINT ( 'NONE',  ( 21.09992658989239089, 29.47145308207317882, 47.04930799450051637 ) ) ;
#1472 = ADVANCED_FACE ( 'NONE', ( #3419 ), #26855, .T. ) ;
#1473 = ORIENTED_EDGE ( 'NONE', *, *, #4176, .T. ) ;
#1474 = AXIS2_PLACEMENT_3D ( 'NONE', #17583, #30074, #30231 ) ;
#1475 = CARTESIAN_POINT ( 'NONE',  ( -37.49824857498671093, 12.70128680827697387, 57.95249952744806166 ) ) ;
#1476 = CARTESIAN_POINT ( 'NONE',  ( 48.83059987400640978, 29.08213139976340500, 48.97189179988551899 ) ) ;
#1477 = CARTESIAN_POINT ( 'NONE',  ( 8.474859994195286461, 28.84184655352418858, 47.04930799450051637 ) ) ;
#1478 = DIRECTION ( 'NONE',  ( 1.000000000000000000, 0.000000000000000000, 0.000000000000000000 ) ) ;
#1479 = ORIENTED_EDGE ( 'NONE', *, *, #19983, .T. ) ;
#1480 = EDGE_LOOP ( 'NONE', ( #25592, #24123, #29450, #23747, #16266, #20918 ) ) ;
#1481 = CARTESIAN_POINT ( 'NONE',  ( 76.91070899933976079, -13.30632128221581212, 43.39636530629569933 ) ) ;
#1482 = DIRECTION ( 'NONE',  ( -1.000000000000000000, 0.000000000000000000, 0.000000000000000000 ) ) ;
#1483 = FACE_OUTER_BOUND ( 'NONE', #28820, .T. ) ;
#1484 = ORIENTED_EDGE ( 'NONE', *, *, #1026, .T. ) ;
#1485 = DIRECTION ( 'NONE',  ( -1.101824276508909887E-16, 1.000000000000000000, -0.000000000000000000 ) ) ;
#1486 = CARTESIAN_POINT ( 'NONE',  ( 24.90860134598588616, -13.74047052604243468, -11.17459240441505841 ) ) ;
#1487 = ORIENTED_EDGE ( 'NONE', *, *, #15824, .F. ) ;
#1488 = CARTESIAN_POINT ( 'NONE',  ( 67.79048676704638865, 13.68462854903246573, 47.04930799450051637 ) ) ;
#1489 = CARTESIAN_POINT ( 'NONE',  ( 44.77625694075214824, 28.81454579807170546, 48.23360063142255427 ) ) ;
#1490 = CIRCLE ( 'NONE', #7811, 12.36707279061065101 ) ;
#1491 = AXIS2_PLACEMENT_3D ( 'NONE', #13784, #18527, #23779 ) ;
#1492 = CARTESIAN_POINT ( 'NONE',  ( 33.72499318558949710, 29.34184655352418858, 47.04930799450051637 ) ) ;
#1493 = AXIS2_PLACEMENT_3D ( 'NONE', #20507, #7402, #30208 ) ;
#1494 =( BOUNDED_CURVE ( )  B_SPLINE_CURVE ( 3, ( #32024, #1823, #2317, #16914 ),
 .UNSPECIFIED., .F., .F. ) 
 B_SPLINE_CURVE_WITH_KNOTS ( ( 4, 4 ),
 ( 4.712388980384723425, 5.497787143782102426 ),
 .UNSPECIFIED. ) 
 CURVE ( )  GEOMETRIC_REPRESENTATION_ITEM ( )  RATIONAL_B_SPLINE_CURVE ( ( 1.000000000000000000, 0.9492530216742000038, 0.9492530216742000038, 1.000000000000000000 ) ) 
 REPRESENTATION_ITEM ( '' )  );
#1495 = AXIS2_PLACEMENT_3D ( 'NONE', #13900, #4203, #4037 ) ;
#1496 = TOROIDAL_SURFACE ( 'NONE', #19845, 78.39999999999999147, 0.1000000000000014350 ) ;
#1497 = ORIENTED_EDGE ( 'NONE', *, *, #22865, .F. ) ;
#1498 = CARTESIAN_POINT ( 'NONE',  ( -39.64148344771002286, 7.657122216028890982, 61.94930799450052206 ) ) ;
#1499 = CARTESIAN_POINT ( 'NONE',  ( 8.474859994195286461, 30.09143805560860585, 47.04930799450051637 ) ) ;
#1500 = CARTESIAN_POINT ( 'NONE',  ( -40.67014616567488616, 6.832698218566654269, 34.86215755014509909 ) ) ;
#1501 = CARTESIAN_POINT ( 'NONE',  ( 48.80717017713595141, 25.21952976649965805, 48.15820438821415195 ) ) ;
#1502 = ORIENTED_EDGE ( 'NONE', *, *, #7949, .T. ) ;
#1503 = FACE_OUTER_BOUND ( 'NONE', #29236, .T. ) ;
#1504 = DIRECTION ( 'NONE',  ( 0.000000000000000000, -0.000000000000000000, -1.000000000000000000 ) ) ;
#1505 = CARTESIAN_POINT ( 'NONE',  ( 7.596071960694297687, -5.098646251524523443, 47.04930799450052348 ) ) ;
#1506 = AXIS2_PLACEMENT_3D ( 'NONE', #10006, #14769, #22786 ) ;
#1507 = CIRCLE ( 'NONE', #12003, 12.27641737965281266 ) ;
#1508 = CARTESIAN_POINT ( 'NONE',  ( 44.21498992391908445, 26.59488759933318747, 46.89958605635244027 ) ) ;
#1509 = ADVANCED_FACE ( 'NONE', ( #13448 ), #18665, .F. ) ;
#1510 = DIRECTION ( 'NONE',  ( -1.000000000000000000, -1.101824276508909887E-16, 0.000000000000000000 ) ) ;
#1511 = CARTESIAN_POINT ( 'NONE',  ( 21.09785597605720042, -17.03545420775220265, 47.04930799450051637 ) ) ;
#1512 = EDGE_CURVE ( 'NONE', #14722, #4736, #3326, .T. ) ;
#1513 = ADVANCED_FACE ( 'NONE', ( #9149 ), #11780, .T. ) ;
#1514 = CYLINDRICAL_SURFACE ( 'NONE', #21014, 54.30000000000000426 ) ;
#1515 = ADVANCED_FACE ( 'NONE', ( #9644 ), #29174, .F. ) ;
#1516 = FILL_AREA_STYLE ('',( #3660 ) ) ;
#1517 = EDGE_LOOP ( 'NONE', ( #29288, #17413, #14062, #5917 ) ) ;
#1518 = DIRECTION ( 'NONE',  ( -1.101824276508909887E-16, 1.000000000000000000, -0.000000000000000000 ) ) ;
#1519 = CARTESIAN_POINT ( 'NONE',  ( 48.94625023931840246, 26.67124452788248945, 46.10640627770148825 ) ) ;
#1520 = DIRECTION ( 'NONE',  ( 3.629881133194233264E-17, 0.9550631830613039996, -0.2964022880492153122 ) ) ;
#1521 = VECTOR ( 'NONE', #32016, 1000.000000000000000 ) ;
#1522 = CARTESIAN_POINT ( 'NONE',  ( 5.811096063210362317, 14.98269195386757602, 47.04930799450052348 ) ) ;
#1523 = ORIENTED_EDGE ( 'NONE', *, *, #1031, .F. ) ;
#1524 = CARTESIAN_POINT ( 'NONE',  ( -39.54681582271551576, -5.935578394679064118, 77.88069024016000697 ) ) ;
#1525 = AXIS2_PLACEMENT_3D ( 'NONE', #173, #7567, #2636 ) ;
#1526 = CYLINDRICAL_SURFACE ( 'NONE', #624, 7.999999999999999112 ) ;
#1527 = CARTESIAN_POINT ( 'NONE',  ( -44.16105795751995799, -3.935454207752190126, 42.04930799450051637 ) ) ;
#1528 = ORIENTED_EDGE ( 'NONE', *, *, #15802, .T. ) ;
#1529 = CARTESIAN_POINT ( 'NONE',  ( -40.46271621608484281, 3.081581074246049212, 57.04930799450051637 ) ) ;
#1530 = CARTESIAN_POINT ( 'NONE',  ( 33.71785032049138664, 23.96664230456639899, 47.04930799450051637 ) ) ;
#1531 = DIRECTION ( 'NONE',  ( 1.000000000000000000, 0.000000000000000000, -1.224646799147353207E-16 ) ) ;
#1532 = ORIENTED_EDGE ( 'NONE', *, *, #7122, .T. ) ;
#1533 = CARTESIAN_POINT ( 'NONE',  ( 21.09785597605720042, -13.68834655544033652, 47.04930799450051637 ) ) ;
#1534 = EDGE_LOOP ( 'NONE', ( #7705, #28572, #22447, #27008 ) ) ;
#1535 = AXIS2_PLACEMENT_3D ( 'NONE', #14725, #29989, #106 ) ;
#1536 = AXIS2_PLACEMENT_3D ( 'NONE', #16619, #1054, #21066 ) ;
#1537 = ORIENTED_EDGE ( 'NONE', *, *, #16167, .F. ) ;
#1538 = EDGE_CURVE ( 'NONE', #16672, #11669, #29014, .T. ) ;
#1539 = ADVANCED_FACE ( 'NONE', ( #21613 ), #14826, .T. ) ;
#1540 = AXIS2_PLACEMENT_3D ( 'NONE', #4446, #23662, #19040 ) ;
#1541 = CIRCLE ( 'NONE', #1019, 12.62506659569710266 ) ;
#1542 = DIRECTION ( 'NONE',  ( 0.8746197071393926326, -0.4848096202463430537, -8.676864087101709653E-18 ) ) ;
#1543 = CYLINDRICAL_SURFACE ( 'NONE', #29774, 31.50000000000000000 ) ;
#1544 = DIRECTION ( 'NONE',  ( 0.4848096202463424431, 0.8746197071393927436, -2.220446049250312588E-16 ) ) ;
#1545 = AXIS2_PLACEMENT_3D ( 'NONE', #3835, #18755, #3997 ) ;
#1546 = VERTEX_POINT ( 'NONE', #29669 ) ;
#1547 = DIRECTION ( 'NONE',  ( 1.000000000000000000, 0.000000000000000000, -1.224646799147353207E-16 ) ) ;
#1548 = ORIENTED_EDGE ( 'NONE', *, *, #14796, .F. ) ;
#1549 = CARTESIAN_POINT ( 'NONE',  ( 21.09785597605720753, -17.03545420775220265, 117.6483275080933169 ) ) ;
#1550 = EDGE_CURVE ( 'NONE', #1830, #10311, #6857, .T. ) ;
#1551 = ORIENTED_EDGE ( 'NONE', *, *, #30547, .T. ) ;
#1552 = DIRECTION ( 'NONE',  ( -0.000000000000000000, 1.000000000000000000, -0.000000000000000000 ) ) ;
#1553 = DIRECTION ( 'NONE',  ( 0.000000000000000000, -0.000000000000000000, -1.000000000000000000 ) ) ;
#1554 = CARTESIAN_POINT ( 'NONE',  ( -40.41647043964083252, 8.356895951721259763, 54.44930799450051495 ) ) ;
#1555 =( NAMED_UNIT ( * ) PLANE_ANGLE_UNIT ( ) SI_UNIT ( $, .RADIAN. ) );
#1556 = AXIS2_PLACEMENT_3D ( 'NONE', #19758, #17627, #12558 ) ;
#1557 = AXIS2_PLACEMENT_3D ( 'NONE', #8265, #28289, #5810 ) ;
#1558 = ORIENTED_EDGE ( 'NONE', *, *, #7947, .T. ) ;
#1559 = CARTESIAN_POINT ( 'NONE',  ( 46.45846941443645761, 22.99884124225578930, 45.79590206249746132 ) ) ;
#1560 = DIRECTION ( 'NONE',  ( -1.000000000000000000, 0.000000000000000000, 0.000000000000000000 ) ) ;
#1561 = CARTESIAN_POINT ( 'NONE',  ( 33.46699938050303302, 38.56284415653841791, 47.04930799450051637 ) ) ;
#1562 = DIRECTION ( 'NONE',  ( 0.000000000000000000, 0.000000000000000000, -1.000000000000000000 ) ) ;
#1563 = CARTESIAN_POINT ( 'NONE',  ( -35.12632216515690686, 11.92558985988973674, 40.04930799450050216 ) ) ;
#1564 = VERTEX_POINT ( 'NONE', #24406 ) ;
#1565 = CARTESIAN_POINT ( 'NONE',  ( -40.18126594841540822, 7.055686659393786364, 34.94323797956834454 ) ) ;
#1566 = DIRECTION ( 'NONE',  ( -0.000000000000000000, -1.000000000000000000, 0.000000000000000000 ) ) ;
#1567 = VERTEX_POINT ( 'NONE', #7175 ) ;
#1568 = FACE_OUTER_BOUND ( 'NONE', #14914, .T. ) ;
#1569 = TOROIDAL_SURFACE ( 'NONE', #2111, 41.50000000000000000, 1.999999999999998224 ) ;
#1570 = AXIS2_PLACEMENT_3D ( 'NONE', #7904, #5439, #15768 ) ;
#1571 = LINE ( 'NONE', #16660, #17978 ) ;
#1572 = ORIENTED_EDGE ( 'NONE', *, *, #13901, .T. ) ;
#1573 = AXIS2_PLACEMENT_3D ( 'NONE', #2497, #15138, #12523 ) ;
#1574 = EDGE_CURVE ( 'NONE', #5070, #14564, #7015, .T. ) ;
#1575 = ORIENTED_EDGE ( 'NONE', *, *, #22675, .F. ) ;
#1576 = AXIS2_PLACEMENT_3D ( 'NONE', #20462, #28021, #8318 ) ;
#1577 = TOROIDAL_SURFACE ( 'NONE', #26742, 1.524998423334081643, 0.1000000000000000056 ) ;
#1578 = EDGE_CURVE ( 'NONE', #29191, #20681, #12935, .T. ) ;
#1579 = ORIENTED_EDGE ( 'NONE', *, *, #29541, .F. ) ;
#1580 = EDGE_CURVE ( 'NONE', #2178, #10687, #25386, .T. ) ;
#1581 = AXIS2_PLACEMENT_3D ( 'NONE', #4798, #14977, #16932 ) ;
#1582 = EDGE_CURVE ( 'NONE', #18712, #25136, #9969, .T. ) ;
#1583 = LINE ( 'NONE', #26862, #8802 ) ;
#1584 = CIRCLE ( 'NONE', #16870, 0.09999999999999978351 ) ;
#1585 = AXIS2_PLACEMENT_3D ( 'NONE', #20292, #30323, #1560 ) ;
#1586 = VERTEX_POINT ( 'NONE', #22759 ) ;
#1587 = FACE_OUTER_BOUND ( 'NONE', #8169, .T. ) ;
#1588 = CARTESIAN_POINT ( 'NONE',  ( -40.69193635511749108, 9.347952559758583746, 39.44930799450052206 ) ) ;
#1589 = CYLINDRICAL_SURFACE ( 'NONE', #7623, 25.50000000000000355 ) ;
#1590 = DIRECTION ( 'NONE',  ( -0.000000000000000000, -1.000000000000000000, -0.000000000000000000 ) ) ;
#1591 = CARTESIAN_POINT ( 'NONE',  ( 45.81741271322955100, 28.54452976649965024, 49.02305402274571122 ) ) ;
#1592 = AXIS2_PLACEMENT_3D ( 'NONE', #8643, #21258, #11114 ) ;
#1593 = ADVANCED_FACE ( 'NONE', ( #30489 ), #27398, .T. ) ;
#1594 = CIRCLE ( 'NONE', #5809, 12.36707279061065101 ) ;
#1595 = ORIENTED_EDGE ( 'NONE', *, *, #19844, .T. ) ;
#1596 = CARTESIAN_POINT ( 'NONE',  ( 21.09992658989239089, 24.97145308207319303, 47.04930799450051637 ) ) ;
#1597 = ORIENTED_EDGE ( 'NONE', *, *, #31123, .F. ) ;
#1598 = AXIS2_PLACEMENT_3D ( 'NONE', #20368, #5295, #15139 ) ;
#1599 = ORIENTED_EDGE ( 'NONE', *, *, #28935, .T. ) ;
#1600 = DIRECTION ( 'NONE',  ( 0.000000000000000000, 0.000000000000000000, 1.000000000000000000 ) ) ;
#1601 = PLANE ( 'NONE',  #30450 ) ;
#1602 = CARTESIAN_POINT ( 'NONE',  ( -40.68074350590692490, 6.811995273159344499, 39.41969944873108744 ) ) ;
#1603 = FACE_OUTER_BOUND ( 'NONE', #20703, .T. ) ;
#1604 = CARTESIAN_POINT ( 'NONE',  ( 33.72499318558949710, 26.09143805560860940, 47.04930799450051637 ) ) ;
#1605 = CARTESIAN_POINT ( 'NONE',  ( 49.28428300279882990, 26.24787913140504614, 48.46772541801551171 ) ) ;
#1606 = CARTESIAN_POINT ( 'NONE',  ( 46.94469835654546586, 23.12036939723557083, 47.28539358874152043 ) ) ;
#1607 = CYLINDRICAL_SURFACE ( 'NONE', #24275, 2.499999999999997335 ) ;
#1608 = ORIENTED_EDGE ( 'NONE', *, *, #11781, .T. ) ;
#1609 = DIRECTION ( 'NONE',  ( 0.9612616959383205595, 0.2756373558169931681, -1.660411357259282445E-16 ) ) ;
#1610 = DIRECTION ( 'NONE',  ( -0.8746197071393926326, 0.4848096202463430537, 8.676864087101709653E-18 ) ) ;
#1611 = VECTOR ( 'NONE', #3459, 1000.000000000000114 ) ;
#1612 = DIRECTION ( 'NONE',  ( -1.101824276508909887E-16, 1.000000000000000000, -0.000000000000000000 ) ) ;
#1613 = DIRECTION ( 'NONE',  ( -0.000000000000000000, -1.000000000000000000, 0.000000000000000000 ) ) ;
#1614 = CARTESIAN_POINT ( 'NONE',  ( -40.51565501380215295, 9.065589196111961456, 56.04611646155296256 ) ) ;
#1615 = ORIENTED_EDGE ( 'NONE', *, *, #25392, .F. ) ;
#1616 = DIRECTION ( 'NONE',  ( -0.000000000000000000, -1.000000000000000000, 0.000000000000000000 ) ) ;
#1617 = EDGE_CURVE ( 'NONE', #26367, #2133, #27487, .T. ) ;
#1618 = ORIENTED_EDGE ( 'NONE', *, *, #5754, .T. ) ;
#1619 = FACE_OUTER_BOUND ( 'NONE', #12270, .T. ) ;
#1620 = FACE_OUTER_BOUND ( 'NONE', #14364, .T. ) ;
#1621 = EDGE_CURVE ( 'NONE', #27550, #112, #2254, .T. ) ;
#1622 = EDGE_LOOP ( 'NONE', ( #2552, #10221, #21109 ) ) ;
#1623 = VECTOR ( 'NONE', #1124, 1000.000000000000000 ) ;
#1624 = CIRCLE ( 'NONE', #32023, 69.59901951359279337 ) ;
#1625 = AXIS2_PLACEMENT_3D ( 'NONE', #26803, #31574, #31889 ) ;
#1626 = EDGE_CURVE ( 'NONE', #3661, #31739, #30026, .T. ) ;
#1627 = ADVANCED_FACE ( 'NONE', ( #7342 ), #12200, .T. ) ;
#1628 = ORIENTED_EDGE ( 'NONE', *, *, #5035, .F. ) ;
#1629 = CARTESIAN_POINT ( 'NONE',  ( 21.09785597605719332, 15.63322284159649556, -0.008722863421593840538 ) ) ;
#1630 = FACE_OUTER_BOUND ( 'NONE', #22733, .T. ) ;
#1631 = DIRECTION ( 'NONE',  ( -0.3958453973319808195, -0.7141240004913296247, -0.5773502691896363892 ) ) ;
#1632 = AXIS2_PLACEMENT_3D ( 'NONE', #17122, #14681, #14197 ) ;
#1633 = ORIENTED_EDGE ( 'NONE', *, *, #8614, .T. ) ;
#1634 = CARTESIAN_POINT ( 'NONE',  ( -43.90780810587784089, -0.03953120679776400692, 62.04930799450052348 ) ) ;
#1635 = CARTESIAN_POINT ( 'NONE',  ( -40.57861772207635198, 7.624524047285945905, 60.14124254659545699 ) ) ;
#1636 = CARTESIAN_POINT ( 'NONE',  ( 75.71263776093286424, -1.580002914024330574, 13.40786461638758098 ) ) ;
#1637 = ORIENTED_EDGE ( 'NONE', *, *, #10423, .T. ) ;
#1638 = DIRECTION ( 'NONE',  ( 0.9761574614375596592, 0.2110602665713100790, 0.05069688703093150339 ) ) ;
#1639 = VERTEX_POINT ( 'NONE', #5206 ) ;
#1640 = AXIS2_PLACEMENT_3D ( 'NONE', #1082, #605, #20783 ) ;
#1641 = LINE ( 'NONE', #1475, #10773 ) ;
#1642 = DIRECTION ( 'NONE',  ( -1.101824276508909887E-16, 1.000000000000000000, -0.000000000000000000 ) ) ;
#1643 = CIRCLE ( 'NONE', #21059, 0.1000000000000007688 ) ;
#1644 = DIRECTION ( 'NONE',  ( 0.9612616959383194493, 0.2756373558169974980, 8.795445018804946186E-19 ) ) ;
#1645 = AXIS2_PLACEMENT_3D ( 'NONE', #2215, #7303, #27489 ) ;
#1646 = DIRECTION ( 'NONE',  ( 0.000000000000000000, 0.000000000000000000, 1.000000000000000000 ) ) ;
#1647 = ORIENTED_EDGE ( 'NONE', *, *, #18364, .T. ) ;
#1648 = EDGE_LOOP ( 'NONE', ( #4268, #16046, #1915, #601, #20806, #11239, #20230, #2720, #2294, #16738, #10326, #17722, #18135, #11663 ) ) ;
#1649 = AXIS2_PLACEMENT_3D ( 'NONE', #31446, #1395, #8950 ) ;
#1650 = CYLINDRICAL_SURFACE ( 'NONE', #30215, 13.50178401536290806 ) ;
#1651 = CYLINDRICAL_SURFACE ( 'NONE', #17206, 1.199999999999999734 ) ;
#1652 = FACE_BOUND ( 'NONE', #19233, .T. ) ;
#1653 = ORIENTED_EDGE ( 'NONE', *, *, #13052, .F. ) ;
#1654 = CARTESIAN_POINT ( 'NONE',  ( -9.316012264051970249, 5.323792735596123649, -5.040144599709082129 ) ) ;
#1655 = CARTESIAN_POINT ( 'NONE',  ( 64.96297466771234497, -13.74047052604243646, 85.52521890125203186 ) ) ;
#1656 = ADVANCED_FACE ( 'NONE', ( #14735 ), #12274, .F. ) ;
#1657 = ORIENTED_EDGE ( 'NONE', *, *, #29871, .F. ) ;
#1658 = CARTESIAN_POINT ( 'NONE',  ( 21.09785597605720042, -13.64309448858209528, 47.04930799450051637 ) ) ;
#1659 = FACE_OUTER_BOUND ( 'NONE', #30379, .T. ) ;
#1660 = CIRCLE ( 'NONE', #29454, 0.1249999999999983763 ) ;
#1661 = CARTESIAN_POINT ( 'NONE',  ( 21.09785597605719332, -19.93545420775220123, 67.04930799450050927 ) ) ;
#1662 = EDGE_CURVE ( 'NONE', #14460, #7845, #17435, .T. ) ;
#1663 = ORIENTED_EDGE ( 'NONE', *, *, #18980, .T. ) ;
#1664 = AXIS2_PLACEMENT_3D ( 'NONE', #2940, #17556, #20664 ) ;
#1665 = VECTOR ( 'NONE', #9472, 1000.000000000000000 ) ;
#1666 = CIRCLE ( 'NONE', #5885, 0.1000000000000018235 ) ;
#1667 = CARTESIAN_POINT ( 'NONE',  ( -41.23380787120766655, 11.23768311167744294, 38.09144330556765112 ) ) ;
#1668 = DIRECTION ( 'NONE',  ( -0.6184495258776567805, 0.3428121700606641120, 0.7071067811865474617 ) ) ;
#1669 = CARTESIAN_POINT ( 'NONE',  ( -40.61197514715824752, 6.966360136513624290, 35.08795977352291118 ) ) ;
#1670 = CARTESIAN_POINT ( 'NONE',  ( 45.79384627280941089, 28.56618040159425931, 49.05938063676249072 ) ) ;
#1671 = ORIENTED_EDGE ( 'NONE', *, *, #9993, .F. ) ;
#1672 = FACE_OUTER_BOUND ( 'NONE', #25999, .T. ) ;
#1673 = LINE ( 'NONE', #8899, #26101 ) ;
#1674 = AXIS2_PLACEMENT_3D ( 'NONE', #9447, #19766, #14863 ) ;
#1675 = CARTESIAN_POINT ( 'NONE',  ( 54.84591317376816022, -2.578969365796082158, -7.209533676615418329 ) ) ;
#1676 = DIRECTION ( 'NONE',  ( 0.1949050434465325055, -0.6797146636928671493, 0.7071067811865460184 ) ) ;
#1677 = DIRECTION ( 'NONE',  ( 0.8746197071393926326, -0.4848096202463430537, -8.676864087101709653E-18 ) ) ;
#1678 = FACE_BOUND ( 'NONE', #7087, .T. ) ;
#1679 = DIRECTION ( 'NONE',  ( 0.000000000000000000, -0.000000000000000000, -1.000000000000000000 ) ) ;
#1680 = VECTOR ( 'NONE', #31721, 1000.000000000000000 ) ;
#1681 = DIRECTION ( 'NONE',  ( -1.000000000000000000, -1.101824276508910010E-16, 0.000000000000000000 ) ) ;
#1682 =( LENGTH_UNIT ( ) NAMED_UNIT ( * ) SI_UNIT ( .MILLI., .METRE. ) );
#1683 = ORIENTED_EDGE ( 'NONE', *, *, #28988, .F. ) ;
#1684 = CARTESIAN_POINT ( 'NONE',  ( 46.04302072787191946, 22.93328494799376571, 45.69307819878901000 ) ) ;
#1685 = DIRECTION ( 'NONE',  ( 0.9612616959383221138, 0.2756373558169876170, 0.000000000000000000 ) ) ;
#1686 = CIRCLE ( 'NONE', #17409, 0.09999999999999795164 ) ;
#1687 = CARTESIAN_POINT ( 'NONE',  ( 21.09992658989238734, 31.59143805560860585, 47.04930799450051637 ) ) ;
#1688 = CARTESIAN_POINT ( 'NONE',  ( -41.07644103349281295, 9.237697617431788188, 34.64930799450051779 ) ) ;
#1689 = ORIENTED_EDGE ( 'NONE', *, *, #14950, .F. ) ;
#1690 = CIRCLE ( 'NONE', #18969, 0.1250000000000001110 ) ;
#1691 =( BOUNDED_CURVE ( )  B_SPLINE_CURVE ( 3, ( #9357, #24286, #9522, #9195 ),
 .UNSPECIFIED., .F., .F. ) 
 B_SPLINE_CURVE_WITH_KNOTS ( ( 4, 4 ),
 ( 1.099063246724959253, 1.220321128156879542 ),
 .UNSPECIFIED. ) 
 CURVE ( )  GEOMETRIC_REPRESENTATION_ITEM ( )  RATIONAL_B_SPLINE_CURVE ( ( 1.000000000000000000, 0.9987750858034806223, 0.9987750858034806223, 1.000000000000000000 ) ) 
 REPRESENTATION_ITEM ( '' )  );
#1692 = CARTESIAN_POINT ( 'NONE',  ( 21.09785597605720753, 13.86454579224779948, 47.04930799450052348 ) ) ;
#1693 = CARTESIAN_POINT ( 'NONE',  ( -42.22138300640814634, 14.68176690255379313, 36.00717268343339583 ) ) ;
#1694 = DIRECTION ( 'NONE',  ( -1.101824276508909887E-16, 1.000000000000000000, -0.000000000000000000 ) ) ;
#1695 = EDGE_LOOP ( 'NONE', ( #32328, #18815, #6147, #19536 ) ) ;
#1696 = DIRECTION ( 'NONE',  ( -1.101824276508909887E-16, 1.000000000000000000, -0.000000000000000000 ) ) ;
#1697 = CARTESIAN_POINT ( 'NONE',  ( 21.09785597605720753, 14.86454579224779948, 47.04930799450052348 ) ) ;
#1698 = LINE ( 'NONE', #6468, #5751 ) ;
#1699 = DIRECTION ( 'NONE',  ( -1.000000000000000000, 0.000000000000000000, 2.775557561562888984E-15 ) ) ;
#1700 = ORIENTED_EDGE ( 'NONE', *, *, #27158, .F. ) ;
#1701 = CARTESIAN_POINT ( 'NONE',  ( 72.51299575579318457, 10.39233698702945929, 21.28292367868997204 ) ) ;
#1702 = EDGE_LOOP ( 'NONE', ( #19188, #4075, #21485, #17491 ) ) ;
#1703 = EDGE_CURVE ( 'NONE', #22782, #13582, #17947, .T. ) ;
#1704 = ORIENTED_EDGE ( 'NONE', *, *, #19291, .T. ) ;
#1705 = EDGE_CURVE ( 'NONE', #3673, #7331, #3796, .T. ) ;
#1706 = EDGE_CURVE ( 'NONE', #17323, #12553, #24768, .T. ) ;
#1707 = AXIS2_PLACEMENT_3D ( 'NONE', #28904, #26587, #9527 ) ;
#1708 = EDGE_CURVE ( 'NONE', #32242, #3463, #29778, .T. ) ;
#1709 = EDGE_CURVE ( 'NONE', #3673, #31872, #30548, .T. ) ;
#1710 = AXIS2_PLACEMENT_3D ( 'NONE', #9678, #29704, #7209 ) ;
#1711 = EDGE_CURVE ( 'NONE', #26418, #21141, #17412, .T. ) ;
#1712 = DIRECTION ( 'NONE',  ( -0.2756373558170082672, 0.9612616959383162296, 0.000000000000000000 ) ) ;
#1713 = VECTOR ( 'NONE', #6688, 1000.000000000000000 ) ;
#1714 = AXIS2_PLACEMENT_3D ( 'NONE', #23583, #11123, #10807 ) ;
#1715 = DIRECTION ( 'NONE',  ( -0.1949050434465267878, 0.6797146636928665941, -0.7071067811865480168 ) ) ;
#1716 = CARTESIAN_POINT ( 'NONE',  ( -29.68171735516254373, 11.15114065686176303, 71.33410141647549096 ) ) ;
#1717 = CARTESIAN_POINT ( 'NONE',  ( 81.75997733922811506, -5.936629510748242744, 77.99024554604916659 ) ) ;
#1718 = ORIENTED_EDGE ( 'NONE', *, *, #12170, .T. ) ;
#1719 = CARTESIAN_POINT ( 'NONE',  ( 21.09785597605720753, 14.81645899701909563, 47.04930799450052348 ) ) ;
#1720 = ORIENTED_EDGE ( 'NONE', *, *, #11473, .F. ) ;
#1721 = SURFACE_SIDE_STYLE ('',( #4019 ) ) ;
#1722 = CARTESIAN_POINT ( 'NONE',  ( -40.23971823762673239, 6.784144620117122493, 53.54930799450051637 ) ) ;
#1723 = ORIENTED_EDGE ( 'NONE', *, *, #1399, .F. ) ;
#1724 = DIRECTION ( 'NONE',  ( 0.8746197071393925215, -0.4848096202463429982, -8.676864087101708112E-18 ) ) ;
#1725 = CARTESIAN_POINT ( 'NONE',  ( 21.09992658989238734, 38.56284415653841791, 47.04930799450051637 ) ) ;
#1726 =( NAMED_UNIT ( * ) SI_UNIT ( $, .STERADIAN. ) SOLID_ANGLE_UNIT ( ) );
#1727 = DIRECTION ( 'NONE',  ( 0.000000000000000000, 0.000000000000000000, 1.000000000000000000 ) ) ;
#1728 = LINE ( 'NONE', #4849, #7403 ) ;
#1729 = FACE_OUTER_BOUND ( 'NONE', #28058, .T. ) ;
#1730 = AXIS2_PLACEMENT_3D ( 'NONE', #27571, #5086, #25109 ) ;
#1731 = CARTESIAN_POINT ( 'NONE',  ( 8.732853799281738105, 30.46183152705961561, 47.04930799450051637 ) ) ;
#1732 = ORIENTED_EDGE ( 'NONE', *, *, #16074, .T. ) ;
#1733 = CARTESIAN_POINT ( 'NONE',  ( 21.09992658989239089, 28.09164230456639544, 47.04930799450051637 ) ) ;
#1734 = CYLINDRICAL_SURFACE ( 'NONE', #11748, 12.36707279061065279 ) ;
#1735 = AXIS2_PLACEMENT_3D ( 'NONE', #18661, #1113, #9306 ) ;
#1736 = ORIENTED_EDGE ( 'NONE', *, *, #28675, .T. ) ;
#1738 = ADVANCED_FACE ( 'NONE', ( #11110 ), #26184, .F. ) ;
#1737 = CARTESIAN_POINT ( 'NONE',  ( -44.28695544631908376, -5.935454207752205669, 40.04930799450050216 ) ) ;
#1739 = DIRECTION ( 'NONE',  ( -1.101824276508909887E-16, 1.000000000000000000, -0.000000000000000000 ) ) ;
#1740 = ORIENTED_EDGE ( 'NONE', *, *, #6664, .F. ) ;
#1741 = CIRCLE ( 'NONE', #24274, 12.36707279061065101 ) ;
#1742 = VECTOR ( 'NONE', #28385, 1000.000000000000000 ) ;
#1743 = ORIENTED_EDGE ( 'NONE', *, *, #5029, .F. ) ;
#1744 = ORIENTED_EDGE ( 'NONE', *, *, #22791, .F. ) ;
#1745 = EDGE_CURVE ( 'NONE', #2754, #8819, #23410, .T. ) ;
#1746 = EDGE_CURVE ( 'NONE', #17665, #27575, #6430, .T. ) ;
#1747 = TOROIDAL_SURFACE ( 'NONE', #3839, 1.100000000000000089, 0.1000000000000000056 ) ;
#1748 = AXIS2_PLACEMENT_3D ( 'NONE', #5290, #25308, #30395 ) ;
#1749 = CARTESIAN_POINT ( 'NONE',  ( -41.91799733298572761, 13.87669230940966969, 54.58433102282629079 ) ) ;
#1750 = APPLICATION_CONTEXT ( 'automotive_design' ) ;
#1751 = ORIENTED_EDGE ( 'NONE', *, *, #19877, .F. ) ;
#1752 = CARTESIAN_POINT ( 'NONE',  ( 21.09992658989239089, 25.46183152705960140, 47.04930799450051637 ) ) ;
#1753 = AXIS2_PLACEMENT_3D ( 'NONE', #7802, #25993, #23048 ) ;
#1754 = DIRECTION ( 'NONE',  ( -1.101824276508909887E-16, 1.000000000000000000, -0.000000000000000000 ) ) ;
#1755 = VECTOR ( 'NONE', #11846, 1000.000000000000000 ) ;
#1756 = CIRCLE ( 'NONE', #28514, 0.1250000000000001110 ) ;
#1757 = CARTESIAN_POINT ( 'NONE',  ( 48.37020515026796375, 25.16454579224780019, 49.54352682589573220 ) ) ;
#1758 = DIRECTION ( 'NONE',  ( -1.101824276508909887E-16, 1.000000000000000000, -0.000000000000000000 ) ) ;
#1759 = CARTESIAN_POINT ( 'NONE',  ( 45.28286642839709231, 26.38619643316631524, 47.97516931882780966 ) ) ;
#1760 = ORIENTED_EDGE ( 'NONE', *, *, #5361, .T. ) ;
#1761 = CARTESIAN_POINT ( 'NONE',  ( -42.12525683681430877, 14.70933063813549424, 37.04930799450052348 ) ) ;
#1762 = ORIENTED_EDGE ( 'NONE', *, *, #31648, .F. ) ;
#1763 = CARTESIAN_POINT ( 'NONE',  ( -12.56410411622038303, -3.374355247260697244, -7.781004297996404695 ) ) ;
#1764 = VERTEX_POINT ( 'NONE', #15694 ) ;
#1766 = EDGE_CURVE ( 'NONE', #12417, #27575, #16173, .T. ) ;
#1765 = CARTESIAN_POINT ( 'NONE',  ( 49.06626442724220283, 29.56259918706335910, 46.29368314320814193 ) ) ;
#1767 = FACE_OUTER_BOUND ( 'NONE', #3133, .T. ) ;
#1768 = DIRECTION ( 'NONE',  ( -0.000000000000000000, -1.000000000000000000, 0.000000000000000000 ) ) ;
#1769 = CARTESIAN_POINT ( 'NONE',  ( 8.732853799281734553, 38.56284415653841791, 47.04930799450051637 ) ) ;
#1770 = DIRECTION ( 'NONE',  ( -1.000000000000000000, 0.000000000000000000, 0.000000000000000000 ) ) ;
#1771 = CARTESIAN_POINT ( 'NONE',  ( 46.96268396749378127, 26.83121246473837473, 49.65201805493727960 ) ) ;
#1772 = CARTESIAN_POINT ( 'NONE',  ( 47.33078969507813838, 23.03451764446789696, 48.23582531347169322 ) ) ;
#1773 = CYLINDRICAL_SURFACE ( 'NONE', #24803, 7.999999999999999112 ) ;
#1774 = VERTEX_POINT ( 'NONE', #18309 ) ;
#1775 = CARTESIAN_POINT ( 'NONE',  ( 33.71785032049135111, 27.46664230456639899, 47.04930799450051637 ) ) ;
#1777 = EDGE_CURVE ( 'NONE', #29734, #15549, #28017, .T. ) ;
#1776 = CARTESIAN_POINT ( 'NONE',  ( -4.402144023942796025, 13.86454579224779948, 47.04930799450052348 ) ) ;
#1778 = DIRECTION ( 'NONE',  ( 1.234978253042719660E-16, -1.000000000000000000, -1.109335647967047851E-31 ) ) ;
#1779 = EDGE_CURVE ( 'NONE', #24681, #28894, #7495, .T. ) ;
#1780 = CIRCLE ( 'NONE', #13322, 12.27641737965283042 ) ;
#1781 = DIRECTION ( 'NONE',  ( -1.000000000000000000, 0.000000000000000000, 0.000000000000000000 ) ) ;
#1782 = FACE_OUTER_BOUND ( 'NONE', #24200, .T. ) ;
#1783 = ORIENTED_EDGE ( 'NONE', *, *, #8175, .F. ) ;
#1784 = CARTESIAN_POINT ( 'NONE',  ( 33.72499318558949710, 30.59184655352422411, 47.04930799450051637 ) ) ;
#1785 = ORIENTED_EDGE ( 'NONE', *, *, #13241, .T. ) ;
#1786 = CARTESIAN_POINT ( 'NONE',  ( 21.09992658989238734, 38.56284415653841791, 47.04930799450051637 ) ) ;
#1787 = DIRECTION ( 'NONE',  ( 0.000000000000000000, 0.000000000000000000, -1.000000000000000000 ) ) ;
#1788 = B_SPLINE_CURVE_WITH_KNOTS ( 'NONE', 3,
 ( #12617, #7026, #17024, #27046, #12286, #14580, #22280, #32308, #9819, #4896, #14909, #8444, #20748, #23697, #13224, #23533, #25991, #18275, #23851, #28306, #5826, #26153, #21217, #6134 ),
 .UNSPECIFIED., .F., .F.,
 ( 4, 2, 2, 2, 2, 2, 2, 2, 2, 2, 2, 4 ),
 ( 1.395353767516851130E-14, 2.664078908521907074E-05, 3.996118362085184644E-05, 4.662138088866923718E-05, 5.328157815648662115E-05, 6.660197269212707436E-05, 7.992236722776753434E-05, 0.0001065631562990277190, 0.0002131263125840656791, 0.0004262526251541395124, 0.0008525052502942665790, 0.001705010500574540011 ),
 .UNSPECIFIED. ) ;
#1789 = VECTOR ( 'NONE', #16656, 1000.000000000000000 ) ;
#1790 = VERTEX_POINT ( 'NONE', #20937 ) ;
#1791 = ADVANCED_FACE ( 'NONE', ( #17996 ), #8000, .F. ) ;
#1792 = ORIENTED_EDGE ( 'NONE', *, *, #16762, .F. ) ;
#1793 = CARTESIAN_POINT ( 'NONE',  ( 8.823509210239526723, 26.09164230456639899, 47.04930799450051637 ) ) ;
#1794 = CARTESIAN_POINT ( 'NONE',  ( 21.09785597605719332, 15.06454579224778456, 102.0493079945005093 ) ) ;
#1795 = CARTESIAN_POINT ( 'NONE',  ( 33.50134396954518223, 32.59164230456639899, 47.04930799450051637 ) ) ;
#1796 = VERTEX_POINT ( 'NONE', #23083 ) ;
#1797 = VECTOR ( 'NONE', #18419, 1000.000000000000114 ) ;
#1798 = CARTESIAN_POINT ( 'NONE',  ( 46.18657129672061501, 22.93807716476589675, 45.61868866909985343 ) ) ;
#1799 = CARTESIAN_POINT ( 'NONE',  ( -43.68921302925062378, 1.179890886355840163, 39.54930799450052348 ) ) ;
#1800 = CARTESIAN_POINT ( 'NONE',  ( 78.44397203118849404, -5.043292969097946887, 14.24782339319855318 ) ) ;
#1801 = EDGE_CURVE ( 'NONE', #17244, #15830, #19463, .T. ) ;
#1802 = ORIENTED_EDGE ( 'NONE', *, *, #6040, .T. ) ;
#1803 = VERTEX_POINT ( 'NONE', #28179 ) ;
#1804 = CARTESIAN_POINT ( 'NONE',  ( -40.61178118339597631, 9.038025460530262123, 56.14611646155296398 ) ) ;
#1805 = ORIENTED_EDGE ( 'NONE', *, *, #30808, .T. ) ;
#1806 = ADVANCED_FACE ( 'NONE', ( #16019 ), #14235, .F. ) ;
#1807 = CIRCLE ( 'NONE', #31687, 1.000000000000000888 ) ;
#1808 = CARTESIAN_POINT ( 'NONE',  ( 21.09785597605719332, -15.93545420775219945, 126.2593585008393831 ) ) ;
#1809 = CARTESIAN_POINT ( 'NONE',  ( -45.58211410561983001, -5.881662548112003286, 40.51623134221831890 ) ) ;
#1810 =( LENGTH_UNIT ( ) NAMED_UNIT ( * ) SI_UNIT ( .MILLI., .METRE. ) );
#1811 = ORIENTED_EDGE ( 'NONE', *, *, #16257, .F. ) ;
#1812 = VERTEX_POINT ( 'NONE', #5865 ) ;
#1813 = CARTESIAN_POINT ( 'NONE',  ( 21.09992658989239089, 27.59164230456639544, 47.04930799450051637 ) ) ;
#1814 = FACE_OUTER_BOUND ( 'NONE', #2795, .T. ) ;
#1815 = EDGE_CURVE ( 'NONE', #27059, #10602, #6898, .T. ) ;
#1816 = EDGE_CURVE ( 'NONE', #22757, #5318, #622, .T. ) ;
#1817 = DIRECTION ( 'NONE',  ( 0.000000000000000000, 0.000000000000000000, -1.000000000000000000 ) ) ;
#1818 = ORIENTED_EDGE ( 'NONE', *, *, #5124, .F. ) ;
#1819 = CARTESIAN_POINT ( 'NONE',  ( -11.94109704398765537, 0.4256545730735167288, -6.630874157835914495 ) ) ;
#1820 = FACE_OUTER_BOUND ( 'NONE', #8386, .T. ) ;
#1821 = EDGE_LOOP ( 'NONE', ( #10516, #4936, #4488, #13134 ) ) ;
#1822 = DIRECTION ( 'NONE',  ( 0.000000000000000000, 0.000000000000000000, -1.000000000000000000 ) ) ;
#1823 = CARTESIAN_POINT ( 'NONE',  ( -40.61463551858321352, 9.441168033762322054, 39.41901908761455786 ) ) ;
#1824 = DIRECTION ( 'NONE',  ( -0.1949050434465283144, 0.6797146636928674823, 0.7071067811865467956 ) ) ;
#1825 = VECTOR ( 'NONE', #8073, 1000.000000000000000 ) ;
#1826 = AXIS2_PLACEMENT_3D ( 'NONE', #16899, #16723, #19189 ) ;
#1827 = AXIS2_PLACEMENT_3D ( 'NONE', #13329, #10539, #25781 ) ;
#1828 = VECTOR ( 'NONE', #26022, 1000.000000000000000 ) ;
#1829 = AXIS2_PLACEMENT_3D ( 'NONE', #31153, #1104, #26213 ) ;
#1830 = VERTEX_POINT ( 'NONE', #15865 ) ;
#1831 = FACE_OUTER_BOUND ( 'NONE', #26578, .T. ) ;
#1832 = FACE_OUTER_BOUND ( 'NONE', #19834, .T. ) ;
#1833 = CARTESIAN_POINT ( 'NONE',  ( -40.18454328187963398, 7.548069831825862330, 60.44930799450051495 ) ) ;
#1834 = CARTESIAN_POINT ( 'NONE',  ( 44.70507715278255745, 28.44951373492759217, 46.92503878583765697 ) ) ;
#1835 = ORIENTED_EDGE ( 'NONE', *, *, #9572, .T. ) ;
#1836 = CARTESIAN_POINT ( 'NONE',  ( 21.09992658989239089, 29.84164230456639899, 47.04930799450051637 ) ) ;
#1837 = EDGE_CURVE ( 'NONE', #5204, #8602, #26814, .T. ) ;
#1838 = PLANE ( 'NONE',  #31511 ) ;
#1839 = ADVANCED_FACE ( 'NONE', ( #31129, #10942 ), #30649, .T. ) ;
#1840 = CARTESIAN_POINT ( 'NONE',  ( 21.09992658989239089, 28.96664230456639899, 47.04930799450051637 ) ) ;
#1841 = CARTESIAN_POINT ( 'NONE',  ( 21.09785597605720397, -15.43545420775221366, -24.95069200549946586 ) ) ;
#1842 = CARTESIAN_POINT ( 'NONE',  ( 21.09785597605719332, -13.74048473023143835, -11.17459240385188934 ) ) ;
#1843 = CARTESIAN_POINT ( 'NONE',  ( -41.13768170161382898, 11.26524684725914227, 37.04930799450052348 ) ) ;
#1844 = CIRCLE ( 'NONE', #18607, 0.1250000000000001110 ) ;
#1845 = AXIS2_PLACEMENT_3D ( 'NONE', #30690, #5572, #3263 ) ;
#1846 = ORIENTED_EDGE ( 'NONE', *, *, #12585, .F. ) ;
#1847 = CARTESIAN_POINT ( 'NONE',  ( 46.27402357847488901, 23.03451764446789696, 46.16421949815220671 ) ) ;
#1848 = VECTOR ( 'NONE', #1885, 1000.000000000000000 ) ;
#1849 = CIRCLE ( 'NONE', #5001, 0.1250000000000001110 ) ;
#1850 = CARTESIAN_POINT ( 'NONE',  ( 49.76180767062073329, 24.76486642951281425, 48.77751362531137147 ) ) ;
#1851 = EDGE_CURVE ( 'NONE', #25423, #22382, #26024, .T. ) ;
#1852 = DIRECTION ( 'NONE',  ( 0.000000000000000000, 0.000000000000000000, -1.000000000000000000 ) ) ;
#1853 = AXIS2_PLACEMENT_3D ( 'NONE', #9106, #4179, #24201 ) ;
#1854 = MANIFOLD_SOLID_BREP ( 'Stock-MAT-060-1', #25227 ) ;
#1855 = CARTESIAN_POINT ( 'NONE',  ( -36.76418579970419387, 10.14130568307076352, 57.04930799450051637 ) ) ;
#1856 = ORIENTED_EDGE ( 'NONE', *, *, #8300, .T. ) ;
#1857 = CARTESIAN_POINT ( 'NONE',  ( -39.56017130034231144, -5.935730392421668888, 77.88797225724067630 ) ) ;
#1858 = DIRECTION ( 'NONE',  ( -0.9612616959383200044, -0.2756373558169954996, 1.660411357259285896E-16 ) ) ;
#1859 = CARTESIAN_POINT ( 'NONE',  ( 80.71684048725118998, -5.935454207752202116, 16.07118271501079221 ) ) ;
#1860 = EDGE_LOOP ( 'NONE', ( #4335, #9255, #17864, #29112 ) ) ;
#1861 = EDGE_LOOP ( 'NONE', ( #29758, #1487, #31150, #31943 ) ) ;
#1862 = DIRECTION ( 'NONE',  ( 0.8746197071393926326, -0.4848096202463430537, -8.676864087101709653E-18 ) ) ;
#1863 = DIRECTION ( 'NONE',  ( 0.8907924397839087627, 1.100109291107993941E-16, -0.4544104193609906361 ) ) ;
#1864 = CARTESIAN_POINT ( 'NONE',  ( 21.09785597605719332, 25.56454579224779877, 70.54930799450050927 ) ) ;
#1865 = CARTESIAN_POINT ( 'NONE',  ( -42.66751614955960292, 15.14923148629343430, 38.44930799450052206 ) ) ;
#1866 = ORIENTED_EDGE ( 'NONE', *, *, #20239, .T. ) ;
#1867 = DIRECTION ( 'NONE',  ( 0.000000000000000000, 0.000000000000000000, 1.000000000000000000 ) ) ;
#1868 = ORIENTED_EDGE ( 'NONE', *, *, #12433, .F. ) ;
#1869 = ORIENTED_EDGE ( 'NONE', *, *, #28980, .T. ) ;
#1870 = DIRECTION ( 'NONE',  ( -1.101824276508909887E-16, 1.000000000000000000, -0.000000000000000000 ) ) ;
#1871 = CIRCLE ( 'NONE', #823, 1.300000000000002487 ) ;
#1872 = CIRCLE ( 'NONE', #30188, 1.003191532947552256 ) ;
#1873 = ORIENTED_EDGE ( 'NONE', *, *, #18457, .T. ) ;
#1874 = CARTESIAN_POINT ( 'NONE',  ( 21.09992658989239089, 24.71183152705960140, 47.04930799450051637 ) ) ;
#1875 = DIRECTION ( 'NONE',  ( -1.224646799147353207E-16, 0.000000000000000000, -1.000000000000000000 ) ) ;
#1876 = DIRECTION ( 'NONE',  ( -0.2530443915477144645, 0.8824706660164548522, 0.3965022818682404915 ) ) ;
#1877 = AXIS2_PLACEMENT_3D ( 'NONE', #16713, #9184, #26743 ) ;
#1878 = VERTEX_POINT ( 'NONE', #8638 ) ;
#1879 = DIRECTION ( 'NONE',  ( 0.9612616959383221138, 0.2756373558169876170, 0.000000000000000000 ) ) ;
#1880 = VERTEX_POINT ( 'NONE', #21406 ) ;
#1881 = CARTESIAN_POINT ( 'NONE',  ( 21.09992658989239089, 26.71664230456639899, 47.04930799450051637 ) ) ;
#1882 = CARTESIAN_POINT ( 'NONE',  ( 48.59475124299144966, 29.58954579224780090, 45.61232171765963272 ) ) ;
#1883 = CARTESIAN_POINT ( 'NONE',  ( -40.66881382964710667, 6.810455744988438198, 39.49839327164657732 ) ) ;
#1884 = VERTEX_POINT ( 'NONE', #9113 ) ;
#1885 = DIRECTION ( 'NONE',  ( -1.101824276508909887E-16, 1.000000000000000000, -0.000000000000000000 ) ) ;
#1886 = CARTESIAN_POINT ( 'NONE',  ( 8.732853799281732776, 27.47145308207318237, 47.04930799450051637 ) ) ;
#1887 = FACE_OUTER_BOUND ( 'NONE', #17720, .T. ) ;
#1888 = ADVANCED_FACE ( 'NONE', ( #14373 ), #14045, .F. ) ;
#1889 = DIRECTION ( 'NONE',  ( 0.2756373558169954441, -0.9612616959383198934, 1.479773560108263451E-16 ) ) ;
#1890 = CARTESIAN_POINT ( 'NONE',  ( -40.16503835899720087, 7.510440877657817538, 35.29832907986742185 ) ) ;
#1891 = EDGE_CURVE ( 'NONE', #26545, #19851, #18412, .T. ) ;
#1892 = FACE_OUTER_BOUND ( 'NONE', #30186, .T. ) ;
#1893 = ADVANCED_FACE ( 'NONE', ( #9279 ), #83, .T. ) ;
#1894 = VERTEX_POINT ( 'NONE', #21900 ) ;
#1895 = CARTESIAN_POINT ( 'NONE',  ( -40.23847961986563604, 6.935107571023904960, 34.63435542749680707 ) ) ;
#1896 = DIRECTION ( 'NONE',  ( -1.101824276508909887E-16, 1.000000000000000000, -0.000000000000000000 ) ) ;
#1897 = EDGE_LOOP ( 'NONE', ( #19194, #19505 ) ) ;
#1898 = DIRECTION ( 'NONE',  ( -0.8746197071393858602, 0.4848096202463547666, 0.000000000000000000 ) ) ;
#1899 = VECTOR ( 'NONE', #10554, 1000.000000000000114 ) ;
#1900 = MECHANICAL_DESIGN_GEOMETRIC_PRESENTATION_REPRESENTATION (  '', ( #11858 ), #30216 ) ;
#1901 = DIRECTION ( 'NONE',  ( -1.101824276508909887E-16, 1.000000000000000000, -0.000000000000000000 ) ) ;
#1902 = ORIENTED_EDGE ( 'NONE', *, *, #24442, .T. ) ;
#1903 = ORIENTED_EDGE ( 'NONE', *, *, #12814, .T. ) ;
#1904 = AXIS2_PLACEMENT_3D ( 'NONE', #31595, #14029, #11568 ) ;
#1905 = VERTEX_POINT ( 'NONE', #29472 ) ;
#1906 = PLANE ( 'NONE',  #19818 ) ;
#1907 = AXIS2_PLACEMENT_3D ( 'NONE', #28226, #27904, #5419 ) ;
#1908 = ORIENTED_EDGE ( 'NONE', *, *, #6557, .F. ) ;
#1909 = ORIENTED_EDGE ( 'NONE', *, *, #24067, .T. ) ;
#1910 = DIRECTION ( 'NONE',  ( -1.000000000000000000, 0.000000000000000000, 0.000000000000000000 ) ) ;
#1911 = CARTESIAN_POINT ( 'NONE',  ( 47.25101359556892078, 23.12036939723557083, 46.81322240026007364 ) ) ;
#1912 = CARTESIAN_POINT ( 'NONE',  ( 21.09785597605719332, 25.56454579224779877, 47.04930799450051637 ) ) ;
#1913 = PLANE ( 'NONE',  #3302 ) ;
#1914 = CARTESIAN_POINT ( 'NONE',  ( 44.74832014356462651, 28.42786309983298310, 46.92728461490987257 ) ) ;
#1915 = ORIENTED_EDGE ( 'NONE', *, *, #16110, .T. ) ;
#1916 = CARTESIAN_POINT ( 'NONE',  ( 1.883339950622007652, 7.264443105416139801, 47.04930799450051637 ) ) ;
#1917 = ORIENTED_EDGE ( 'NONE', *, *, #28279, .F. ) ;
#1918 = CARTESIAN_POINT ( 'NONE',  ( -11.49897738644833645, -5.264348929021194223, -9.633576251181647621 ) ) ;
#1919 = EDGE_LOOP ( 'NONE', ( #1575, #9249, #30657, #15820 ) ) ;
#1920 = CARTESIAN_POINT ( 'NONE',  ( 81.79971628361815306, -5.937448199248381187, 77.92687966219790496 ) ) ;
#1921 = DIRECTION ( 'NONE',  ( -1.101824276508909887E-16, 1.000000000000000000, -0.000000000000000000 ) ) ;
#1922 = AXIS2_PLACEMENT_3D ( 'NONE', #20265, #2460, #29877 ) ;
#1923 = DIRECTION ( 'NONE',  ( -1.000000000000000000, 0.000000000000000000, 0.000000000000000000 ) ) ;
#1924 = CARTESIAN_POINT ( 'NONE',  ( 21.09785597605719332, -8.535454207752287914, 47.04930799450051637 ) ) ;
#1925 = DIRECTION ( 'NONE',  ( -0.4848096202463645921, -0.8746197071393805311, 0.000000000000000000 ) ) ;
#1926 = EDGE_CURVE ( 'NONE', #18455, #2485, #10046, .T. ) ;
#1927 = EDGE_CURVE ( 'NONE', #2146, #30019, #20527, .T. ) ;
#1928 = CARTESIAN_POINT ( 'NONE',  ( 45.24946171279598417, 29.82124452788248092, 47.99220971130007030 ) ) ;
#1929 = EDGE_CURVE ( 'NONE', #26389, #3234, #9006, .T. ) ;
#1930 = CARTESIAN_POINT ( 'NONE',  ( 46.17891025898683921, 22.93807716476589675, 48.46582155994513386 ) ) ;
#1931 = CARTESIAN_POINT ( 'NONE',  ( 21.09785597605719332, -5.935454207752083988, 47.04930799449963530 ) ) ;
#1932 = EDGE_CURVE ( 'NONE', #24691, #28859, #24532, .T. ) ;
#1933 = ORIENTED_EDGE ( 'NONE', *, *, #22375, .F. ) ;
#1934 = CARTESIAN_POINT ( 'NONE',  ( 41.51205063648687599, 11.92558985988973497, -37.95069200549950494 ) ) ;
#1935 = DIRECTION ( 'NONE',  ( 0.9275012328650846793, -0.3738200944756017163, -1.135861416033449914E-16 ) ) ;
#1936 = CARTESIAN_POINT ( 'NONE',  ( -36.59542768321662720, 12.56771722797891400, 37.04930799450052348 ) ) ;
#1937 = CARTESIAN_POINT ( 'NONE',  ( 48.28750925852675380, 22.93328494799376571, 45.80964605384927069 ) ) ;
#1938 = CARTESIAN_POINT ( 'NONE',  ( -29.27337757263006424, 2.267350949466874432, 14.79705809024468088 ) ) ;
#1939 = EDGE_LOOP ( 'NONE', ( #1484, #32183, #18857, #25866, #22142, #10442 ) ) ;
#1940 = VERTEX_POINT ( 'NONE', #6494 ) ;
#1941 = DIRECTION ( 'NONE',  ( -1.000000000000000000, 0.000000000000000000, 0.000000000000000000 ) ) ;
#1942 = CARTESIAN_POINT ( 'NONE',  ( 21.09785597605720042, -13.98292989133646103, 47.04930799450051637 ) ) ;
#1943 = AXIS2_PLACEMENT_3D ( 'NONE', #31975, #9495, #19493 ) ;
#1944 = ORIENTED_EDGE ( 'NONE', *, *, #2599, .T. ) ;
#1945 = APPLICATION_CONTEXT ( 'automotive_design' ) ;
#1946 = EDGE_LOOP ( 'NONE', ( #12322, #14844, #6465, #22478 ) ) ;
#1947 = CARTESIAN_POINT ( 'NONE',  ( 33.72499318558949710, 30.84184655352422411, 47.04930799450051637 ) ) ;
#1948 = ADVANCED_FACE ( 'NONE', ( #24212 ), #8785, .T. ) ;
#1949 = CARTESIAN_POINT ( 'NONE',  ( 21.09992658989239089, 27.72145308207318237, 47.04930799450051637 ) ) ;
#1950 = DIRECTION ( 'NONE',  ( 0.000000000000000000, 0.000000000000000000, -1.000000000000000000 ) ) ;
#1951 = EDGE_CURVE ( 'NONE', #5630, #5136, #14433, .T. ) ;
#1952 = ORIENTED_EDGE ( 'NONE', *, *, #11352, .T. ) ;
#1953 = VECTOR ( 'NONE', #28095, 999.9999999999998863 ) ;
#1954 = CARTESIAN_POINT ( 'NONE',  ( 8.474859994195282908, 38.56284415653841791, 47.04930799450051637 ) ) ;
#1955 = CIRCLE ( 'NONE', #21866, 12.36707279061065101 ) ;
#1956 = DIRECTION ( 'NONE',  ( 0.000000000000000000, -0.000000000000000000, -1.000000000000000000 ) ) ;
#1957 = CARTESIAN_POINT ( 'NONE',  ( 75.25323102592015800, -0.6709275202869922072, 13.62290469009603022 ) ) ;
#1958 = VERTEX_POINT ( 'NONE', #4188 ) ;
#1959 = AXIS2_PLACEMENT_3D ( 'NONE', #7931, #27946, #15149 ) ;
#1960 = VERTEX_POINT ( 'NONE', #8952 ) ;
#1961 = AXIS2_PLACEMENT_3D ( 'NONE', #13939, #11633, #11953 ) ;
#1962 = ORIENTED_EDGE ( 'NONE', *, *, #4009, .T. ) ;
#1963 = DIRECTION ( 'NONE',  ( 1.000000000000000000, 0.000000000000000000, 0.000000000000000000 ) ) ;
#1964 = DIRECTION ( 'NONE',  ( -1.101824276508909887E-16, 1.000000000000000000, -0.000000000000000000 ) ) ;
#1965 = DIRECTION ( 'NONE',  ( 0.000000000000000000, 0.000000000000000000, -1.000000000000000000 ) ) ;
#1966 = TOROIDAL_SURFACE ( 'NONE', #22937, 12.61792373059890693, 0.1250000000000019429 ) ;
#1967 = DIRECTION ( 'NONE',  ( -1.101824276508909887E-16, 1.000000000000000000, -0.000000000000000000 ) ) ;
#1968 = EDGE_CURVE ( 'NONE', #4559, #29013, #12874, .T. ) ;
#1969 = DIRECTION ( 'NONE',  ( 1.000000000000000000, 0.000000000000000000, 0.000000000000000000 ) ) ;
#1970 = ORIENTED_EDGE ( 'NONE', *, *, #13537, .F. ) ;
#1971 = ORIENTED_EDGE ( 'NONE', *, *, #4751, .T. ) ;
#1972 = DIRECTION ( 'NONE',  ( -1.000000000000000000, 0.000000000000000000, 0.000000000000000000 ) ) ;
#1973 = CARTESIAN_POINT ( 'NONE',  ( -40.90015969217747482, 8.955334253785164123, 57.04930799450051637 ) ) ;
#1974 = LINE ( 'NONE', #9699, #15157 ) ;
#1975 = ORIENTED_EDGE ( 'NONE', *, *, #7569, .F. ) ;
#1976 = CARTESIAN_POINT ( 'NONE',  ( -6.242780362964605700, 9.162376348828958683, -4.318210402824582239 ) ) ;
#1977 = CARTESIAN_POINT ( 'NONE',  ( 39.85850837550807313, -13.74047052604243824, 102.2994869940680616 ) ) ;
#1978 = ORIENTED_EDGE ( 'NONE', *, *, #18415, .F. ) ;
#1979 = DIRECTION ( 'NONE',  ( -1.101824276508909887E-16, 1.000000000000000000, -0.000000000000000000 ) ) ;
#1980 = DIRECTION ( 'NONE',  ( -1.101824276508909887E-16, 1.000000000000000000, -0.000000000000000000 ) ) ;
#1981 = DIRECTION ( 'NONE',  ( -1.101824276508909887E-16, 1.000000000000000000, -0.000000000000000000 ) ) ;
#1982 = ADVANCED_FACE ( 'NONE', ( #11582 ), #9775, .F. ) ;
#1983 = CIRCLE ( 'NONE', #27669, 0.1000000000000006301 ) ;
#1984 = CIRCLE ( 'NONE', #9326, 12.36707279061065279 ) ;
#1985 = EDGE_CURVE ( 'NONE', #6454, #6391, #27880, .T. ) ;
#1986 = ORIENTED_EDGE ( 'NONE', *, *, #27426, .F. ) ;
#1987 = AXIS2_PLACEMENT_3D ( 'NONE', #8912, #6617, #21212 ) ;
#1988 = VECTOR ( 'NONE', #29349, 1000.000000000000114 ) ;
#1989 = DIRECTION ( 'NONE',  ( -1.000000000000000000, 0.000000000000000000, 0.000000000000000000 ) ) ;
#1990 = CARTESIAN_POINT ( 'NONE',  ( -43.86882709718853590, -0.1754741395363378920, 32.14930799450051779 ) ) ;
#1991 = EDGE_CURVE ( 'NONE', #17686, #12130, #16391, .T. ) ;
#1992 = CARTESIAN_POINT ( 'NONE',  ( 48.16694854572211426, 25.86119643316632022, 49.14507740233662503 ) ) ;
#1993 = EDGE_CURVE ( 'NONE', #12799, #21428, #12734, .T. ) ;
#1994 = CIRCLE ( 'NONE', #8809, 0.1000000000000028644 ) ;
#1995 = ORIENTED_EDGE ( 'NONE', *, *, #15821, .T. ) ;
#1996 = ADVANCED_FACE ( 'NONE', ( #2860 ), #9931, .T. ) ;
#1997 = CARTESIAN_POINT ( 'NONE',  ( 33.71785032049099584, 30.96664230456641675, 47.04930799450051637 ) ) ;
#1998 = CARTESIAN_POINT ( 'NONE',  ( -43.69495677161796010, 1.169528900831203311, 60.44930799450051495 ) ) ;
#1999 = CARTESIAN_POINT ( 'NONE',  ( 53.71827270862435455, -5.211355130743560160, -9.585364147679955593 ) ) ;
#2000 = CARTESIAN_POINT ( 'NONE',  ( 21.09992658989238734, 32.59164230456639899, 47.04930799450051637 ) ) ;
#2001 = CARTESIAN_POINT ( 'NONE',  ( 8.698509210239571132, 30.34164230456639544, 47.04930799450051637 ) ) ;
#2002 = CARTESIAN_POINT ( 'NONE',  ( -43.68921302925062378, 1.179890886355840163, 39.54930799450052348 ) ) ;
#2003 = DIRECTION ( 'NONE',  ( -0.000000000000000000, -1.000000000000000000, 0.000000000000000000 ) ) ;
#2004 = FACE_OUTER_BOUND ( 'NONE', #10096, .T. ) ;
#2005 = SURFACE_SIDE_STYLE ('',( #27280 ) ) ;
#2006 = EDGE_CURVE ( 'NONE', #16515, #15368, #32070, .T. ) ;
#2007 = VERTEX_POINT ( 'NONE', #27650 ) ;
#2008 = FACE_OUTER_BOUND ( 'NONE', #5670, .T. ) ;
#2009 = AXIS2_PLACEMENT_3D ( 'NONE', #9915, #29946, #12718 ) ;
#2010 = AXIS2_PLACEMENT_3D ( 'NONE', #11975, #7046, #4265 ) ;
#2011 = CARTESIAN_POINT ( 'NONE',  ( -40.41702379479729501, 8.543002789739318814, 34.55838508629864947 ) ) ;
#2012 = DIRECTION ( 'NONE',  ( -0.000000000000000000, -1.000000000000000000, 0.000000000000000000 ) ) ;
#2013 = VECTOR ( 'NONE', #10033, 1000.000000000000000 ) ;
#2014 = CARTESIAN_POINT ( 'NONE',  ( 52.81327818505165794, -5.811083640285383822, 104.5757368101217679 ) ) ;
#2015 = ORIENTED_EDGE ( 'NONE', *, *, #27426, .T. ) ;
#2016 = CYLINDRICAL_SURFACE ( 'NONE', #12424, 7.999999999999999112 ) ;
#2017 = DIRECTION ( 'NONE',  ( 0.4848096202463484938, 0.8746197071393896350, -2.220446049250314067E-16 ) ) ;
#2018 = FACE_OUTER_BOUND ( 'NONE', #29941, .T. ) ;
#2019 = AXIS2_PLACEMENT_3D ( 'NONE', #9128, #1247, #29308 ) ;
#2020 = ORIENTED_EDGE ( 'NONE', *, *, #7856, .F. ) ;
#2021 = VERTEX_POINT ( 'NONE', #24868 ) ;
#2022 = DIRECTION ( 'NONE',  ( 0.000000000000000000, 0.000000000000000000, -1.000000000000000000 ) ) ;
#2023 = LINE ( 'NONE', #24338, #21436 ) ;
#2024 = CARTESIAN_POINT ( 'NONE',  ( -39.58809650894544774, 2.596771453999702661, 47.04930799450051637 ) ) ;
#2025 = AXIS2_PLACEMENT_3D ( 'NONE', #31213, #23969, #11345 ) ;
#2026 = DIRECTION ( 'NONE',  ( -1.000000000000000000, -1.101824276508909887E-16, 0.000000000000000000 ) ) ;
#2027 = VERTEX_POINT ( 'NONE', #9607 ) ;
#2028 = CARTESIAN_POINT ( 'NONE',  ( 72.31638179958355295, 11.69718155787697356, 24.43823011782819776 ) ) ;
#2029 = ORIENTED_EDGE ( 'NONE', *, *, #14198, .F. ) ;
#2030 = ADVANCED_FACE ( 'NONE', ( #10267 ), #15024, .T. ) ;
#2031 = EDGE_CURVE ( 'NONE', #28434, #15217, #25759, .T. ) ;
#2032 = ORIENTED_EDGE ( 'NONE', *, *, #25394, .F. ) ;
#2033 = DIRECTION ( 'NONE',  ( -0.2756373558169947779, 0.9612616959383200044, 0.000000000000000000 ) ) ;
#2034 = EDGE_CURVE ( 'NONE', #8765, #30210, #25027, .T. ) ;
#2035 = EDGE_LOOP ( 'NONE', ( #28490, #17099, #19281, #32413 ) ) ;
#2036 = ADVANCED_FACE ( 'NONE', ( #29634 ), #2387, .F. ) ;
#2037 = AXIS2_PLACEMENT_3D ( 'NONE', #3, #2629, #15747 ) ;
#2038 = CARTESIAN_POINT ( 'NONE',  ( 45.96182992765471909, 27.17822092656774657, 44.82232689504102296 ) ) ;
#2039 = CARTESIAN_POINT ( 'NONE',  ( -30.66701073789274901, 11.92468888572869723, 68.04721722412880069 ) ) ;
#2040 = CARTESIAN_POINT ( 'NONE',  ( -29.27613032885505007, -5.935454207752198563, 77.87546120947918382 ) ) ;
#2041 = VERTEX_POINT ( 'NONE', #17475 ) ;
#2042 = CIRCLE ( 'NONE', #6239, 0.1250000000000001110 ) ;
#2043 = CARTESIAN_POINT ( 'NONE',  ( 51.92400919103563695, -5.935454207752202116, -13.39445452378610568 ) ) ;
#2044 = ORIENTED_EDGE ( 'NONE', *, *, #26227, .F. ) ;
#2045 = CARTESIAN_POINT ( 'NONE',  ( 34.09963999142011204, 15.70210863493540288, 47.04930799450052348 ) ) ;
#2046 = DIRECTION ( 'NONE',  ( -0.000000000000000000, -1.000000000000000000, -0.000000000000000000 ) ) ;
#2047 = CARTESIAN_POINT ( 'NONE',  ( 71.61810346057937693, 10.40257568944042710, 72.79952121014760280 ) ) ;
#2048 = ORIENTED_EDGE ( 'NONE', *, *, #29916, .F. ) ;
#2049 = CARTESIAN_POINT ( 'NONE',  ( 21.09992658989239089, 25.09164230456639899, 47.04930799450051637 ) ) ;
#2050 = CYLINDRICAL_SURFACE ( 'NONE', #4327, 12.36707279061065101 ) ;
#2051 = CARTESIAN_POINT ( 'NONE',  ( -41.04685960816998147, 9.497330455345890599, 38.54930799450052348 ) ) ;
#2052 = DIRECTION ( 'NONE',  ( -0.9097384655268497822, -0.4151817967359032191, -2.820562191637069417E-18 ) ) ;
#2053 = CARTESIAN_POINT ( 'NONE',  ( 21.09785597605720753, 14.86454579224779948, 47.04930799450052348 ) ) ;
#2054 = DIRECTION ( 'NONE',  ( -0.000000000000000000, 0.000000000000000000, 1.000000000000000000 ) ) ;
#2055 = DIRECTION ( 'NONE',  ( -0.000000000000000000, -1.000000000000000000, 0.000000000000000000 ) ) ;
#2056 = ORIENTED_EDGE ( 'NONE', *, *, #22974, .T. ) ;
#2057 = DIRECTION ( 'NONE',  ( -1.000000000000000000, 0.000000000000000000, 0.000000000000000000 ) ) ;
#2058 = DIRECTION ( 'NONE',  ( -1.000000000000000000, 0.000000000000000000, 0.000000000000000000 ) ) ;
#2059 = ORIENTED_EDGE ( 'NONE', *, *, #18153, .T. ) ;
#2060 = DIRECTION ( 'NONE',  ( 0.000000000000000000, 1.000000000000000000, -0.000000000000000000 ) ) ;
#2061 = CIRCLE ( 'NONE', #20397, 27.49999999999999645 ) ;
#2062 = CIRCLE ( 'NONE', #31939, 12.62506659569710266 ) ;
#2063 = PLANE ( 'NONE',  #31594 ) ;
#2064 = VERTEX_POINT ( 'NONE', #12404 ) ;
#2065 = ORIENTED_EDGE ( 'NONE', *, *, #19663, .T. ) ;
#2066 = AXIS2_PLACEMENT_3D ( 'NONE', #1530, #9418, #26972 ) ;
#2067 = ORIENTED_EDGE ( 'NONE', *, *, #49, .F. ) ;
#2068 = AXIS2_PLACEMENT_3D ( 'NONE', #7531, #10318, #15399 ) ;
#2069 = AXIS2_PLACEMENT_3D ( 'NONE', #26157, #11550, #15989 ) ;
#2070 = ADVANCED_FACE ( 'NONE', ( #27494 ), #29966, .T. ) ;
#2071 = ADVANCED_FACE ( 'NONE', ( #24704 ), #30126, .T. ) ;
#2072 = EDGE_CURVE ( 'NONE', #12553, #7860, #31016, .T. ) ;
#2073 = CARTESIAN_POINT ( 'NONE',  ( 21.09785597605719332, 16.86454579224779948, 47.04930799450051637 ) ) ;
#2074 = AXIS2_PLACEMENT_3D ( 'NONE', #27150, #7137, #7301 ) ;
#2075 = ORIENTED_EDGE ( 'NONE', *, *, #32083, .T. ) ;
#2076 = EDGE_LOOP ( 'NONE', ( #17495, #22198, #1962, #16896 ) ) ;
#2077 = CARTESIAN_POINT ( 'NONE',  ( -40.13606231985500017, 7.635531802539802015, 60.54930799450051637 ) ) ;
#2078 = DIRECTION ( 'NONE',  ( -1.000000000000000000, 0.000000000000000000, 0.000000000000000000 ) ) ;
#2079 = DIRECTION ( 'NONE',  ( -1.000000000000000000, 0.000000000000000000, 0.000000000000000000 ) ) ;
#2080 = CARTESIAN_POINT ( 'NONE',  ( 21.09992658989239089, 23.71183152705959429, 47.04930799450051637 ) ) ;
#2081 = CARTESIAN_POINT ( 'NONE',  ( -36.21250238186772208, 8.895094119121829124, 53.80788663826320573 ) ) ;
#2082 = EDGE_LOOP ( 'NONE', ( #15005, #21265, #17984, #14405 ) ) ;
#2083 = CARTESIAN_POINT ( 'NONE',  ( 21.09785597605719332, -6.314304012688826795, -18.91914050022838012 ) ) ;
#2084 = ORIENTED_EDGE ( 'NONE', *, *, #28084, .T. ) ;
#2085 = CARTESIAN_POINT ( 'NONE',  ( -12.50119137592388441, -1.331120222581884560, -6.486951009445048655 ) ) ;
#2086 = VERTEX_POINT ( 'NONE', #727 ) ;
#2087 = DIRECTION ( 'NONE',  ( 0.9612616959383127879, 0.2756373558170205351, 1.210030619774134952E-14 ) ) ;
#2088 = DIRECTION ( 'NONE',  ( -1.224646799147353207E-16, 0.000000000000000000, -1.000000000000000000 ) ) ;
#2089 = TOROIDAL_SURFACE ( 'NONE', #19894, 12.40141737965280022, 0.1249999999999992228 ) ;
#2090 = TOROIDAL_SURFACE ( 'NONE', #31989, 12.61792373059896200, 0.1249999999999979183 ) ;
#2091 = CARTESIAN_POINT ( 'NONE',  ( 48.86248627303584158, 22.86454579224779948, 46.10725065118596433 ) ) ;
#2092 = DIRECTION ( 'NONE',  ( 0.8746197071393925215, -0.4848096202463429982, -8.676864087101708112E-18 ) ) ;
#2093 = CARTESIAN_POINT ( 'NONE',  ( 33.46699938050304013, 25.22145308207319303, 47.04930799450050927 ) ) ;
#2094 = CARTESIAN_POINT ( 'NONE',  ( 44.77625694075215534, 25.31454579807171257, 48.23360063142255427 ) ) ;
#2095 = DIRECTION ( 'NONE',  ( 0.000000000000000000, 0.000000000000000000, -1.000000000000000000 ) ) ;
#2096 = DIRECTION ( 'NONE',  ( -1.000000000000000000, 0.000000000000000000, 0.000000000000000000 ) ) ;
#2097 = ORIENTED_EDGE ( 'NONE', *, *, #6002, .F. ) ;
#2098 = CIRCLE ( 'NONE', #24716, 0.1000000000000014905 ) ;
#2099 = DIRECTION ( 'NONE',  ( 0.2756373558170082672, -0.9612616959383162296, 0.000000000000000000 ) ) ;
#2100 = AXIS2_PLACEMENT_3D ( 'NONE', #6138, #1696, #11716 ) ;
#2101 = DIRECTION ( 'NONE',  ( -1.101824276508909887E-16, 1.000000000000000000, -0.000000000000000000 ) ) ;
#2102 = LINE ( 'NONE', #14423, #15595 ) ;
#2103 = CARTESIAN_POINT ( 'NONE',  ( 48.61853364894580665, 22.95310733321322161, 46.43464276236652921 ) ) ;
#2104 = CARTESIAN_POINT ( 'NONE',  ( -29.27337757263006424, 11.92558985988973497, 26.63511333407100778 ) ) ;
#2105 = ORIENTED_EDGE ( 'NONE', *, *, #26289, .F. ) ;
#2106 = ORIENTED_EDGE ( 'NONE', *, *, #1295, .F. ) ;
#2107 = CARTESIAN_POINT ( 'NONE',  ( 21.09992658989238734, 31.09164230456639544, 47.04930799450051637 ) ) ;
#2108 = CIRCLE ( 'NONE', #27820, 12.52641737965288904 ) ;
#2109 = ORIENTED_EDGE ( 'NONE', *, *, #21254, .T. ) ;
#2110 = EDGE_CURVE ( 'NONE', #3554, #1319, #4271, .T. ) ;
#2111 = AXIS2_PLACEMENT_3D ( 'NONE', #4236, #18822, #16688 ) ;
#2112 = TOROIDAL_SURFACE ( 'NONE', #7373, 13.30178401536290878, 0.2000000000000002609 ) ;
#2113 = EDGE_CURVE ( 'NONE', #11449, #13013, #22617, .T. ) ;
#2114 = ADVANCED_FACE ( 'NONE', ( #560 ), #23211, .F. ) ;
#2115 = EDGE_CURVE ( 'NONE', #25631, #5457, #8469, .T. ) ;
#2116 = TOROIDAL_SURFACE ( 'NONE', #10523, 1.524998423334081643, 0.1000000000000000056 ) ;
#2117 = ORIENTED_EDGE ( 'NONE', *, *, #14572, .T. ) ;
#2118 = EDGE_CURVE ( 'NONE', #31159, #14982, #10591, .T. ) ;
#2119 = EDGE_CURVE ( 'NONE', #14676, #16515, #11127, .T. ) ;
#2120 = CIRCLE ( 'NONE', #12091, 12.08499999999999908 ) ;
#2121 = DIRECTION ( 'NONE',  ( -0.000000000000000000, -1.000000000000000000, -0.000000000000000000 ) ) ;
#2122 = TOROIDAL_SURFACE ( 'NONE', #18854, 12.40141737965281621, 0.1250000000000009159 ) ;
#2123 = AXIS2_PLACEMENT_3D ( 'NONE', #10950, #5539, #28660 ) ;
#2124 = VERTEX_POINT ( 'NONE', #18588 ) ;
#2125 = DIRECTION ( 'NONE',  ( 1.234978253042719660E-16, -1.000000000000000000, -1.109335647967047851E-31 ) ) ;
#2126 = CARTESIAN_POINT ( 'NONE',  ( 45.45050395073641170, 20.53597436367637030, 46.96375251515745930 ) ) ;
#2127 = DIRECTION ( 'NONE',  ( 0.000000000000000000, 3.754529891495955404E-16, -1.000000000000000000 ) ) ;
#2128 = EDGE_LOOP ( 'NONE', ( #25205, #31539, #7322, #24885 ) ) ;
#2129 = ORIENTED_EDGE ( 'NONE', *, *, #16040, .F. ) ;
#2130 = B_SPLINE_CURVE_WITH_KNOTS ( 'NONE', 3,
 ( #29565, #16909, #16580, #14301, #31697, #16739, #9209, #27088, #28917, #26765, #26929, #11503, #4284, #13979, #31855, #24302, #19200, #21499, #21673, #11838, #1819, #29396, #4445, #9370, #24627, #19533, #1654, #19366, #14467, #19039, #14623, #2147, #24461, #1976, #14138, #16425 ),
 .UNSPECIFIED., .F., .F.,
 ( 4, 2, 2, 2, 2, 2, 2, 2, 2, 2, 2, 2, 2, 2, 2, 2, 2, 4 ),
 ( 2.602085213965210642E-18, 0.001253900128824282905, 0.001880850193236422189, 0.002507800257648561473, 0.003134750322060700974, 0.003761700386472840475, 0.005015600515297116008, 0.005642550579709253340, 0.006269500644121390673, 0.007523400772945662736, 0.008777300901769934799, 0.01003120103059420773, 0.01253900128824275012, 0.01504680154589129598, 0.01630070167471556544, 0.01755460180353983837, 0.01880850193236410783, 0.02006240206118838076 ),
 .UNSPECIFIED. ) ;
#2131 = LINE ( 'NONE', #11662, #2854 ) ;
#2132 = CIRCLE ( 'NONE', #31519, 1.042135311067126979 ) ;
#2133 = VERTEX_POINT ( 'NONE', #20742 ) ;
#2134 = CARTESIAN_POINT ( 'NONE',  ( -40.49360782792987123, 7.147293204394357780, 35.15590551817737008 ) ) ;
#2135 = FACE_OUTER_BOUND ( 'NONE', #26216, .T. ) ;
#2136 = DIRECTION ( 'NONE',  ( 0.000000000000000000, 1.000000000000000000, 0.000000000000000000 ) ) ;
#2137 = LINE ( 'NONE', #17223, #18878 ) ;
#2138 = CARTESIAN_POINT ( 'NONE',  ( 48.83862994770794330, 27.95457786121581734, 48.17861352429476796 ) ) ;
#2139 = CARTESIAN_POINT ( 'NONE',  ( 0.000000000000000000, 0.000000000000000000, 0.000000000000000000 ) ) ;
#2140 = ORIENTED_EDGE ( 'NONE', *, *, #22896, .T. ) ;
#2141 = ORIENTED_EDGE ( 'NONE', *, *, #29004, .F. ) ;
#2142 = CARTESIAN_POINT ( 'NONE',  ( 21.09785597605720753, 17.16467605102632632, 47.04930799450052348 ) ) ;
#2143 = DIRECTION ( 'NONE',  ( 0.000000000000000000, 0.000000000000000000, -1.000000000000000000 ) ) ;
#2144 = AXIS2_PLACEMENT_3D ( 'NONE', #28347, #8003, #23255 ) ;
#2145 = CARTESIAN_POINT ( 'NONE',  ( 8.474859994195282908, 38.56284415653841791, 47.04930799450051637 ) ) ;
#2146 = VERTEX_POINT ( 'NONE', #28616 ) ;
#2147 = CARTESIAN_POINT ( 'NONE',  ( -7.125208762201825863, 8.281585831149227417, -4.396110345893636584 ) ) ;
#2148 = CIRCLE ( 'NONE', #28885, 0.1000000000000006301 ) ;
#2149 = CARTESIAN_POINT ( 'NONE',  ( 8.732853799281738105, 25.71183152705960140, 47.04930799450051637 ) ) ;
#2150 = AXIS2_PLACEMENT_3D ( 'NONE', #346, #4958, #2966 ) ;
#2151 = ORIENTED_EDGE ( 'NONE', *, *, #17153, .F. ) ;
#2152 = CARTESIAN_POINT ( 'NONE',  ( 21.09785597605719332, 25.56454579224779877, 73.04930799450052348 ) ) ;
#2153 = AXIS2_PLACEMENT_3D ( 'NONE', #11898, #18942, #21895 ) ;
#2154 = CARTESIAN_POINT ( 'NONE',  ( 49.28428300279882990, 26.24787913140504614, 48.46772541801551171 ) ) ;
#2155 = EDGE_CURVE ( 'NONE', #30753, #31841, #26830, .T. ) ;
#2156 = AXIS2_PLACEMENT_3D ( 'NONE', #13055, #17960, #18436 ) ;
#2157 = DIRECTION ( 'NONE',  ( 0.000000000000000000, -0.000000000000000000, -1.000000000000000000 ) ) ;
#2158 = AXIS2_PLACEMENT_3D ( 'NONE', #22995, #5122, #12845 ) ;
#2159 = EDGE_LOOP ( 'NONE', ( #14206, #9203, #31203, #26392 ) ) ;
#2160 = ORIENTED_EDGE ( 'NONE', *, *, #31987, .F. ) ;
#2161 = ADVANCED_FACE ( 'NONE', ( #28145 ), #8119, .T. ) ;
#2162 = DIRECTION ( 'NONE',  ( 0.000000000000000000, 0.000000000000000000, 1.000000000000000000 ) ) ;
#2163 = CARTESIAN_POINT ( 'NONE',  ( 8.474859994195282908, 38.56284415653841791, 47.04930799450051637 ) ) ;
#2164 = CARTESIAN_POINT ( 'NONE',  ( 46.99023568444673060, 25.12451373492760354, 49.12151524109405898 ) ) ;
#2165 = VERTEX_POINT ( 'NONE', #13372 ) ;
#2166 = CIRCLE ( 'NONE', #8471, 54.49999999999997868 ) ;
#2167 = DIRECTION ( 'NONE',  ( 0.000000000000000000, 0.000000000000000000, 1.000000000000000000 ) ) ;
#2168 = TOROIDAL_SURFACE ( 'NONE', #3729, 12.40141737965280555, 0.1250000000000006939 ) ;
#2169 = CARTESIAN_POINT ( 'NONE',  ( 49.11022725746682482, 8.508769500014663478, -3.454732803723541412 ) ) ;
#2170 = VECTOR ( 'NONE', #280, 1000.000000000000227 ) ;
#2171 = FACE_OUTER_BOUND ( 'NONE', #29334, .T. ) ;
#2172 = CARTESIAN_POINT ( 'NONE',  ( 21.09785597605719332, 6.547041198165487685, 47.04930799450051637 ) ) ;
#2173 = DIRECTION ( 'NONE',  ( 0.000000000000000000, 0.000000000000000000, 1.000000000000000000 ) ) ;
#2174 = CARTESIAN_POINT ( 'NONE',  ( 21.09992658989238734, 38.56284415653841791, 47.04930799450051637 ) ) ;
#2175 = CARTESIAN_POINT ( 'NONE',  ( 8.698509210239507183, 24.09164230456639544, 47.04930799450051637 ) ) ;
#2176 =( BOUNDED_CURVE ( )  B_SPLINE_CURVE ( 2, ( #16600, #11860, #28765, #1508, #31877, #18903, #26621, #21353, #31399 ),
 .UNSPECIFIED., .F., .F. ) 
 B_SPLINE_CURVE_WITH_KNOTS ( ( 3, 2, 2, 2, 3 ),
 ( 0.2499999988387273664, 0.2619047619047618625, 0.2857142857142856984, 0.3095238095238095344, 0.3214285702672988188 ),
 .UNSPECIFIED. ) 
 CURVE ( )  GEOMETRIC_REPRESENTATION_ITEM ( )  RATIONAL_B_SPLINE_CURVE ( ( 0.9330127018922199644, 0.9330126953578159466, 1.000000000000000000, 0.8660254037844387076, 1.000000000000000000, 0.8660254037844387076, 1.000000000000000000, 0.9330127084266226500, 0.9330127018922199644 ) ) 
 REPRESENTATION_ITEM ( '' )  );
#2177 = FACE_BOUND ( 'NONE', #7800, .T. ) ;
#2178 = VERTEX_POINT ( 'NONE', #26147 ) ;
#2179 = ORIENTED_EDGE ( 'NONE', *, *, #10545, .T. ) ;
#2180 = DIRECTION ( 'NONE',  ( 0.000000000000000000, 0.000000000000000000, -1.000000000000000000 ) ) ;
#2181 = CARTESIAN_POINT ( 'NONE',  ( -40.40343367063677249, 8.556671693759611230, 34.56793150177820451 ) ) ;
#2182 = ADVANCED_FACE ( 'NONE', ( #18269 ), #2727, .T. ) ;
#2183 = CARTESIAN_POINT ( 'NONE',  ( -30.20912666432285576, 4.777658832336100225, 16.29113105709203779 ) ) ;
#2184 = FACE_OUTER_BOUND ( 'NONE', #24835, .T. ) ;
#2185 = VERTEX_POINT ( 'NONE', #23370 ) ;
#2186 = DIRECTION ( 'NONE',  ( -0.000000000000000000, -1.000000000000000000, 0.000000000000000000 ) ) ;
#2187 = FACE_OUTER_BOUND ( 'NONE', #30023, .T. ) ;
#2188 = CARTESIAN_POINT ( 'NONE',  ( 21.09992658989239089, 24.84164230456639544, 47.04930799450051637 ) ) ;
#2189 = ORIENTED_EDGE ( 'NONE', *, *, #15032, .T. ) ;
#2190 = ORIENTED_EDGE ( 'NONE', *, *, #7437, .T. ) ;
#2191 = CARTESIAN_POINT ( 'NONE',  ( -40.11096502192367552, 6.858424625636979854, 39.50614098478442315 ) ) ;
#2192 = CARTESIAN_POINT ( 'NONE',  ( 49.40414881150629611, 22.86454579224779948, 47.16908566558144855 ) ) ;
#2193 = ADVANCED_FACE ( 'NONE', ( #8276 ), #25512, .F. ) ;
#2194 = EDGE_CURVE ( 'NONE', #13126, #21006, #21056, .T. ) ;
#2195 = CARTESIAN_POINT ( 'NONE',  ( -9.880269303432738681, -5.935454207752202116, -12.62465409255485582 ) ) ;
#2196 = CARTESIAN_POINT ( 'NONE',  ( -39.45773241730296377, -5.935454212835550969, 77.98461610899785512 ) ) ;
#2197 = AXIS2_PLACEMENT_3D ( 'NONE', #3174, #13217, #12896 ) ;
#2198 = CARTESIAN_POINT ( 'NONE',  ( 44.85846160380767600, 29.33657771061399089, 47.75346028685437005 ) ) ;
#2199 = CIRCLE ( 'NONE', #20531, 1.999999999999998224 ) ;
#2200 = VERTEX_POINT ( 'NONE', #20416 ) ;
#2201 = ORIENTED_EDGE ( 'NONE', *, *, #8975, .T. ) ;
#2202 = ADVANCED_FACE ( 'NONE', ( #5648 ), #21568, .T. ) ;
#2203 = DIRECTION ( 'NONE',  ( 1.169615070119505487E-16, -0.2964022880492245271, 0.9550631830613013351 ) ) ;
#2204 = TOROIDAL_SURFACE ( 'NONE', #22655, 64.50000000000000000, 5.099019513592785380 ) ;
#2205 = ORIENTED_EDGE ( 'NONE', *, *, #12784, .F. ) ;
#2206 = DIRECTION ( 'NONE',  ( -0.000000000000000000, -1.000000000000000000, 0.000000000000000000 ) ) ;
#2207 = CARTESIAN_POINT ( 'NONE',  ( -30.66127778995677033, 3.242016564995574335, 78.70398512147052372 ) ) ;
#2208 = VECTOR ( 'NONE', #12644, 1000.000000000000000 ) ;
#2209 = ORIENTED_EDGE ( 'NONE', *, *, #15227, .F. ) ;
#2210 = DIRECTION ( 'NONE',  ( 1.234978253042719660E-16, -1.000000000000000000, -1.109335647967047851E-31 ) ) ;
#2211 = ORIENTED_EDGE ( 'NONE', *, *, #23688, .T. ) ;
#2212 = DIRECTION ( 'NONE',  ( 2.779292025043186357E-18, -1.288349127009862211E-17, 1.000000000000000000 ) ) ;
#2213 = AXIS2_PLACEMENT_3D ( 'NONE', #15394, #27549, #23100 ) ;
#2214 = EDGE_CURVE ( 'NONE', #31154, #24996, #28410, .T. ) ;
#2215 = CARTESIAN_POINT ( 'NONE',  ( 21.09785597605719332, 30.36454579224779238, 47.04930799450051637 ) ) ;
#2216 = CARTESIAN_POINT ( 'NONE',  ( -40.68134976037170247, 6.801398876102698665, 39.48202140826487039 ) ) ;
#2217 = ORIENTED_EDGE ( 'NONE', *, *, #17290, .F. ) ;
#2218 = LINE ( 'NONE', #6977, #1848 ) ;
#2219 = CARTESIAN_POINT ( 'NONE',  ( 21.09785597605720753, -5.098646251524523443, 47.04930799450052348 ) ) ;
#2220 = CARTESIAN_POINT ( 'NONE',  ( -42.21195563036362586, 4.051200314738734320, 57.04930799450051637 ) ) ;
#2221 = EDGE_CURVE ( 'NONE', #19350, #26434, #20578, .T. ) ;
#2222 = DIRECTION ( 'NONE',  ( 1.000000000000000000, 0.000000000000000000, -1.224646799147353207E-16 ) ) ;
#2223 = DIRECTION ( 'NONE',  ( 0.000000000000000000, 0.000000000000000000, -1.000000000000000000 ) ) ;
#2224 = EDGE_LOOP ( 'NONE', ( #3469, #18305, #23139, #26666 ) ) ;
#2225 = CARTESIAN_POINT ( 'NONE',  ( 21.09992658989238734, 31.34184655352422766, 47.04930799450051637 ) ) ;
#2226 = DIRECTION ( 'NONE',  ( 0.000000000000000000, 0.000000000000000000, -1.000000000000000000 ) ) ;
#2227 = ORIENTED_EDGE ( 'NONE', *, *, #224, .T. ) ;
#2228 = EDGE_CURVE ( 'NONE', #27481, #12804, #5802, .T. ) ;
#2229 = DIRECTION ( 'NONE',  ( -1.000000000000000000, 0.000000000000000000, 0.000000000000000000 ) ) ;
#2230 = EDGE_CURVE ( 'NONE', #2858, #3439, #19942, .T. ) ;
#2231 = AXIS2_PLACEMENT_3D ( 'NONE', #13331, #839, #8554 ) ;
#2232 = ORIENTED_EDGE ( 'NONE', *, *, #29944, .F. ) ;
#2233 = PRODUCT_DEFINITION_SHAPE ( 'NONE', 'NONE',  #31780 ) ;
#2234 = ORIENTED_EDGE ( 'NONE', *, *, #4882, .T. ) ;
#2235 = AXIS2_PLACEMENT_3D ( 'NONE', #7426, #28093, #26096 ) ;
#2236 = AXIS2_PLACEMENT_3D ( 'NONE', #31647, #8988, #24078 ) ;
#2237 = ORIENTED_EDGE ( 'NONE', *, *, #16879, .F. ) ;
#2238 = PRODUCT_DEFINITION_SHAPE ( 'NONE', 'NONE',  #32500 ) ;
#2239 = CARTESIAN_POINT ( 'NONE',  ( 33.71785032049134401, 28.21664230456639899, 47.04930799450051637 ) ) ;
#2240 = ORIENTED_EDGE ( 'NONE', *, *, #13865, .T. ) ;
#2241 = ORIENTED_EDGE ( 'NONE', *, *, #24153, .T. ) ;
#2242 = CARTESIAN_POINT ( 'NONE',  ( 21.09785597605720753, -5.098646251524523443, 47.04930799450052348 ) ) ;
#2243 = AXIS2_PLACEMENT_3D ( 'NONE', #9490, #16213, #21781 ) ;
#2244 = CARTESIAN_POINT ( 'NONE',  ( 21.09992658989238734, 38.56284415653841791, 47.04930799450051637 ) ) ;
#2245 = FACE_BOUND ( 'NONE', #17285, .T. ) ;
#2246 = DIRECTION ( 'NONE',  ( 0.2756373558169973870, -0.9612616959383193382, -1.315048337272770280E-17 ) ) ;
#2247 = CIRCLE ( 'NONE', #18498, 55.68770647617149194 ) ;
#2248 = EDGE_CURVE ( 'NONE', #4768, #9952, #1584, .T. ) ;
#2249 = DIRECTION ( 'NONE',  ( -1.000000000000000000, 0.000000000000000000, 0.000000000000000000 ) ) ;
#2250 = VERTEX_POINT ( 'NONE', #25434 ) ;
#2251 = CARTESIAN_POINT ( 'NONE',  ( -8.054007235165986600, 7.161243906346020260, 97.76730497187020319 ) ) ;
#2252 = ORIENTED_EDGE ( 'NONE', *, *, #26261, .T. ) ;
#2253 = CARTESIAN_POINT ( 'NONE',  ( -30.29083761341767911, 10.19527012171080393, 20.98910367824052159 ) ) ;
#2254 = LINE ( 'NONE', #4716, #27916 ) ;
#2255 = EDGE_LOOP ( 'NONE', ( #24827, #13187, #8431, #1234 ) ) ;
#2256 = CARTESIAN_POINT ( 'NONE',  ( 81.79971628361815306, -5.937394935145312580, 77.97850100859398026 ) ) ;
#2257 = DIRECTION ( 'NONE',  ( 1.188208965918165239E-16, 1.880121038077813132E-16, 1.000000000000000000 ) ) ;
#2258 = ADVANCED_FACE ( 'NONE', ( #20179 ), #3094, .F. ) ;
#2259 = CARTESIAN_POINT ( 'NONE',  ( 52.07598125554711999, -5.935454207752202116, 107.5832303370038403 ) ) ;
#2260 = CARTESIAN_POINT ( 'NONE',  ( -40.59783130604490253, 7.538194345349022996, 60.10545738969978657 ) ) ;
#2261 = LINE ( 'NONE', #29841, #23746 ) ;
#2262 = CARTESIAN_POINT ( 'NONE',  ( 49.49063479933183629, 28.71291119454914664, 47.17357720316391578 ) ) ;
#2263 = AXIS2_PLACEMENT_3D ( 'NONE', #4002, #14021, #19083 ) ;
#2264 = AXIS2_PLACEMENT_3D ( 'NONE', #20141, #15067, #20297 ) ;
#2265 = CARTESIAN_POINT ( 'NONE',  ( -41.94956971822180947, 3.905757428664828890, 48.94930799450051495 ) ) ;
#2266 = CARTESIAN_POINT ( 'NONE',  ( 21.09992658989239089, 28.09143805560861296, 47.04930799450051637 ) ) ;
#2267 = VERTEX_POINT ( 'NONE', #13133 ) ;
#2268 = CARTESIAN_POINT ( 'NONE',  ( 106.0978559760574313, 1.925589859889728972, 67.46350265493050813 ) ) ;
#2269 = DIRECTION ( 'NONE',  ( 0.8907924160295465077, 1.100109261771873178E-16, -0.4544104659272754643 ) ) ;
#2270 = ORIENTED_EDGE ( 'NONE', *, *, #18446, .F. ) ;
#2271 = EDGE_CURVE ( 'NONE', #6626, #25934, #27412, .T. ) ;
#2272 = CARTESIAN_POINT ( 'NONE',  ( 58.09785597605721108, -5.098646251524523443, 47.04930799450051637 ) ) ;
#2273 = CARTESIAN_POINT ( 'NONE',  ( -29.27337757263006424, -3.086620340690746644, 13.27411520529475020 ) ) ;
#2274 = ORIENTED_EDGE ( 'NONE', *, *, #22337, .T. ) ;
#2275 = ORIENTED_EDGE ( 'NONE', *, *, #262, .T. ) ;
#2276 = DIRECTION ( 'NONE',  ( -1.101824276508909887E-16, 1.000000000000000000, -0.000000000000000000 ) ) ;
#2277 = ORIENTED_EDGE ( 'NONE', *, *, #32113, .T. ) ;
#2278 = VECTOR ( 'NONE', #21411, 1000.000000000000000 ) ;
#2279 = AXIS2_PLACEMENT_3D ( 'NONE', #14814, #20364, #10056 ) ;
#2280 = AXIS2_PLACEMENT_3D ( 'NONE', #12246, #32269, #2712 ) ;
#2281 = VECTOR ( 'NONE', #28156, 1000.000000000000000 ) ;
#2282 = AXIS2_PLACEMENT_3D ( 'NONE', #8168, #15877, #13267 ) ;
#2283 = ORIENTED_EDGE ( 'NONE', *, *, #5714, .F. ) ;
#2284 = CARTESIAN_POINT ( 'NONE',  ( -40.69193635511749108, 9.347952559758585522, 39.44930799450052206 ) ) ;
#2285 = DIRECTION ( 'NONE',  ( 0.9612616959383207815, 0.2756373558169926685, 8.795445018804289444E-19 ) ) ;
#2286 = VERTEX_POINT ( 'NONE', #12813 ) ;
#2287 = CARTESIAN_POINT ( 'NONE',  ( 21.09992658989239089, 23.84184655352419213, 47.04930799450051637 ) ) ;
#2288 = LINE ( 'NONE', #30033, #23866 ) ;
#2289 = CARTESIAN_POINT ( 'NONE',  ( 49.19517401419062708, 26.30920399681023270, 48.40991706654173754 ) ) ;
#2290 = CARTESIAN_POINT ( 'NONE',  ( 48.91284552371730143, 29.49289516297709213, 46.12344667017377020 ) ) ;
#2291 = VERTEX_POINT ( 'NONE', #15100 ) ;
#2292 = ORIENTED_EDGE ( 'NONE', *, *, #24852, .F. ) ;
#2293 = SURFACE_STYLE_USAGE ( .BOTH. , #14775 ) ;
#2294 = ORIENTED_EDGE ( 'NONE', *, *, #13052, .T. ) ;
#2295 = CARTESIAN_POINT ( 'NONE',  ( -40.50410981870283678, 7.604537000166496696, 35.33853321918559232 ) ) ;
#2296 = DIRECTION ( 'NONE',  ( -0.2756373558169973870, 0.9612616959383193382, 1.315048337272770435E-17 ) ) ;
#2297 = CARTESIAN_POINT ( 'NONE',  ( -40.69423955692155204, 6.789232590171223158, 34.67341590623290415 ) ) ;
#2298 = CIRCLE ( 'NONE', #6486, 0.1250000000000001110 ) ;
#2299 = DIRECTION ( 'NONE',  ( -0.9612616959383205595, -0.2756373558169931681, 1.660411357259282445E-16 ) ) ;
#2300 = CARTESIAN_POINT ( 'NONE',  ( 45.35708200440645044, 28.30457786121581876, 45.92000246470680480 ) ) ;
#2301 = SHAPE_DEFINITION_REPRESENTATION ( #8290, #3604 ) ;
#2302 = VERTEX_POINT ( 'NONE', #10339 ) ;
#2303 = ORIENTED_EDGE ( 'NONE', *, *, #4028, .F. ) ;
#2304 = CARTESIAN_POINT ( 'NONE',  ( -42.33363892739273382, 14.73725438281773847, 58.96402370174222085 ) ) ;
#2305 = LINE ( 'NONE', #9697, #452 ) ;
#2306 = EDGE_CURVE ( 'NONE', #17291, #14793, #22637, .T. ) ;
#2307 = TOROIDAL_SURFACE ( 'NONE', #26411, 15.35463912851480828, 0.6621856154243856984 ) ;
#2308 = ADVANCED_FACE ( 'NONE', ( #22469 ), #25270, .T. ) ;
#2309 = FACE_OUTER_BOUND ( 'NONE', #10411, .T. ) ;
#2310 = EDGE_CURVE ( 'NONE', #12604, #19419, #3241, .T. ) ;
#2311 = EDGE_CURVE ( 'NONE', #7331, #3673, #14263, .T. ) ;
#2312 = VERTEX_POINT ( 'NONE', #20333 ) ;
#2313 = CARTESIAN_POINT ( 'NONE',  ( 52.07598125554711999, -5.935454207752203004, 107.5573216553427187 ) ) ;
#2314 = PLANE ( 'NONE',  #32485 ) ;
#2315 = ORIENTED_EDGE ( 'NONE', *, *, #2221, .T. ) ;
#2316 = LINE ( 'NONE', #32192, #548 ) ;
#2317 = CARTESIAN_POINT ( 'NONE',  ( -40.63136629056263160, 9.462201496834369507, 39.42930412971698217 ) ) ;
#2318 = CARTESIAN_POINT ( 'NONE',  ( 21.09785597605719332, 17.36451738380053555, 47.04930799450051637 ) ) ;
#2319 = VERTEX_POINT ( 'NONE', #5069 ) ;
#2320 = CONICAL_SURFACE ( 'NONE', #20662, 58.70143199044622406, 1.269872874662816509 ) ;
#2321 = ORIENTED_EDGE ( 'NONE', *, *, #21254, .F. ) ;
#2322 = AXIS2_PLACEMENT_3D ( 'NONE', #5370, #12921, #15687 ) ;
#2323 = CARTESIAN_POINT ( 'NONE',  ( -41.08785830660042393, 9.277514380576530328, 34.69072935073783981 ) ) ;
#2324 = CARTESIAN_POINT ( 'NONE',  ( 73.19394920542428906, 11.69997306056223607, 69.64732492378499273 ) ) ;
#2326 = CARTESIAN_POINT ( 'NONE',  ( 44.70507715278255745, 27.04951373492760069, 46.92503878583765697 ) ) ;
#2325 = AXIS2_PLACEMENT_3D ( 'NONE', #7259, #22180, #32208 ) ;
#2327 = VECTOR ( 'NONE', #6599, 1000.000000000000114 ) ;
#2328 = ORIENTED_EDGE ( 'NONE', *, *, #25601, .T. ) ;
#2329 = DIRECTION ( 'NONE',  ( -1.000000000000000000, 0.000000000000000000, 0.000000000000000000 ) ) ;
#2330 = CARTESIAN_POINT ( 'NONE',  ( 21.09785597605720042, -13.59284023713420630, 47.04930799450051637 ) ) ;
#2331 = ADVANCED_FACE ( 'NONE', ( #5088 ), #8204, .T. ) ;
#2332 = CARTESIAN_POINT ( 'NONE',  ( -42.73182147790732444, -0.8057266458565844891, 61.94930799450052206 ) ) ;
#2333 = DIRECTION ( 'NONE',  ( -0.4848096202463673121, -0.8746197071393789768, 0.000000000000000000 ) ) ;
#2334 = DIRECTION ( 'NONE',  ( -0.000000000000000000, 1.000000000000000000, -0.000000000000000000 ) ) ;
#2335 = DIRECTION ( 'NONE',  ( -0.9097384655268497822, -0.4151817967359032191, -2.820562191637069803E-18 ) ) ;
#2336 = DIRECTION ( 'NONE',  ( -1.000000000000000000, -6.722685822323786766E-17, 0.000000000000000000 ) ) ;
#2337 = DIRECTION ( 'NONE',  ( 0.000000000000000000, 1.000000000000000000, 0.000000000000000000 ) ) ;
#2338 = DIRECTION ( 'NONE',  ( -1.000000000000000000, 0.000000000000000000, 0.000000000000000000 ) ) ;
#2339 = CARTESIAN_POINT ( 'NONE',  ( -40.58388821705207761, 6.836049376365832764, 39.54676951983897482 ) ) ;
#2340 = ORIENTED_EDGE ( 'NONE', *, *, #16245, .T. ) ;
#2341 = EDGE_LOOP ( 'NONE', ( #4125, #591, #7956, #5863 ) ) ;
#2342 = CARTESIAN_POINT ( 'NONE',  ( 33.72499318558949000, 38.56284415653841791, 47.04930799450051637 ) ) ;
#2343 = CARTESIAN_POINT ( 'NONE',  ( 48.28214861297873739, 25.48954579807170262, 49.37090702980594159 ) ) ;
#2344 = FACE_OUTER_BOUND ( 'NONE', #18141, .T. ) ;
#2345 = ADVANCED_FACE ( 'NONE', ( #27573 ), #1218, .F. ) ;
#2346 = DIRECTION ( 'NONE',  ( -1.000000000000000000, 0.000000000000000000, 0.000000000000000000 ) ) ;
#2347 = EDGE_CURVE ( 'NONE', #16477, #663, #28484, .T. ) ;
#2348 = AXIS2_PLACEMENT_3D ( 'NONE', #11822, #13796, #19020 ) ;
#2349 = EDGE_CURVE ( 'NONE', #63, #14845, #17884, .T. ) ;
#2350 = EDGE_LOOP ( 'NONE', ( #17700, #31035, #31048, #18559 ) ) ;
#2351 = DIRECTION ( 'NONE',  ( -1.101824276508909887E-16, 1.000000000000000000, -0.000000000000000000 ) ) ;
#2352 = DIRECTION ( 'NONE',  ( -0.4848096202463432203, -0.8746197071393924105, -9.920727850371698576E-18 ) ) ;
#2353 = DIRECTION ( 'NONE',  ( -1.000000000000000000, 0.000000000000000000, 0.000000000000000000 ) ) ;
#2354 = ORIENTED_EDGE ( 'NONE', *, *, #13031, .T. ) ;
#2355 = EDGE_LOOP ( 'NONE', ( #9054, #15659, #16923, #25728 ) ) ;
#2357 = AXIS2_PLACEMENT_3D ( 'NONE', #14559, #12104, #2413 ) ;
#2356 = DIRECTION ( 'NONE',  ( 0.8746197071393925215, -0.4848096202463429982, -8.676864087101708112E-18 ) ) ;
#2358 = EDGE_CURVE ( 'NONE', #19852, #10175, #31112, .T. ) ;
#2359 = CARTESIAN_POINT ( 'NONE',  ( 48.40186567930498285, 29.61618040159425647, 45.03923535223908203 ) ) ;
#2360 = AXIS2_PLACEMENT_3D ( 'NONE', #29508, #9641, #14246 ) ;
#2361 = AXIS2_PLACEMENT_3D ( 'NONE', #2640, #32194, #175 ) ;
#2362 = LINE ( 'NONE', #7286, #1034 ) ;
#2363 = DIRECTION ( 'NONE',  ( -1.101824276508909887E-16, 1.000000000000000000, -0.000000000000000000 ) ) ;
#2364 = CIRCLE ( 'NONE', #2885, 0.09999999999999795164 ) ;
#2365 = CARTESIAN_POINT ( 'NONE',  ( 45.06051016020553135, 29.34935871078510061, 48.15932322090515783 ) ) ;
#2366 = ORIENTED_EDGE ( 'NONE', *, *, #387, .F. ) ;
#2367 = ORIENTED_EDGE ( 'NONE', *, *, #7537, .F. ) ;
#2368 = DIRECTION ( 'NONE',  ( 0.2756373558169961102, -0.9612616959383197823, 0.000000000000000000 ) ) ;
#2369 = ORIENTED_EDGE ( 'NONE', *, *, #31211, .T. ) ;
#2370 = B_SPLINE_CURVE_WITH_KNOTS ( 'NONE', 3,
 ( #26492, #9256, #1701, #11084, #6306, #13541, #14023, #16794, #16311, #21071, #11722, #18604 ),
 .UNSPECIFIED., .F., .F.,
 ( 4, 2, 2, 2, 2, 4 ),
 ( 0.0003422370341462280100, 0.002080102550335780759, 0.003817968066525333128, 0.005555833582714885498, 0.006424766340809661899, 0.007293699098904438301 ),
 .UNSPECIFIED. ) ;
#2371 =( BOUNDED_CURVE ( )  B_SPLINE_CURVE ( 3, ( #7988, #13550, #13400, #3525 ),
 .UNSPECIFIED., .F., .F. ) 
 B_SPLINE_CURVE_WITH_KNOTS ( ( 4, 4 ),
 ( 4.712388980384693227, 6.283185307179583567 ),
 .UNSPECIFIED. ) 
 CURVE ( )  GEOMETRIC_REPRESENTATION_ITEM ( )  RATIONAL_B_SPLINE_CURVE ( ( 1.000000000000000000, 0.8047378541243658256, 0.8047378541243658256, 1.000000000000000000 ) ) 
 REPRESENTATION_ITEM ( '' )  );
#2372 = CARTESIAN_POINT ( 'NONE',  ( 21.09992658989239089, 29.71183152705961561, 47.04930799450051637 ) ) ;
#2373 = DIRECTION ( 'NONE',  ( 0.9612616959383198934, 0.2756373558169958327, 1.367252280957423978E-15 ) ) ;
#2374 = CIRCLE ( 'NONE', #7609, 1.142135311067127512 ) ;
#2375 = ADVANCED_FACE ( 'NONE', ( #3584 ), #9623, .T. ) ;
#2376 = AXIS2_PLACEMENT_3D ( 'NONE', #32094, #11579, #21574 ) ;
#2377 = ADVANCED_FACE ( 'NONE', ( #28694 ), #25755, .F. ) ;
#2378 = CIRCLE ( 'NONE', #28592, 1.199999999999999734 ) ;
#2379 = EDGE_LOOP ( 'NONE', ( #32400, #27308 ) ) ;
#2380 = CARTESIAN_POINT ( 'NONE',  ( -40.74365851677129768, 8.439942589813739460, 34.54930799450052348 ) ) ;
#2381 = ORIENTED_EDGE ( 'NONE', *, *, #26036, .T. ) ;
#2382 = DIRECTION ( 'NONE',  ( -1.000000000000000000, -1.101824276508910010E-16, 0.000000000000000000 ) ) ;
#2383 = DIRECTION ( 'NONE',  ( -1.101824276508909887E-16, 1.000000000000000000, -0.000000000000000000 ) ) ;
#2384 = VERTEX_POINT ( 'NONE', #6061 ) ;
#2385 = CARTESIAN_POINT ( 'NONE',  ( 72.66453678218256584, 3.903925281081655818, 78.31450457581732394 ) ) ;
#2386 = CARTESIAN_POINT ( 'NONE',  ( 21.09992658989238734, 38.56284415653841791, 47.04930799450051637 ) ) ;
#2387 = PLANE ( 'NONE',  #11604 ) ;
#2388 = DIRECTION ( 'NONE',  ( -0.000000000000000000, -1.000000000000000000, -0.000000000000000000 ) ) ;
#2389 = CARTESIAN_POINT ( 'NONE',  ( 21.09785597605719332, 25.56454579224779167, 33.84930799450050642 ) ) ;
#2390 = FACE_OUTER_BOUND ( 'NONE', #24514, .T. ) ;
#2391 = ORIENTED_EDGE ( 'NONE', *, *, #4341, .T. ) ;
#2392 = DIRECTION ( 'NONE',  ( -1.000000000000000000, 0.000000000000000000, 0.000000000000000000 ) ) ;
#2393 = DIRECTION ( 'NONE',  ( 1.000000000000000000, 0.000000000000000000, 0.000000000000000000 ) ) ;
#2394 = ORIENTED_EDGE ( 'NONE', *, *, #12400, .T. ) ;
#2395 = EDGE_CURVE ( 'NONE', #16985, #13978, #11459, .T. ) ;
#2396 = CARTESIAN_POINT ( 'NONE',  ( 21.09992658989238734, 38.56284415653841791, 47.04930799450051637 ) ) ;
#2397 = CYLINDRICAL_SURFACE ( 'NONE', #18502, 12.36707279061065101 ) ;
#2398 = ORIENTED_EDGE ( 'NONE', *, *, #27659, .T. ) ;
#2399 = CIRCLE ( 'NONE', #23356, 55.96105416618080142 ) ;
#2400 = ORIENTED_EDGE ( 'NONE', *, *, #2953, .T. ) ;
#2401 = AXIS2_PLACEMENT_3D ( 'NONE', #18268, #13216, #8748 ) ;
#2402 = ORIENTED_EDGE ( 'NONE', *, *, #17078, .T. ) ;
#2403 = EDGE_CURVE ( 'NONE', #27591, #9758, #4892, .T. ) ;
#2404 = EDGE_CURVE ( 'NONE', #11885, #27524, #27429, .T. ) ;
#2405 = AXIS2_PLACEMENT_3D ( 'NONE', #30954, #8619, #21237 ) ;
#2406 = CARTESIAN_POINT ( 'NONE',  ( 21.09785597605719332, 48.06454579224779877, 50.00023834876391504 ) ) ;
#2407 = ADVANCED_FACE ( 'NONE', ( #31327 ), #27966, .T. ) ;
#2408 = EDGE_CURVE ( 'NONE', #23152, #30572, #16379, .T. ) ;
#2409 = ORIENTED_EDGE ( 'NONE', *, *, #31113, .F. ) ;
#2410 = VERTEX_POINT ( 'NONE', #31491 ) ;
#2411 = FACE_OUTER_BOUND ( 'NONE', #20446, .T. ) ;
#2412 = LINE ( 'NONE', #12429, #29320 ) ;
#2413 = DIRECTION ( 'NONE',  ( -1.000000000000000000, 0.000000000000000000, 0.000000000000000000 ) ) ;
#2414 = LINE ( 'NONE', #22260, #684 ) ;
#2415 = CARTESIAN_POINT ( 'NONE',  ( 49.64105649875294546, 24.93604219378083187, 46.47965702198763438 ) ) ;
#2416 = ORIENTED_EDGE ( 'NONE', *, *, #23784, .F. ) ;
#2417 = DIRECTION ( 'NONE',  ( -0.9612616959383194493, -0.2756373558169974980, -8.795445018804946186E-19 ) ) ;
#2418 = EDGE_LOOP ( 'NONE', ( #26739, #13481, #9987, #17226 ) ) ;
#2419 = CARTESIAN_POINT ( 'NONE',  ( 21.09992658989239089, 25.09184655352419213, 47.04930799450051637 ) ) ;
#2421 = DIRECTION ( 'NONE',  ( 0.1949050434465355863, -0.6797146636928657060, 0.7071067811865464625 ) ) ;
#2420 = VECTOR ( 'NONE', #13652, 1000.000000000000000 ) ;
#2422 = PRODUCT_DEFINITION_FORMATION_WITH_SPECIFIED_SOURCE ( 'ANY', '', #14546, .NOT_KNOWN. ) ;
#2423 = ORIENTED_EDGE ( 'NONE', *, *, #7011, .F. ) ;
#2424 = DIRECTION ( 'NONE',  ( -1.000000000000000000, 0.000000000000000000, 0.000000000000000000 ) ) ;
#2425 = DIRECTION ( 'NONE',  ( 0.1949050434465264547, -0.6797146636928678154, 0.7071067811865470176 ) ) ;
#2426 = CARTESIAN_POINT ( 'NONE',  ( -35.12632216515691397, 11.92558985988973674, 54.04930799450053769 ) ) ;
#2427 = FACE_OUTER_BOUND ( 'NONE', #23670, .T. ) ;
#2428 = DIRECTION ( 'NONE',  ( -1.000000000000000000, 0.000000000000000000, 0.000000000000000000 ) ) ;
#2429 = CARTESIAN_POINT ( 'NONE',  ( 45.24946171279598417, 27.72124452788248661, 47.99220971130007030 ) ) ;
#2430 = CARTESIAN_POINT ( 'NONE',  ( 21.09992658989238734, 31.59184655352418503, 47.04930799450051637 ) ) ;
#2431 = VERTEX_POINT ( 'NONE', #1125 ) ;
#2432 = EDGE_CURVE ( 'NONE', #5318, #19617, #8358, .T. ) ;
#2433 = FACE_OUTER_BOUND ( 'NONE', #2418, .T. ) ;
#2434 = CARTESIAN_POINT ( 'NONE',  ( -44.16105795751995799, -3.935454207752183020, 52.04930799450050927 ) ) ;
#2435 = ORIENTED_EDGE ( 'NONE', *, *, #10167, .T. ) ;
#2436 = CIRCLE ( 'NONE', #25489, 12.62506659569710266 ) ;
#2437 = CARTESIAN_POINT ( 'NONE',  ( 8.698509210239548040, 28.09164230456639544, 47.04930799450051637 ) ) ;
#2438 = ORIENTED_EDGE ( 'NONE', *, *, #7569, .T. ) ;
#2439 = EDGE_LOOP ( 'NONE', ( #4209, #25565, #3242, #13634 ) ) ;
#2440 = CARTESIAN_POINT ( 'NONE',  ( 21.09992658989239089, 29.09164230456639899, 47.04930799450051637 ) ) ;
#2441 = VERTEX_POINT ( 'NONE', #13301 ) ;
#2442 = EDGE_CURVE ( 'NONE', #22267, #8364, #13818, .T. ) ;
#2443 = AXIS2_PLACEMENT_3D ( 'NONE', #21790, #26722, #9166 ) ;
#2444 = ORIENTED_EDGE ( 'NONE', *, *, #12081, .T. ) ;
#2445 = ADVANCED_FACE ( 'NONE', ( #28546 ), #31168, .F. ) ;
#2446 = ORIENTED_EDGE ( 'NONE', *, *, #12465, .T. ) ;
#2447 = CARTESIAN_POINT ( 'NONE',  ( 21.09785597605718976, 6.547041198165487685, 67.43013672359793986 ) ) ;
#2448 = FACE_OUTER_BOUND ( 'NONE', #29487, .T. ) ;
#2449 = EDGE_CURVE ( 'NONE', #28013, #10438, #11704, .T. ) ;
#2450 = AXIS2_PLACEMENT_3D ( 'NONE', #27101, #16920, #14639 ) ;
#2451 = VERTEX_POINT ( 'NONE', #23452 ) ;
#2452 = EDGE_CURVE ( 'NONE', #15022, #19678, #30061, .T. ) ;
#2453 = DIRECTION ( 'NONE',  ( -0.000000000000000000, -1.000000000000000000, -0.000000000000000000 ) ) ;
#2454 = LINE ( 'NONE', #32490, #18082 ) ;
#2455 = CARTESIAN_POINT ( 'NONE',  ( 49.49063479933183629, 25.91291119454915304, 47.17357720316391578 ) ) ;
#2456 = ORIENTED_EDGE ( 'NONE', *, *, #11933, .T. ) ;
#2457 = ORIENTED_EDGE ( 'NONE', *, *, #2724, .T. ) ;
#2458 = CARTESIAN_POINT ( 'NONE',  ( 8.474859994195286461, 24.84143805560860940, 47.04930799450051637 ) ) ;
#2459 = ORIENTED_EDGE ( 'NONE', *, *, #29086, .F. ) ;
#2460 = DIRECTION ( 'NONE',  ( -0.000000000000000000, -1.000000000000000000, -0.000000000000000000 ) ) ;
#2461 = DIRECTION ( 'NONE',  ( -1.101824276508909887E-16, 1.000000000000000000, -0.000000000000000000 ) ) ;
#2462 = DIRECTION ( 'NONE',  ( -1.101824276508909887E-16, 1.000000000000000000, -0.000000000000000000 ) ) ;
#2463 = DIRECTION ( 'NONE',  ( -0.000000000000000000, -1.000000000000000000, 0.000000000000000000 ) ) ;
#2464 = DIRECTION ( 'NONE',  ( 0.2756373558170082672, -0.9612616959383162296, 0.000000000000000000 ) ) ;
#2465 = APPLICATION_PROTOCOL_DEFINITION ( 'draft international standard', 'automotive_design', 1998, #9722 ) ;
#2466 = EDGE_LOOP ( 'NONE', ( #32496, #15726, #538, #3563 ) ) ;
#2467 = VERTEX_POINT ( 'NONE', #8521 ) ;
#2468 = CARTESIAN_POINT ( 'NONE',  ( -23.40214402394279247, 13.86454579224779948, 47.04930799450052348 ) ) ;
#2469 = AXIS2_PLACEMENT_3D ( 'NONE', #9577, #14503, #4644 ) ;
#2470 = CARTESIAN_POINT ( 'NONE',  ( 21.09992658989238734, 38.56284415653841791, 47.04930799450051637 ) ) ;
#2471 = CARTESIAN_POINT ( 'NONE',  ( -41.93344242462055149, 13.82826554927147988, 59.53596428539564300 ) ) ;
#2472 = EDGE_LOOP ( 'NONE', ( #26108, #20058 ) ) ;
#2473 = CARTESIAN_POINT ( 'NONE',  ( 44.70507715278255034, 27.04951373492759714, 46.92503878583765697 ) ) ;
#2474 = ORIENTED_EDGE ( 'NONE', *, *, #3629, .F. ) ;
#2475 = FACE_OUTER_BOUND ( 'NONE', #10012, .T. ) ;
#2476 = DIRECTION ( 'NONE',  ( 0.4544104193609915243, 0.000000000000000000, 0.8907924397839082076 ) ) ;
#2477 = CYLINDRICAL_SURFACE ( 'NONE', #20687, 0.1000000000000008243 ) ;
#2478 = ORIENTED_EDGE ( 'NONE', *, *, #16762, .T. ) ;
#2479 = VERTEX_POINT ( 'NONE', #18513 ) ;
#2480 = CARTESIAN_POINT ( 'NONE',  ( 21.09785597605720753, 13.86454579224779948, 47.04930799450052348 ) ) ;
#2481 = AXIS2_PLACEMENT_3D ( 'NONE', #20226, #2351, #30251 ) ;
#2482 = CARTESIAN_POINT ( 'NONE',  ( 49.64623691886138346, 24.93450097658724118, 46.50278401396133177 ) ) ;
#2483 = CARTESIAN_POINT ( 'NONE',  ( 48.66895200406656130, 27.88420399681022488, 44.62753372671561181 ) ) ;
#2484 = EDGE_CURVE ( 'NONE', #20946, #18375, #23232, .T. ) ;
#2485 = VERTEX_POINT ( 'NONE', #18673 ) ;
#2486 = EDGE_CURVE ( 'NONE', #7948, #25895, #16934, .T. ) ;
#2487 = CIRCLE ( 'NONE', #911, 1.300000000000002487 ) ;
#2488 = DIRECTION ( 'NONE',  ( 0.8746197071393926326, -0.4848096202463430537, -8.676864087101709653E-18 ) ) ;
#2489 = CARTESIAN_POINT ( 'NONE',  ( 45.36511207810797686, 27.20948166895303189, 45.12672418911604666 ) ) ;
#2490 = FACE_OUTER_BOUND ( 'NONE', #13565, .T. ) ;
#2491 = CYLINDRICAL_SURFACE ( 'NONE', #241, 33.50000000000000000 ) ;
#2492 = CARTESIAN_POINT ( 'NONE',  ( -42.60588768478345401, 14.57151196022700113, 37.04930799450052348 ) ) ;
#2493 = CYLINDRICAL_SURFACE ( 'NONE', #10685, 0.1000000000000018235 ) ;
#2494 = DIRECTION ( 'NONE',  ( 1.313185983435984691E-29, -1.000000000000000000, -3.761114140369702165E-15 ) ) ;
#2495 = DIRECTION ( 'NONE',  ( -1.000000000000000000, 0.000000000000000000, 0.000000000000000000 ) ) ;
#2496 = B_SPLINE_SURFACE_WITH_KNOTS ( 'NONE', 3, 1, ( 
 ( #29765, #9584 ),
 ( #21872, #27467 ),
 ( #9252, #19905 ),
 ( #19413, #31899 ) ),
 .UNSPECIFIED., .F., .F., .F.,
 ( 4, 4 ),
 ( 2, 2 ),
 ( 0.9958781556774846111, 1.000000000000000000 ),
 ( 0.000000000000000000, 1.000000000000000000 ),
 .UNSPECIFIED. ) ;
#2497 = CARTESIAN_POINT ( 'NONE',  ( 21.09785597605720753, -5.098646251524523443, 47.04930799450052348 ) ) ;
#2498 = CARTESIAN_POINT ( 'NONE',  ( 21.09785597605719332, 40.06454579224778456, 59.04930799450051637 ) ) ;
#2499 = VERTEX_POINT ( 'NONE', #11306 ) ;
#2500 = ORIENTED_EDGE ( 'NONE', *, *, #9156, .F. ) ;
#2501 = CARTESIAN_POINT ( 'NONE',  ( 44.79156314060809763, 19.96454579224779380, 46.92953032342012420 ) ) ;
#2502 = DIRECTION ( 'NONE',  ( 0.3428121700606596156, 0.6184495258776487869, 0.7071067811865566766 ) ) ;
#2503 = CARTESIAN_POINT ( 'NONE',  ( -43.90780810587784089, -0.03953120679776574165, 32.14930799450051779 ) ) ;
#2504 = CARTESIAN_POINT ( 'NONE',  ( 48.23388202445966044, 26.95087065737812182, 49.27628909396054979 ) ) ;
#2505 = ORIENTED_EDGE ( 'NONE', *, *, #17038, .T. ) ;
#2506 = LINE ( 'NONE', #12858, #30280 ) ;
#2507 = DIRECTION ( 'NONE',  ( -1.000000000000000000, 0.000000000000000000, 0.000000000000000000 ) ) ;
#2508 = CARTESIAN_POINT ( 'NONE',  ( 41.51205063648687599, 11.92558985988973497, -4.944603100128015960 ) ) ;
#2509 = ORIENTED_EDGE ( 'NONE', *, *, #10196, .T. ) ;
#2510 = ORIENTED_EDGE ( 'NONE', *, *, #19097, .T. ) ;
#2511 = CARTESIAN_POINT ( 'NONE',  ( 46.04844006429464542, 19.96454579224779380, 44.99211097489548905 ) ) ;
#2512 = CARTESIAN_POINT ( 'NONE',  ( 49.49063479933183629, 28.09951373492759430, 47.17357720316391578 ) ) ;
#2513 = AXIS2_PLACEMENT_3D ( 'NONE', #3595, #31183, #18047 ) ;
#2514 = DIRECTION ( 'NONE',  ( -0.000000000000000000, -1.000000000000000000, -0.000000000000000000 ) ) ;
#2515 = CIRCLE ( 'NONE', #13073, 58.84990142703892246 ) ;
#2516 = CARTESIAN_POINT ( 'NONE',  ( 45.14219408817155710, 29.35362821189650617, 48.28978332510292404 ) ) ;
#2517 = AXIS2_PLACEMENT_3D ( 'NONE', #16868, #29187, #24258 ) ;
#2518 = CIRCLE ( 'NONE', #5149, 12.36707279061065279 ) ;
#2519 = ORIENTED_EDGE ( 'NONE', *, *, #32257, .F. ) ;
#2520 = FACE_OUTER_BOUND ( 'NONE', #1517, .T. ) ;
#2521 = ORIENTED_EDGE ( 'NONE', *, *, #29812, .F. ) ;
#2522 = ADVANCED_FACE ( 'NONE', ( #21296 ), #8834, .F. ) ;
#2523 = ADVANCED_FACE ( 'NONE', ( #11948 ), #1607, .T. ) ;
#2524 = EDGE_CURVE ( 'NONE', #27647, #17361, #29345, .T. ) ;
#2525 = DIRECTION ( 'NONE',  ( -1.101824276508909887E-16, 1.000000000000000000, -0.000000000000000000 ) ) ;
#2526 = CARTESIAN_POINT ( 'NONE',  ( -9.883074696779189594, -5.935345006353231589, 107.4930705127871846 ) ) ;
#2527 = EDGE_CURVE ( 'NONE', #9420, #29931, #8567, .T. ) ;
#2528 = AXIS2_PLACEMENT_3D ( 'NONE', #22537, #27632, #25010 ) ;
#2529 = AXIS2_PLACEMENT_3D ( 'NONE', #19130, #19467, #9299 ) ;
#2530 = ORIENTED_EDGE ( 'NONE', *, *, #20490, .F. ) ;
#2531 = CARTESIAN_POINT ( 'NONE',  ( 45.96182992765471909, 15.77906836436399374, 44.82232689504101586 ) ) ;
#2532 = EDGE_LOOP ( 'NONE', ( #10022, #23605, #1532, #19365 ) ) ;
#2533 = AXIS2_PLACEMENT_3D ( 'NONE', #30091, #358, #7598 ) ;
#2534 = DIRECTION ( 'NONE',  ( -1.101824276508909887E-16, 1.000000000000000000, -0.000000000000000000 ) ) ;
#2535 = VECTOR ( 'NONE', #22077, 999.9999999999998863 ) ;
#2536 =( NAMED_UNIT ( * ) SI_UNIT ( $, .STERADIAN. ) SOLID_ANGLE_UNIT ( ) );
#2537 = VERTEX_POINT ( 'NONE', #18995 ) ;
#2538 = CARTESIAN_POINT ( 'NONE',  ( 71.64025509781936307, 8.185031362399408650, 75.36104810003064358 ) ) ;
#2539 = DIRECTION ( 'NONE',  ( -0.000000000000000000, -1.000000000000000000, 0.000000000000000000 ) ) ;
#2540 = CARTESIAN_POINT ( 'NONE',  ( 8.698509210239517842, 25.34164230456639899, 47.04930799450051637 ) ) ;
#2541 = DIRECTION ( 'NONE',  ( 0.000000000000000000, -0.2756373558169902815, -0.9612616959383214477 ) ) ;
#2542 = CIRCLE ( 'NONE', #20877, 55.68770647617149194 ) ;
#2543 = CARTESIAN_POINT ( 'NONE',  ( 21.09785597605719332, 17.56454579224779877, 47.04930799450051637 ) ) ;
#2544 = ORIENTED_EDGE ( 'NONE', *, *, #17977, .F. ) ;
#2545 = DIRECTION ( 'NONE',  ( 0.000000000000000000, 0.000000000000000000, -1.000000000000000000 ) ) ;
#2546 = CARTESIAN_POINT ( 'NONE',  ( 7.796071960694296976, 17.16474120167318418, 47.04930799450052348 ) ) ;
#2547 = EDGE_LOOP ( 'NONE', ( #24954, #30069, #15985, #23180 ) ) ;
#2548 = LINE ( 'NONE', #29481, #18243 ) ;
#2549 = DIRECTION ( 'NONE',  ( -1.000000000000000000, 0.000000000000000000, 0.000000000000000000 ) ) ;
#2550 = ORIENTED_EDGE ( 'NONE', *, *, #23423, .T. ) ;
#2551 = DIRECTION ( 'NONE',  ( 0.000000000000000000, -0.000000000000000000, -1.000000000000000000 ) ) ;
#2552 = ORIENTED_EDGE ( 'NONE', *, *, #25358, .T. ) ;
#2553 = EDGE_CURVE ( 'NONE', #1215, #16982, #10146, .T. ) ;
#2554 = EDGE_CURVE ( 'NONE', #15510, #16262, #29519, .T. ) ;
#2555 = VECTOR ( 'NONE', #21564, 1000.000000000000114 ) ;
#2556 = AXIS2_PLACEMENT_3D ( 'NONE', #29728, #17235, #27250 ) ;
#2557 = VERTEX_POINT ( 'NONE', #22112 ) ;
#2558 = CIRCLE ( 'NONE', #16691, 1.899999999999999023 ) ;
#2559 = CIRCLE ( 'NONE', #21396, 12.27641737965283397 ) ;
#2560 = DIRECTION ( 'NONE',  ( -1.000000000000000000, 0.000000000000000000, 0.000000000000000000 ) ) ;
#2561 = FACE_OUTER_BOUND ( 'NONE', #28539, .T. ) ;
#2562 = ADVANCED_FACE ( 'NONE', ( #24090 ), #6868, .F. ) ;
#2563 = ORIENTED_EDGE ( 'NONE', *, *, #21276, .T. ) ;
#2564 = ORIENTED_EDGE ( 'NONE', *, *, #1705, .T. ) ;
#2565 = CARTESIAN_POINT ( 'NONE',  ( 73.61977373202824992, 0.9814505390143158925, 14.24566699581558638 ) ) ;
#2566 = CARTESIAN_POINT ( 'NONE',  ( 42.05610609765635388, 11.92558985988972964, -5.593356398450009870 ) ) ;
#2567 = DIRECTION ( 'NONE',  ( 0.4544104193609917464, 0.000000000000000000, 0.8907924397839080966 ) ) ;
#2568 = DIRECTION ( 'NONE',  ( -1.000000000000000000, 0.000000000000000000, 0.000000000000000000 ) ) ;
#2569 = CARTESIAN_POINT ( 'NONE',  ( 21.09785597605719332, 14.56957104541719694, -7.455717258668906666 ) ) ;
#2570 = VERTEX_POINT ( 'NONE', #26557 ) ;
#2571 = CARTESIAN_POINT ( 'NONE',  ( -12.59080382683723442, -1.820484904611798349, 100.8496278133052897 ) ) ;
#2572 = EDGE_LOOP ( 'NONE', ( #24176, #17970, #898, #18395 ) ) ;
#2573 = DIRECTION ( 'NONE',  ( -1.000000000000000000, 0.000000000000000000, 0.000000000000000000 ) ) ;
#2574 = DIRECTION ( 'NONE',  ( -0.8746197071393926326, 0.4848096202463430537, 8.676864087101709653E-18 ) ) ;
#2575 = VECTOR ( 'NONE', #21813, 1000.000000000000227 ) ;
#2576 = EDGE_LOOP ( 'NONE', ( #56, #9669, #26047, #25845 ) ) ;
#2577 = CARTESIAN_POINT ( 'NONE',  ( -41.01929587258828747, 9.401204285752058354, 35.44930799450052206 ) ) ;
#2578 = DIRECTION ( 'NONE',  ( -1.000000000000000000, -1.101824276508909887E-16, 0.000000000000000000 ) ) ;
#2579 = CIRCLE ( 'NONE', #8852, 67.36417311134211161 ) ;
#2580 = DIRECTION ( 'NONE',  ( 0.000000000000000000, 0.000000000000000000, -1.000000000000000000 ) ) ;
#2581 = FACE_OUTER_BOUND ( 'NONE', #27056, .T. ) ;
#2582 = CARTESIAN_POINT ( 'NONE',  ( -40.90015969217747482, 8.955334253785162346, 57.95249952744806166 ) ) ;
#2583 = CARTESIAN_POINT ( 'NONE',  ( 49.49063479933183629, 28.01291119454915091, 47.17357720316391578 ) ) ;
#2584 = DIRECTION ( 'NONE',  ( -0.8746197071393925215, 0.4848096202463429982, 1.121857559391816958E-19 ) ) ;
#2585 = CARTESIAN_POINT ( 'NONE',  ( -40.64500813507293486, 6.819128862114092193, 39.51928662074344345 ) ) ;
#2586 = EDGE_CURVE ( 'NONE', #655, #6754, #17979, .T. ) ;
#2587 = ORIENTED_EDGE ( 'NONE', *, *, #29280, .T. ) ;
#2588 = DIRECTION ( 'NONE',  ( 0.000000000000000000, 0.000000000000000000, -1.000000000000000000 ) ) ;
#2589 = CARTESIAN_POINT ( 'NONE',  ( 8.732853799281734553, 38.56284415653841791, 47.04930799450051637 ) ) ;
#2590 = ORIENTED_EDGE ( 'NONE', *, *, #22060, .T. ) ;
#2591 = EDGE_CURVE ( 'NONE', #27103, #29537, #16694, .T. ) ;
#2592 = AXIS2_PLACEMENT_3D ( 'NONE', #13616, #19001, #31663 ) ;
#2593 = LINE ( 'NONE', #30336, #17952 ) ;
#2594 = ORIENTED_EDGE ( 'NONE', *, *, #13948, .T. ) ;
#2595 = TOROIDAL_SURFACE ( 'NONE', #29318, 58.88977237527051756, 0.5999999999999987566 ) ;
#2596 = ORIENTED_EDGE ( 'NONE', *, *, #6937, .F. ) ;
#2597 = DIRECTION ( 'NONE',  ( -0.4848096202463430537, -0.8746197071393926326, -9.920727850371701658E-18 ) ) ;
#2598 = EDGE_CURVE ( 'NONE', #23536, #19811, #3820, .T. ) ;
#2599 = EDGE_CURVE ( 'NONE', #17105, #11324, #6696, .T. ) ;
#2600 = ORIENTED_EDGE ( 'NONE', *, *, #17148, .F. ) ;
#2601 = AXIS2_PLACEMENT_3D ( 'NONE', #8776, #28810, #26832 ) ;
#2602 = CIRCLE ( 'NONE', #5211, 19.45967690998103805 ) ;
#2603 = ORIENTED_EDGE ( 'NONE', *, *, #17117, .F. ) ;
#2604 = CARTESIAN_POINT ( 'NONE',  ( 53.59785597605720397, 13.86454579224779948, 47.04930799450051637 ) ) ;
#2605 = EDGE_CURVE ( 'NONE', #30851, #31921, #18503, .T. ) ;
#2606 = AXIS2_PLACEMENT_3D ( 'NONE', #26812, #21379, #26644 ) ;
#2607 = ORIENTED_EDGE ( 'NONE', *, *, #8665, .T. ) ;
#2608 = DIRECTION ( 'NONE',  ( -0.000000000000000000, -1.000000000000000000, 0.000000000000000000 ) ) ;
#2609 = AXIS2_PLACEMENT_3D ( 'NONE', #9333, #24100, #29358 ) ;
#2610 = CARTESIAN_POINT ( 'NONE',  ( 21.09785597605720042, -13.87844638871996850, 47.04930799450051637 ) ) ;
#2611 = CARTESIAN_POINT ( 'NONE',  ( 49.06491948623858690, 22.86454579224779948, 46.50408568885027449 ) ) ;
#2612 = CARTESIAN_POINT ( 'NONE',  ( 47.20353132263855400, 28.90956182964375643, 45.01455027646041174 ) ) ;
#2613 = AXIS2_PLACEMENT_3D ( 'NONE', #25201, #15511, #27987 ) ;
#2614 = VERTEX_POINT ( 'NONE', #4241 ) ;
#2615 = ORIENTED_EDGE ( 'NONE', *, *, #2737, .F. ) ;
#2616 = DIRECTION ( 'NONE',  ( -1.000000000000000000, 0.000000000000000000, 0.000000000000000000 ) ) ;
#2617 = ORIENTED_EDGE ( 'NONE', *, *, #25045, .F. ) ;
#2618 = DIRECTION ( 'NONE',  ( -1.000000000000000000, 0.000000000000000000, 0.000000000000000000 ) ) ;
#2619 = CARTESIAN_POINT ( 'NONE',  ( 21.09785597605719332, 15.56454579224779877, -7.450692005499464088 ) ) ;
#2620 = CARTESIAN_POINT ( 'NONE',  ( -39.50554051497144314, 7.696103224718195968, 62.04930799450052348 ) ) ;
#2621 = DIRECTION ( 'NONE',  ( -1.000000000000000000, 0.000000000000000000, 0.000000000000000000 ) ) ;
#2622 = CARTESIAN_POINT ( 'NONE',  ( 21.09785597605720753, 17.36467600858027183, 47.04930799450052348 ) ) ;
#2623 = EDGE_CURVE ( 'NONE', #16795, #10074, #24416, .T. ) ;
#2624 = SHAPE_DEFINITION_REPRESENTATION ( #25040, #28161 ) ;
#2625 = ORIENTED_EDGE ( 'NONE', *, *, #12738, .F. ) ;
#2626 = ORIENTED_EDGE ( 'NONE', *, *, #122, .T. ) ;
#2627 = CARTESIAN_POINT ( 'NONE',  ( -42.70758099689500398, -0.7619956604996156457, 32.09930799450052064 ) ) ;
#2628 = CIRCLE ( 'NONE', #4190, 78.50000000000000000 ) ;
#2629 = DIRECTION ( 'NONE',  ( 0.000000000000000000, 0.000000000000000000, 1.000000000000000000 ) ) ;
#2630 = CIRCLE ( 'NONE', #11519, 0.1250000000000001110 ) ;
#2631 = EDGE_CURVE ( 'NONE', #3463, #27012, #9072, .T. ) ;
#2632 = FACE_OUTER_BOUND ( 'NONE', #29935, .T. ) ;
#2633 = ORIENTED_EDGE ( 'NONE', *, *, #5229, .F. ) ;
#2634 = CARTESIAN_POINT ( 'NONE',  ( 48.94625023931840246, 28.85784706826092716, 46.10640627770150246 ) ) ;
#2635 = ORIENTED_EDGE ( 'NONE', *, *, #31498, .F. ) ;
#2636 = DIRECTION ( 'NONE',  ( -1.000000000000000000, -1.101824276508909887E-16, 0.000000000000000000 ) ) ;
#2637 = DIRECTION ( 'NONE',  ( 0.4544104193609900810, 0.000000000000000000, 0.8907924397839089847 ) ) ;
#2638 = ADVANCED_FACE ( 'NONE', ( #11791 ), #1773, .F. ) ;
#2639 = CIRCLE ( 'NONE', #24632, 12.36707279061065101 ) ;
#2640 = CARTESIAN_POINT ( 'NONE',  ( -36.18493864628602807, 8.798967949527998655, 53.84930799450051353 ) ) ;
#2641 = EDGE_CURVE ( 'NONE', #13496, #21395, #7024, .T. ) ;
#2642 = CIRCLE ( 'NONE', #23062, 1.000000000000002220 ) ;
#2643 = CIRCLE ( 'NONE', #17, 1.300000000000002487 ) ;
#2644 = AXIS2_PLACEMENT_3D ( 'NONE', #17608, #7936, #28271 ) ;
#2645 = VERTEX_POINT ( 'NONE', #32144 ) ;
#2646 = ORIENTED_EDGE ( 'NONE', *, *, #3109, .T. ) ;
#2647 = DIRECTION ( 'NONE',  ( -1.101824276508909887E-16, 1.000000000000000000, -0.000000000000000000 ) ) ;
#2648 = CARTESIAN_POINT ( 'NONE',  ( -41.74033427429298371, 15.41509661078533355, 38.54930799450052348 ) ) ;
#2649 = CARTESIAN_POINT ( 'NONE',  ( 45.24946171279598417, 25.70784706826093569, 47.99220971130007030 ) ) ;
#2650 = AXIS2_PLACEMENT_3D ( 'NONE', #6932, #27605, #24486 ) ;
#2651 = ORIENTED_EDGE ( 'NONE', *, *, #31061, .T. ) ;
#2652 = CARTESIAN_POINT ( 'NONE',  ( 21.09785597605720753, 14.66454579224780019, 47.04930799450052348 ) ) ;
#2653 = CARTESIAN_POINT ( 'NONE',  ( 21.09785597605720753, -13.40182760052194588, 102.8325207889781439 ) ) ;
#2654 = CARTESIAN_POINT ( 'NONE',  ( 47.63716429968716426, 26.21960992152948577, 49.58068632438585865 ) ) ;
#2655 = CIRCLE ( 'NONE', #5803, 0.7000000000000061728 ) ;
#2656 = CYLINDRICAL_SURFACE ( 'NONE', #5032, 12.62506659569710266 ) ;
#2657 = CARTESIAN_POINT ( 'NONE',  ( -10.40214402394279425, 13.86454579224779948, 47.04930799450052348 ) ) ;
#2658 = FACE_OUTER_BOUND ( 'NONE', #25338, .T. ) ;
#2659 = CYLINDRICAL_SURFACE ( 'NONE', #29429, 0.1000000000000028644 ) ;
#2660 = FACE_OUTER_BOUND ( 'NONE', #20395, .T. ) ;
#2661 = AXIS2_PLACEMENT_3D ( 'NONE', #11338, #26104, #23330 ) ;
#2662 = CARTESIAN_POINT ( 'NONE',  ( 41.51205063648687599, 11.92558985988973497, 99.04321908912902472 ) ) ;
#2663 = EDGE_CURVE ( 'NONE', #1880, #18016, #6540, .T. ) ;
#2664 = DIRECTION ( 'NONE',  ( -0.7141240004913222972, 0.3958453973320028019, -0.5773502691896303940 ) ) ;
#2665 = AXIS2_PLACEMENT_3D ( 'NONE', #20127, #7170, #17167 ) ;
#2666 = ORIENTED_EDGE ( 'NONE', *, *, #22445, .F. ) ;
#2667 = ORIENTED_EDGE ( 'NONE', *, *, #32219, .F. ) ;
#2668 = DIRECTION ( 'NONE',  ( 0.000000000000000000, 0.000000000000000000, -1.000000000000000000 ) ) ;
#2669 = CIRCLE ( 'NONE', #23099, 0.1000000000000018235 ) ;
#2670 = CARTESIAN_POINT ( 'NONE',  ( 21.09992658989239089, 24.09164230456639544, 47.04930799450051637 ) ) ;
#2671 = DIRECTION ( 'NONE',  ( 0.000000000000000000, -1.000000000000000000, 0.000000000000000000 ) ) ;
#2672 = CARTESIAN_POINT ( 'NONE',  ( 54.82737574693081939, -2.284241381456145970, 101.1271600646791029 ) ) ;
#2673 = ORIENTED_EDGE ( 'NONE', *, *, #22568, .T. ) ;
#2674 = FACE_OUTER_BOUND ( 'NONE', #2355, .T. ) ;
#2675 = DIRECTION ( 'NONE',  ( 9.242526717056601033E-17, -0.6560590289905074979, 0.7547095802227717920 ) ) ;
#2676 = CARTESIAN_POINT ( 'NONE',  ( 49.09785597605721108, 14.86454579224779948, 47.04930799450052348 ) ) ;
#2677 = ORIENTED_EDGE ( 'NONE', *, *, #17420, .F. ) ;
#2678 = ORIENTED_EDGE ( 'NONE', *, *, #2248, .F. ) ;
#2679 = CARTESIAN_POINT ( 'NONE',  ( -40.65762574042817334, 9.591092754368338191, 35.59072935073783128 ) ) ;
#2680 = CARTESIAN_POINT ( 'NONE',  ( 46.00908685603034343, 26.93284706826093355, 44.91496614357595263 ) ) ;
#2681 = AXIS2_PLACEMENT_3D ( 'NONE', #3297, #30398, #3129 ) ;
#2682 = FACE_OUTER_BOUND ( 'NONE', #28319, .T. ) ;
#2683 = EDGE_CURVE ( 'NONE', #5958, #20704, #12223, .T. ) ;
#2684 = FACE_OUTER_BOUND ( 'NONE', #6076, .T. ) ;
#2685 = B_SPLINE_CURVE_WITH_KNOTS ( 'NONE', 3,
 ( #29665, #11936, #4547, #4713, #21932, #14733, #2251, #14563, #12271, #5374, #25228, #27525, #8157, #14894, #432, #12600, #30316, #15532, #5203, #10457, #2571, #5046, #15054, #22419, #20129, #2739, #15377, #30486, #18147, #13086, #12435, #32454, #15213, #9966, #29995, #7830 ),
 .UNSPECIFIED., .F., .F.,
 ( 4, 2, 2, 2, 2, 2, 2, 2, 2, 2, 2, 2, 2, 2, 2, 2, 2, 4 ),
 ( 0.000000000000000000, 0.001327013081135473057, 0.002654026162270946114, 0.003981039243406417003, 0.005308052324541888758, 0.006635065405677360514, 0.007962078486812830536, 0.01061610464908377231, 0.01194311773021923886, 0.01327013081135470368, 0.01459714389249017023, 0.01592415697362563679, 0.01725117005476110160, 0.01857818313589656642, 0.01924168967646430056, 0.01990519621703203124, 0.02056870275759976191, 0.02123220929816749258 ),
 .UNSPECIFIED. ) ;
#2686 = ORIENTED_EDGE ( 'NONE', *, *, #28464, .F. ) ;
#2687 = CIRCLE ( 'NONE', #21013, 0.9999999999999978906 ) ;
#2688 = AXIS2_PLACEMENT_3D ( 'NONE', #14002, #16605, #1681 ) ;
#2689 = CARTESIAN_POINT ( 'NONE',  ( 21.09785597605719332, 14.77459629858661572, 101.3493079945005206 ) ) ;
#2690 = TOROIDAL_SURFACE ( 'NONE', #18398, 15.35463912851480828, 0.6621856154243856984 ) ;
#2691 = ORIENTED_EDGE ( 'NONE', *, *, #8934, .F. ) ;
#2692 = LINE ( 'NONE', #10251, #6619 ) ;
#2693 = CARTESIAN_POINT ( 'NONE',  ( -42.50976151518962354, 14.59907569580870224, 38.19144330556764544 ) ) ;
#2694 = AXIS2_PLACEMENT_3D ( 'NONE', #20538, #32372, #7590 ) ;
#2695 = ORIENTED_EDGE ( 'NONE', *, *, #16677, .F. ) ;
#2696 = CARTESIAN_POINT ( 'NONE',  ( -40.80566404189690388, 8.441333990788717045, 34.56793150177820451 ) ) ;
#2697 = VERTEX_POINT ( 'NONE', #2585 ) ;
#2698 = DIRECTION ( 'NONE',  ( -1.101824276508909887E-16, 1.000000000000000000, -0.000000000000000000 ) ) ;
#2699 = LINE ( 'NONE', #15019, #27764 ) ;
#2700 = CARTESIAN_POINT ( 'NONE',  ( -39.52978099598376360, 7.652372239361226569, 32.09930799450052064 ) ) ;
#2701 = CARTESIAN_POINT ( 'NONE',  ( -39.67555847965937943, 2.645252416024337361, 47.04930799450051637 ) ) ;
#2702 = ORIENTED_EDGE ( 'NONE', *, *, #9200, .T. ) ;
#2703 = CARTESIAN_POINT ( 'NONE',  ( 71.55760889374487022, 9.126991894476596201, 74.42996348956144459 ) ) ;
#2704 = DIRECTION ( 'NONE',  ( 0.2072038891212098777, -0.4540212254542328463, -0.8665629089512670857 ) ) ;
#2705 = DIRECTION ( 'NONE',  ( -1.000000000000000000, 0.000000000000000000, 0.000000000000000000 ) ) ;
#2706 = LINE ( 'NONE', #10754, #31338 ) ;
#2707 = VECTOR ( 'NONE', #8596, 1000.000000000000000 ) ;
#2708 = FACE_OUTER_BOUND ( 'NONE', #13436, .T. ) ;
#2709 = ORIENTED_EDGE ( 'NONE', *, *, #12911, .F. ) ;
#2710 = VECTOR ( 'NONE', #28353, 1000.000000000000000 ) ;
#2711 = CARTESIAN_POINT ( 'NONE',  ( 21.09992658989238734, 32.09164230456639899, 47.04930799450051637 ) ) ;
#2712 = DIRECTION ( 'NONE',  ( 0.000000000000000000, 0.000000000000000000, 1.000000000000000000 ) ) ;
#2713 = ORIENTED_EDGE ( 'NONE', *, *, #4530, .T. ) ;
#2714 = DIRECTION ( 'NONE',  ( -1.101824276508909887E-16, 1.000000000000000000, -0.000000000000000000 ) ) ;
#2715 = CARTESIAN_POINT ( 'NONE',  ( 21.09785597605719332, -19.93545420775220123, 47.04930799450051637 ) ) ;
#2716 = EDGE_CURVE ( 'NONE', #32455, #14337, #8035, .T. ) ;
#2717 = CARTESIAN_POINT ( 'NONE',  ( 8.482002859293443109, 28.46664230456639899, 47.04930799450051637 ) ) ;
#2718 = EDGE_CURVE ( 'NONE', #14523, #2027, #20604, .T. ) ;
#2719 = EDGE_CURVE ( 'NONE', #26808, #16648, #7355, .T. ) ;
#2720 = ORIENTED_EDGE ( 'NONE', *, *, #10034, .F. ) ;
#2721 = EDGE_CURVE ( 'NONE', #12417, #12904, #1756, .T. ) ;
#2722 = CARTESIAN_POINT ( 'NONE',  ( -40.46271621608484281, 3.081581074246044327, 32.14930799450051779 ) ) ;
#2723 = ORIENTED_EDGE ( 'NONE', *, *, #27198, .F. ) ;
#2724 = EDGE_CURVE ( 'NONE', #11490, #28677, #15920, .T. ) ;
#2725 = CIRCLE ( 'NONE', #15306, 0.1000000000000014905 ) ;
#2726 = VERTEX_POINT ( 'NONE', #25241 ) ;
#2727 = TOROIDAL_SURFACE ( 'NONE', #20011, 46.53489018157424084, 0.7000000000000002887 ) ;
#2728 = AXIS2_PLACEMENT_3D ( 'NONE', #2225, #14868, #27825 ) ;
#2729 = DIRECTION ( 'NONE',  ( -0.4848096202463430537, -0.8746197071393926326, -9.920727850371701658E-18 ) ) ;
#2730 = CARTESIAN_POINT ( 'NONE',  ( 47.63716429968715715, 26.09696019071910200, 49.58068632438583734 ) ) ;
#2731 = ORIENTED_EDGE ( 'NONE', *, *, #27073, .F. ) ;
#2732 = VERTEX_POINT ( 'NONE', #19810 ) ;
#2733 = CARTESIAN_POINT ( 'NONE',  ( 43.69587290534151691, 11.69997306056223607, -5.046785234866655756 ) ) ;
#2734 = CARTESIAN_POINT ( 'NONE',  ( -5.602943079677954685, 9.702389020015065313, 98.41455612196619995 ) ) ;
#2735 = CARTESIAN_POINT ( 'NONE',  ( -30.56895382951262619, 7.047361869319173522, 76.28100816727524602 ) ) ;
#2736 = DIRECTION ( 'NONE',  ( 0.000000000000000000, -0.000000000000000000, -1.000000000000000000 ) ) ;
#2737 = EDGE_CURVE ( 'NONE', #5504, #27500, #14879, .T. ) ;
#2738 = EDGE_LOOP ( 'NONE', ( #24640, #20713, #687, #12474 ) ) ;
#2739 = CARTESIAN_POINT ( 'NONE',  ( -12.07837398813756913, -4.576799740321095378, 102.9520008778022913 ) ) ;
#2740 = ORIENTED_EDGE ( 'NONE', *, *, #4168, .F. ) ;
#2741 = CARTESIAN_POINT ( 'NONE',  ( 21.09785597605720753, 14.86454579224779948, 47.04930799450052348 ) ) ;
#2742 = DIRECTION ( 'NONE',  ( 1.000000000000000000, 0.000000000000000000, 0.000000000000000000 ) ) ;
#2743 = AXIS2_PLACEMENT_3D ( 'NONE', #26516, #21579, #8482 ) ;
#2744 = EDGE_LOOP ( 'NONE', ( #13844, #8496 ) ) ;
#2745 = DIRECTION ( 'NONE',  ( -0.000000000000000000, -1.000000000000000000, -0.000000000000000000 ) ) ;
#2746 = DIRECTION ( 'NONE',  ( -0.2743622330404226206, 0.9568148143496237878, 0.09607692814702083195 ) ) ;
#2747 = CARTESIAN_POINT ( 'NONE',  ( 81.71508932399986236, -5.936918531481694572, 15.99626209184008552 ) ) ;
#2748 = CARTESIAN_POINT ( 'NONE',  ( -40.52669582637187773, 7.652910973922034010, 53.94439779120588696 ) ) ;
#2749 = CARTESIAN_POINT ( 'NONE',  ( 61.09785597605721108, 14.86454579224779948, 47.04930799450051637 ) ) ;
#2750 = AXIS2_PLACEMENT_3D ( 'NONE', #4589, #14614, #21976 ) ;
#2751 = CARTESIAN_POINT ( 'NONE',  ( 48.94625023931840957, 26.67124452788248945, 46.10640627770150246 ) ) ;
#2752 = DIRECTION ( 'NONE',  ( -0.000000000000000000, -1.000000000000000000, 0.000000000000000000 ) ) ;
#2753 = CARTESIAN_POINT ( 'NONE',  ( -40.13606231985500017, 7.635531802539801127, 60.29072935073781991 ) ) ;
#2754 = VERTEX_POINT ( 'NONE', #2753 ) ;
#2755 = CYLINDRICAL_SURFACE ( 'NONE', #17209, 2.500000000000002220 ) ;
#2756 = VERTEX_POINT ( 'NONE', #30009 ) ;
#2757 = AXIS2_PLACEMENT_3D ( 'NONE', #29874, #7390, #17384 ) ;
#2758 = CARTESIAN_POINT ( 'NONE',  ( -40.80097511801616150, 8.246641009394465982, 59.64930799450051779 ) ) ;
#2759 = EDGE_LOOP ( 'NONE', ( #15121, #5548, #3395, #3205 ) ) ;
#2760 = ADVANCED_FACE ( 'NONE', ( #30173 ), #14907, .F. ) ;
#2761 = AXIS2_PLACEMENT_3D ( 'NONE', #6066, #31179, #31334 ) ;
#2762 = ORIENTED_EDGE ( 'NONE', *, *, #1929, .F. ) ;
#2763 = EDGE_CURVE ( 'NONE', #2915, #32455, #17494, .T. ) ;
#2764 = ORIENTED_EDGE ( 'NONE', *, *, #2763, .T. ) ;
#2765 = AXIS2_PLACEMENT_3D ( 'NONE', #6248, #21011, #30882 ) ;
#2766 = B_SPLINE_SURFACE_WITH_KNOTS ( 'NONE', 3, 3, ( 
 ( #18342, #13593, #31313, #10819, #31155, #18178 ),
 ( #21281, #11290, #13442, #18501, #23753, #18659 ),
 ( #28531, #28205, #6195, #11138, #6048, #23597 ),
 ( #16047, #10973, #8814, #1109, #13287, #1259 ),
 ( #8668, #5722, #25743, #26217, #3252, #30833 ),
 ( #21119, #28373, #5563, #15727, #20652, #13118 ) ),
 .UNSPECIFIED., .F., .F., .F.,
 ( 4, 2, 4 ),
 ( 4, 2, 4 ),
 ( 0.000000000000000000, 0.5000000000000000000, 1.000000000000000000 ),
 ( 0.000000000000000000, 0.5000000000000000000, 1.000000000000000000 ),
 .UNSPECIFIED. ) ;
#2767 = EDGE_LOOP ( 'NONE', ( #14506, #267, #22597, #1671 ) ) ;
#2768 = VECTOR ( 'NONE', #3452, 1000.000000000000114 ) ;
#2769 = CARTESIAN_POINT ( 'NONE',  ( 46.52714753771119405, 23.10527865767145173, 47.18627808671003265 ) ) ;
#2770 = EDGE_CURVE ( 'NONE', #7874, #11316, #29009, .T. ) ;
#2771 = ORIENTED_EDGE ( 'NONE', *, *, #6793, .F. ) ;
#2772 = SURFACE_STYLE_USAGE ( .BOTH. , #22626 ) ;
#2773 = CIRCLE ( 'NONE', #30032, 12.36707279061065101 ) ;
#2774 = DIRECTION ( 'NONE',  ( -1.169615070119510171E-16, -0.2964022880492104273, -0.9550631830613055540 ) ) ;
#2775 = CARTESIAN_POINT ( 'NONE',  ( 48.89639543821420631, 22.86454579224779948, 46.17372366037167097 ) ) ;
#2776 = CARTESIAN_POINT ( 'NONE',  ( 45.24946171279598417, 26.32124452788248803, 47.99220971130007030 ) ) ;
#2777 = ADVANCED_FACE ( 'NONE', ( #12782 ), #28025, .T. ) ;
#2778 = ORIENTED_EDGE ( 'NONE', *, *, #15032, .F. ) ;
#2779 = ORIENTED_EDGE ( 'NONE', *, *, #14759, .F. ) ;
#2780 = EDGE_CURVE ( 'NONE', #9753, #22946, #5965, .T. ) ;
#2781 = ORIENTED_EDGE ( 'NONE', *, *, #809, .F. ) ;
#2782 = DIRECTION ( 'NONE',  ( -1.000000000000000000, 0.000000000000000000, 0.000000000000000000 ) ) ;
#2783 = CARTESIAN_POINT ( 'NONE',  ( 54.63702927177264002, -3.812314126620138577, 103.1735800200605553 ) ) ;
#2784 = FACE_OUTER_BOUND ( 'NONE', #1292, .T. ) ;
#2785 = LINE ( 'NONE', #15421, #22569 ) ;
#2786 = DIRECTION ( 'NONE',  ( -1.000000000000000000, 0.000000000000000000, 0.000000000000000000 ) ) ;
#2787 = SHAPE_DEFINITION_REPRESENTATION ( #24763, #11371 ) ;
#2788 = ORIENTED_EDGE ( 'NONE', *, *, #19743, .T. ) ;
#2789 = VERTEX_POINT ( 'NONE', #27696 ) ;
#2790 = DIRECTION ( 'NONE',  ( -1.000000000000000000, 0.000000000000000000, -1.110223024625155594E-14 ) ) ;
#2791 = CARTESIAN_POINT ( 'NONE',  ( 47.63716429968716426, 29.01960992152946872, 49.58068632438585155 ) ) ;
#2792 = TOROIDAL_SURFACE ( 'NONE', #20079, 12.40141737965285529, 0.1250000000000000555 ) ;
#2793 = CARTESIAN_POINT ( 'NONE',  ( 48.94625023931840246, 29.55784706826092645, 46.10640627770150246 ) ) ;
#2794 = CONICAL_SURFACE ( 'NONE', #6443, 1.799999999999998490, 0.7853981633974489451 ) ;
#2795 = EDGE_LOOP ( 'NONE', ( #424, #16242, #2877, #20423 ) ) ;
#2796 = FACE_OUTER_BOUND ( 'NONE', #7289, .T. ) ;
#2797 = EDGE_CURVE ( 'NONE', #21972, #16102, #21675, .T. ) ;
#2798 = DIRECTION ( 'NONE',  ( 0.9612616959383193382, 0.2756373558169973870, 8.795445018804928853E-19 ) ) ;
#2799 = AXIS2_PLACEMENT_3D ( 'NONE', #31420, #14187, #2026 ) ;
#2800 = AXIS2_PLACEMENT_3D ( 'NONE', #1931, #21944, #9653 ) ;
#2801 = ORIENTED_EDGE ( 'NONE', *, *, #13825, .F. ) ;
#2802 = ORIENTED_EDGE ( 'NONE', *, *, #4971, .T. ) ;
#2803 = EDGE_CURVE ( 'NONE', #20430, #16795, #25880, .T. ) ;
#2804 = FACE_OUTER_BOUND ( 'NONE', #22909, .T. ) ;
#2805 = CARTESIAN_POINT ( 'NONE',  ( -42.47434154250543514, 4.196643200812633978, 35.14930799450051779 ) ) ;
#2806 = EDGE_CURVE ( 'NONE', #1340, #8773, #10695, .T. ) ;
#2807 = ORIENTED_EDGE ( 'NONE', *, *, #22162, .F. ) ;
#2808 = DIRECTION ( 'NONE',  ( -0.2756373558169956106, 0.9612616959383197823, 0.000000000000000000 ) ) ;
#2809 = FACE_OUTER_BOUND ( 'NONE', #30576, .T. ) ;
#2810 = CARTESIAN_POINT ( 'NONE',  ( -41.96544240928614755, 13.75880317176705603, 54.54930799450051637 ) ) ;
#2811 = EDGE_CURVE ( 'NONE', #2027, #26330, #3850, .T. ) ;
#2812 = CARTESIAN_POINT ( 'NONE',  ( 52.12585496443453081, -5.943281723642242831, -10.93395394839392587 ) ) ;
#2813 = EDGE_CURVE ( 'NONE', #26531, #27840, #30084, .T. ) ;
#2814 = EDGE_CURVE ( 'NONE', #4198, #16034, #19041, .T. ) ;
#2815 = DIRECTION ( 'NONE',  ( 0.000000000000000000, 0.000000000000000000, -1.000000000000000000 ) ) ;
#2816 = AXIS2_PLACEMENT_3D ( 'NONE', #19771, #27826, #2226 ) ;
#2817 = CARTESIAN_POINT ( 'NONE',  ( 45.41164638504195494, 22.93807716476589675, 46.96173444154113241 ) ) ;
#2818 = CARTESIAN_POINT ( 'NONE',  ( 21.09992658989239089, 29.09164230456639899, 47.04930799450051637 ) ) ;
#2819 = VECTOR ( 'NONE', #3476, 1000.000000000000000 ) ;
#2820 = DIRECTION ( 'NONE',  ( -2.779292025043186357E-18, 1.288349127009862211E-17, -1.000000000000000000 ) ) ;
#2821 = CARTESIAN_POINT ( 'NONE',  ( 49.41945501136223839, 29.16454579807170688, 45.86501535757901848 ) ) ;
#2822 = EDGE_LOOP ( 'NONE', ( #10818, #13643, #14022, #11285 ) ) ;
#2823 = ORIENTED_EDGE ( 'NONE', *, *, #22749, .T. ) ;
#2824 = DIRECTION ( 'NONE',  ( -0.000000000000000000, -1.000000000000000000, 0.000000000000000000 ) ) ;
#2825 = CARTESIAN_POINT ( 'NONE',  ( -31.67509402814005881, 0.3087484226586330038, 13.94399873050154781 ) ) ;
#2826 = CARTESIAN_POINT ( 'NONE',  ( 53.37090610332811025, 2.112486173643655096, 99.16308969199836554 ) ) ;
#2827 = ORIENTED_EDGE ( 'NONE', *, *, #23066, .F. ) ;
#2828 = CARTESIAN_POINT ( 'NONE',  ( -39.67555847965937943, 2.645252416024337361, 47.04930799450051637 ) ) ;
#2829 = CARTESIAN_POINT ( 'NONE',  ( 33.72499318558949000, 38.56284415653841791, 47.04930799450051637 ) ) ;
#2830 = VERTEX_POINT ( 'NONE', #4894 ) ;
#2831 = VERTEX_POINT ( 'NONE', #22605 ) ;
#2832 = CARTESIAN_POINT ( 'NONE',  ( -42.38263560350583248, 14.61917486843862868, 53.54930799450051637 ) ) ;
#2833 = CARTESIAN_POINT ( 'NONE',  ( 45.35708200440645044, 26.29118040159426428, 45.92000246470679770 ) ) ;
#2834 = EDGE_CURVE ( 'NONE', #15810, #12910, #13422, .T. ) ;
#2835 = DIRECTION ( 'NONE',  ( -2.779292025043186357E-18, 1.288349127009862211E-17, -1.000000000000000000 ) ) ;
#2836 = CARTESIAN_POINT ( 'NONE',  ( 21.09992658989239089, 26.84143805560860940, 47.04930799450051637 ) ) ;
#2837 = CIRCLE ( 'NONE', #31726, 1.700000000000000178 ) ;
#2838 = DIRECTION ( 'NONE',  ( -1.101824276508909887E-16, 1.000000000000000000, -0.000000000000000000 ) ) ;
#2839 = ORIENTED_EDGE ( 'NONE', *, *, #30504, .T. ) ;
#2840 = EDGE_CURVE ( 'NONE', #1796, #6385, #12255, .T. ) ;
#2841 = CARTESIAN_POINT ( 'NONE',  ( -22.40214402394279247, 14.86454579224779948, 47.04930799450052348 ) ) ;
#2842 = ADVANCED_FACE ( 'NONE', ( #8323 ), #11567, .T. ) ;
#2843 = ORIENTED_EDGE ( 'NONE', *, *, #18427, .F. ) ;
#2844 = DIRECTION ( 'NONE',  ( 2.779292025043186357E-18, -1.288349127009862057E-17, 1.000000000000000000 ) ) ;
#2845 = DIRECTION ( 'NONE',  ( -0.2756373558169932236, 0.9612616959383205595, -1.479773560108267395E-16 ) ) ;
#2846 = EDGE_CURVE ( 'NONE', #11299, #8773, #3328, .T. ) ;
#2847 = EDGE_LOOP ( 'NONE', ( #18759, #30686 ) ) ;
#2848 = CARTESIAN_POINT ( 'NONE',  ( -40.85259535153578270, 8.476421318711492958, 34.61707255558062002 ) ) ;
#2849 = ORIENTED_EDGE ( 'NONE', *, *, #4751, .F. ) ;
#2850 = EDGE_CURVE ( 'NONE', #1764, #2499, #23259, .T. ) ;
#2851 = DIRECTION ( 'NONE',  ( -1.000000000000000000, 0.000000000000000000, 0.000000000000000000 ) ) ;
#2852 = DIRECTION ( 'NONE',  ( 0.000000000000000000, 0.000000000000000000, -1.000000000000000000 ) ) ;
#2853 = AXIS2_PLACEMENT_3D ( 'NONE', #13835, #23830, #29087 ) ;
#2854 = VECTOR ( 'NONE', #1638, 999.9999999999997726 ) ;
#2855 = CARTESIAN_POINT ( 'NONE',  ( -0.4058007941739975033, 11.88152873911358753, 99.49782616222140064 ) ) ;
#2856 = AXIS2_PLACEMENT_3D ( 'NONE', #24398, #17003, #21928 ) ;
#2857 = DIRECTION ( 'NONE',  ( 0.000000000000000000, -1.000000000000000000, 0.000000000000000000 ) ) ;
#2858 = VERTEX_POINT ( 'NONE', #5699 ) ;
#2859 = DIRECTION ( 'NONE',  ( -1.101824276508909887E-16, 1.000000000000000000, -0.000000000000000000 ) ) ;
#2860 = FACE_OUTER_BOUND ( 'NONE', #25007, .T. ) ;
#2861 = AXIS2_PLACEMENT_3D ( 'NONE', #25544, #273, #20453 ) ;
#2862 = AXIS2_PLACEMENT_3D ( 'NONE', #4608, #7241, #12334 ) ;
#2863 = DIRECTION ( 'NONE',  ( -0.8907924397839087627, -1.100109291107994187E-16, 0.4544104193609907472 ) ) ;
#2864 = CARTESIAN_POINT ( 'NONE',  ( -40.47970302497625994, 7.463434137431151250, 53.54930799450051637 ) ) ;
#2865 = VECTOR ( 'NONE', #14637, 1000.000000000000114 ) ;
#2866 = DIRECTION ( 'NONE',  ( -0.8746197071393926326, 0.4848096202463430537, 8.676864087101709653E-18 ) ) ;
#2867 = ORIENTED_EDGE ( 'NONE', *, *, #8743, .T. ) ;
#2868 = DIRECTION ( 'NONE',  ( -1.224646799147353207E-16, 0.000000000000000000, -1.000000000000000000 ) ) ;
#2869 = FACE_OUTER_BOUND ( 'NONE', #1078, .T. ) ;
#2870 = ORIENTED_EDGE ( 'NONE', *, *, #30114, .F. ) ;
#2871 = CARTESIAN_POINT ( 'NONE',  ( -10.30158825675060008, -5.900224301042254815, -12.20999419125749696 ) ) ;
#2872 = CARTESIAN_POINT ( 'NONE',  ( -45.72330504332163059, -5.935454207752205669, 40.04930799450050216 ) ) ;
#2873 = CARTESIAN_POINT ( 'NONE',  ( -38.57628410747783221, -5.935454207752202116, 16.07118271501078866 ) ) ;
#2874 = DIRECTION ( 'NONE',  ( -1.224646799147353207E-16, -1.349345573449484691E-32, 1.000000000000000000 ) ) ;
#2875 = ORIENTED_EDGE ( 'NONE', *, *, #7120, .T. ) ;
#2876 = DIRECTION ( 'NONE',  ( -1.224646799147353207E-16, 0.000000000000000000, -1.000000000000000000 ) ) ;
#2877 = ORIENTED_EDGE ( 'NONE', *, *, #19461, .F. ) ;
#2878 = PRODUCT_DEFINITION_CONTEXT ( 'detailed design', #25444, 'design' ) ;
#2879 = ORIENTED_EDGE ( 'NONE', *, *, #8848, .F. ) ;
#2880 = VECTOR ( 'NONE', #12997, 1000.000000000000000 ) ;
#2881 = AXIS2_PLACEMENT_3D ( 'NONE', #2172, #32370, #4960 ) ;
#2882 = B_SPLINE_CURVE_WITH_KNOTS ( 'NONE', 3,
 ( #12590, #422, #15365, #9514, #20119, #23068, #25534, #8147, #30150, #7818, #20275, #20441 ),
 .UNSPECIFIED., .F., .F.,
 ( 4, 2, 2, 2, 2, 4 ),
 ( 0.0003195369756189209219, 0.0003994212195236353908, 0.0004793054634283499139, 0.0005192475853807071483, 0.0005591897073330643828, 0.0006390739512378048725 ),
 .UNSPECIFIED. ) ;
#2883 = AXIS2_PLACEMENT_3D ( 'NONE', #16494, #14042, #31765 ) ;
#2884 = AXIS2_PLACEMENT_3D ( 'NONE', #22880, #3008, #5170 ) ;
#2885 = AXIS2_PLACEMENT_3D ( 'NONE', #29205, #24766, #14765 ) ;
#2886 = CARTESIAN_POINT ( 'NONE',  ( 21.09785597605719332, -9.935454207752199451, 118.3493079945004922 ) ) ;
#2887 = CARTESIAN_POINT ( 'NONE',  ( 48.23388202445966755, 26.82822092656774515, 49.27628909396054979 ) ) ;
#2888 = ADVANCED_FACE ( 'NONE', ( #15704 ), #27450, .T. ) ;
#2889 = VERTEX_POINT ( 'NONE', #23261 ) ;
#2890 = EDGE_LOOP ( 'NONE', ( #24943, #20819, #3048, #15004 ) ) ;
#2891 = ADVANCED_FACE ( 'NONE', ( #773 ), #3548, .T. ) ;
#2892 = CARTESIAN_POINT ( 'NONE',  ( -44.02786950842664027, -5.204346380200058242, 52.49783445483662803 ) ) ;
#2893 = FACE_BOUND ( 'NONE', #21626, .T. ) ;
#2894 = DIRECTION ( 'NONE',  ( -1.101824276508909887E-16, 1.000000000000000000, -0.000000000000000000 ) ) ;
#2895 = CARTESIAN_POINT ( 'NONE',  ( 8.482002859293450214, 29.21664230456640254, 47.04930799450051637 ) ) ;
#2896 = EDGE_LOOP ( 'NONE', ( #10191, #14250, #4824, #25229 ) ) ;
#2897 = DIRECTION ( 'NONE',  ( 0.000000000000000000, 0.000000000000000000, -1.000000000000000000 ) ) ;
#2898 = VERTEX_POINT ( 'NONE', #8649 ) ;
#2899 = DIRECTION ( 'NONE',  ( 1.000000000000000000, 0.000000000000000000, 0.000000000000000000 ) ) ;
#2900 = CARTESIAN_POINT ( 'NONE',  ( -41.13156850465621517, 9.429949956619452678, 35.64930799450052490 ) ) ;
#2901 = EDGE_LOOP ( 'NONE', ( #29208, #11999, #12158, #28052 ) ) ;
#2902 = CARTESIAN_POINT ( 'NONE',  ( 47.86364407361583062, 22.99884124225578930, 45.86888002329718717 ) ) ;
#2903 = CARTESIAN_POINT ( 'NONE',  ( -35.22851096958370221, 11.86391768464652152, 53.48664131055646465 ) ) ;
#2904 = DIRECTION ( 'NONE',  ( -2.779292025043186357E-18, 1.288349127009862211E-17, -1.000000000000000000 ) ) ;
#2905 = CARTESIAN_POINT ( 'NONE',  ( 46.99023568444673060, 27.13791119454915446, 49.12151524109405898 ) ) ;
#2906 = AXIS2_PLACEMENT_3D ( 'NONE', #9143, #13758, #18812 ) ;
#2907 = CARTESIAN_POINT ( 'NONE',  ( -40.06561427811386267, 7.496110634155836117, 54.64930799450051779 ) ) ;
#2908 = DIRECTION ( 'NONE',  ( -1.000000000000000000, 0.000000000000000000, 0.000000000000000000 ) ) ;
#2909 = CIRCLE ( 'NONE', #25448, 94.44530576803552435 ) ;
#2910 = ORIENTED_EDGE ( 'NONE', *, *, #17751, .F. ) ;
#2911 = CARTESIAN_POINT ( 'NONE',  ( 21.09992658989239089, 26.34143805560860940, 47.04930799450051637 ) ) ;
#2912 = EDGE_LOOP ( 'NONE', ( #31676, #1868, #13955, #3623 ) ) ;
#2913 = AXIS2_PLACEMENT_3D ( 'NONE', #230, #17624, #17784 ) ;
#2914 = DIRECTION ( 'NONE',  ( -0.2756373558170082672, 0.9612616959383162296, 0.000000000000000000 ) ) ;
#2915 = VERTEX_POINT ( 'NONE', #18638 ) ;
#2916 = ORIENTED_EDGE ( 'NONE', *, *, #5389, .T. ) ;
#2917 = CARTESIAN_POINT ( 'NONE',  ( 21.09992658989238734, 38.56284415653841791, 47.04930799450051637 ) ) ;
#2918 = VECTOR ( 'NONE', #6397, 1000.000000000000000 ) ;
#2919 = ORIENTED_EDGE ( 'NONE', *, *, #12849, .T. ) ;
#2920 = EDGE_LOOP ( 'NONE', ( #13323, #6461, #20434, #8177 ) ) ;
#2921 = CARTESIAN_POINT ( 'NONE',  ( -38.41701585771487260, 6.978388747684010518, 62.04930799450052348 ) ) ;
#2922 = AXIS2_PLACEMENT_3D ( 'NONE', #22353, #24663, #2180 ) ;
#2923 = ORIENTED_EDGE ( 'NONE', *, *, #25215, .T. ) ;
#2924 = EDGE_CURVE ( 'NONE', #9356, #12175, #6500, .T. ) ;
#2925 = ADVANCED_FACE ( 'NONE', ( #3388 ), #6177, .F. ) ;
#2926 = ADVANCED_FACE ( 'NONE', ( #29150 ), #9614, .T. ) ;
#2927 = CARTESIAN_POINT ( 'NONE',  ( 21.09992658989238734, 38.56284415653841791, 47.04930799450051637 ) ) ;
#2928 = LINE ( 'NONE', #12960, #17990 ) ;
#2929 = EDGE_CURVE ( 'NONE', #21091, #11329, #12266, .T. ) ;
#2930 = CARTESIAN_POINT ( 'NONE',  ( 46.99023568444673060, 26.43791119454915517, 49.12151524109405898 ) ) ;
#2931 = ORIENTED_EDGE ( 'NONE', *, *, #32403, .T. ) ;
#2932 = ORIENTED_EDGE ( 'NONE', *, *, #9760, .T. ) ;
#2933 = DIRECTION ( 'NONE',  ( -1.101824276508909887E-16, 1.000000000000000000, -0.000000000000000000 ) ) ;
#2934 = ORIENTED_EDGE ( 'NONE', *, *, #7599, .T. ) ;
#2935 = CIRCLE ( 'NONE', #15520, 13.00000000000000533 ) ;
#2936 = DIRECTION ( 'NONE',  ( 0.000000000000000000, 0.000000000000000000, -1.000000000000000000 ) ) ;
#2937 = CARTESIAN_POINT ( 'NONE',  ( 54.80744232836631369, -3.171899563477265094, 102.6569140501756152 ) ) ;
#2938 = CARTESIAN_POINT ( 'NONE',  ( 21.09785597605720753, 13.78442380691147839, 47.04930799450052348 ) ) ;
#2939 = CARTESIAN_POINT ( 'NONE',  ( 47.88116631533108603, 22.93807716476589675, 45.54480264941530265 ) ) ;
#2940 = CARTESIAN_POINT ( 'NONE',  ( 21.09785597605720753, 13.80129159329807287, 47.04930799450052348 ) ) ;
#2941 = ITEM_DEFINED_TRANSFORMATION ( 'NONE', 'NONE', #14488,  #8172 ) ;
#2942 = ORIENTED_EDGE ( 'NONE', *, *, #6749, .F. ) ;
#2943 = DIRECTION ( 'NONE',  ( -1.224646799147353207E-16, -1.349345573449484691E-32, 1.000000000000000000 ) ) ;
#2944 = DIRECTION ( 'NONE',  ( 0.1949050434465264547, -0.6797146636928678154, 0.7071067811865470176 ) ) ;
#2945 = CARTESIAN_POINT ( 'NONE',  ( 21.09785597605720397, -15.93545420775219945, 131.5493079945005377 ) ) ;
#2946 = DIRECTION ( 'NONE',  ( 0.000000000000000000, -0.000000000000000000, -1.000000000000000000 ) ) ;
#2947 = EDGE_LOOP ( 'NONE', ( #22043, #26815, #24946, #6905 ) ) ;
#2948 = CARTESIAN_POINT ( 'NONE',  ( -40.20068974435373121, 7.604379238274955100, 53.94930799450051495 ) ) ;
#2949 = DIRECTION ( 'NONE',  ( 1.234978253042719660E-16, -1.000000000000000000, -1.109335647967047851E-31 ) ) ;
#2950 = DIRECTION ( 'NONE',  ( -1.000000000000000000, 0.000000000000000000, 0.000000000000000000 ) ) ;
#2951 = ORIENTED_EDGE ( 'NONE', *, *, #24151, .F. ) ;
#2952 = EDGE_CURVE ( 'NONE', #16490, #29214, #12461, .T. ) ;
#2953 = EDGE_CURVE ( 'NONE', #25453, #12063, #26847, .T. ) ;
#2954 = AXIS2_PLACEMENT_3D ( 'NONE', #24614, #4762, #4587 ) ;
#2955 = ORIENTED_EDGE ( 'NONE', *, *, #21589, .F. ) ;
#2956 = ORIENTED_EDGE ( 'NONE', *, *, #19881, .F. ) ;
#2957 = CARTESIAN_POINT ( 'NONE',  ( -42.38687957179150345, 4.148162238788003719, 57.04930799450051637 ) ) ;
#2958 = DIRECTION ( 'NONE',  ( -1.000000000000000000, 0.000000000000000000, 0.000000000000000000 ) ) ;
#2959 = CARTESIAN_POINT ( 'NONE',  ( 21.09992658989239089, 25.09184655352419213, 47.04930799450051637 ) ) ;
#2960 = ORIENTED_EDGE ( 'NONE', *, *, #12826, .T. ) ;
#2961 = CARTESIAN_POINT ( 'NONE',  ( -29.27613032885505007, 11.92558985988973497, 67.46350265493038023 ) ) ;
#2962 = FACE_OUTER_BOUND ( 'NONE', #5982, .T. ) ;
#2963 = DIRECTION ( 'NONE',  ( -0.9612616959383205595, -0.2756373558169931681, 1.660411357259282445E-16 ) ) ;
#2964 = ADVANCED_FACE ( 'NONE', ( #21908 ), #1734, .F. ) ;
#2965 = VECTOR ( 'NONE', #31329, 1000.000000000000000 ) ;
#2966 = DIRECTION ( 'NONE',  ( -1.000000000000000000, 0.000000000000000000, 0.000000000000000000 ) ) ;
#2967 = CARTESIAN_POINT ( 'NONE',  ( -40.70484894842233103, 8.274204744976163539, 54.44930799450051495 ) ) ;
#2968 = DIRECTION ( 'NONE',  ( 0.000000000000000000, 1.517883041479704827E-15, -1.000000000000000000 ) ) ;
#2969 = CARTESIAN_POINT ( 'NONE',  ( -40.57832943677391313, 7.446916543903029151, 60.23803160207061325 ) ) ;
#2970 = CARTESIAN_POINT ( 'NONE',  ( 8.823575513742490273, 15.24673779880127356, 47.37072134000479906 ) ) ;
#2971 = CARTESIAN_POINT ( 'NONE',  ( -39.59300248568538194, 7.744584186742829779, 32.04930799450052348 ) ) ;
#2972 = CARTESIAN_POINT ( 'NONE',  ( 43.70893385272968601, 11.69718155787697356, 98.26783381802677297 ) ) ;
#2973 = CARTESIAN_POINT ( 'NONE',  ( -42.37913764077812573, 15.23192269303853053, 38.44930799450052206 ) ) ;
#2974 = ORIENTED_EDGE ( 'NONE', *, *, #30326, .F. ) ;
#2975 = ORIENTED_EDGE ( 'NONE', *, *, #14761, .F. ) ;
#2976 = LINE ( 'NONE', #11187, #1899 ) ;
#2977 = CARTESIAN_POINT ( 'NONE',  ( 21.09992658989239089, 26.09164230456639899, 47.04930799450051637 ) ) ;
#2978 = TOROIDAL_SURFACE ( 'NONE', #1412, 12.61792373059897798, 0.1249999999999968636 ) ;
#2979 = DIRECTION ( 'NONE',  ( 0.000000000000000000, 0.000000000000000000, -1.000000000000000000 ) ) ;
#2980 = EDGE_LOOP ( 'NONE', ( #25527, #19797, #14227, #2141 ) ) ;
#2981 = CARTESIAN_POINT ( 'NONE',  ( -41.23380787120766655, 11.23768311167744294, 35.90717268343339441 ) ) ;
#2982 = LINE ( 'NONE', #27947, #3798 ) ;
#2983 = CARTESIAN_POINT ( 'NONE',  ( -40.00476266209339116, 7.314288625133150035, 38.76830122587732319 ) ) ;
#2984 = EDGE_CURVE ( 'NONE', #22139, #31904, #10708, .T. ) ;
#2985 = EDGE_LOOP ( 'NONE', ( #4919, #1388, #31234, #29479 ) ) ;
#2986 = ORIENTED_EDGE ( 'NONE', *, *, #710, .T. ) ;
#2987 = DIRECTION ( 'NONE',  ( -1.101824276508909887E-16, 1.000000000000000000, -0.000000000000000000 ) ) ;
#2988 = CARTESIAN_POINT ( 'NONE',  ( 49.49063479933183629, 26.69951373492759927, 47.17357720316391578 ) ) ;
#2989 = CARTESIAN_POINT ( 'NONE',  ( 48.18662509608405031, 29.29624452788248234, 49.18364984542562013 ) ) ;
#2990 = EDGE_CURVE ( 'NONE', #4508, #8640, #27007, .T. ) ;
#2991 = CARTESIAN_POINT ( 'NONE',  ( -39.48645896158937774, -5.935494601668936276, 77.87709717717420688 ) ) ;
#2992 = ADVANCED_FACE ( 'NONE', ( #6504 ), #2307, .T. ) ;
#2993 = CIRCLE ( 'NONE', #20277, 2.000000000000001776 ) ;
#2994 = EDGE_CURVE ( 'NONE', #10069, #32344, #11592, .T. ) ;
#2995 = EDGE_LOOP ( 'NONE', ( #31600, #19757, #7686, #16895 ) ) ;
#2996 = ADVANCED_FACE ( 'NONE', ( #4522 ), #19055, .T. ) ;
#2997 = DIRECTION ( 'NONE',  ( 0.4544104193609911913, 0.000000000000000000, 0.8907924397839085406 ) ) ;
#2998 = DIRECTION ( 'NONE',  ( 0.000000000000000000, -0.000000000000000000, -1.000000000000000000 ) ) ;
#2999 = ORIENTED_EDGE ( 'NONE', *, *, #19749, .F. ) ;
#3000 = CARTESIAN_POINT ( 'NONE',  ( 47.63716429968716426, 26.91960992152948151, 49.58068632438585865 ) ) ;
#3001 = CARTESIAN_POINT ( 'NONE',  ( 21.09992658989239089, 25.09164230456639899, 47.04930799450051637 ) ) ;
#3002 = ADVANCED_FACE ( 'NONE', ( #32105 ), #6663, .T. ) ;
#3003 = VERTEX_POINT ( 'NONE', #14222 ) ;
#3004 = DIRECTION ( 'NONE',  ( -0.8746197071393926326, 0.4848096202463430537, 8.676864087101709653E-18 ) ) ;
#3005 = DIRECTION ( 'NONE',  ( -1.000000000000000000, 0.000000000000000000, 0.000000000000000000 ) ) ;
#3006 = DIRECTION ( 'NONE',  ( -1.000000000000000000, 0.000000000000000000, 0.000000000000000000 ) ) ;
#3007 = DIRECTION ( 'NONE',  ( -0.000000000000000000, -1.000000000000000000, 0.000000000000000000 ) ) ;
#3008 = DIRECTION ( 'NONE',  ( 0.000000000000000000, 1.000000000000000000, -0.000000000000000000 ) ) ;
#3009 = ORIENTED_EDGE ( 'NONE', *, *, #27393, .F. ) ;
#3010 = CARTESIAN_POINT ( 'NONE',  ( 76.42527971025482714, -3.977894809549873401, 80.53958960090274388 ) ) ;
#3012 = DIRECTION ( 'NONE',  ( 0.000000000000000000, -0.000000000000000000, -1.000000000000000000 ) ) ;
#3011 = TOROIDAL_SURFACE ( 'NONE', #26582, 12.61792373059891226, 0.1250000000000024980 ) ;
#3013 = CIRCLE ( 'NONE', #23981, 22.00000000000000000 ) ;
#3014 = CARTESIAN_POINT ( 'NONE',  ( 33.72499318558949710, 28.09184655352419213, 47.04930799450051637 ) ) ;
#3015 = DIRECTION ( 'NONE',  ( -1.000000000000000000, -1.101824276508909887E-16, 0.000000000000000000 ) ) ;
#3016 = CARTESIAN_POINT ( 'NONE',  ( 76.50383461303660226, -2.878806504921911813, 80.77738562869335226 ) ) ;
#3017 = ORIENTED_EDGE ( 'NONE', *, *, #1837, .F. ) ;
#3018 = CARTESIAN_POINT ( 'NONE',  ( 49.73084373776887901, 24.88948912900243116, 46.55219242998139606 ) ) ;
#3019 = CARTESIAN_POINT ( 'NONE',  ( 21.09992658989239089, 25.84164230456639899, 47.04930799450051637 ) ) ;
#3020 = CIRCLE ( 'NONE', #27138, 12.36707279061065101 ) ;
#3021 = EDGE_CURVE ( 'NONE', #15217, #27344, #29039, .T. ) ;
#3022 = EDGE_LOOP ( 'NONE', ( #4299, #29590, #26515, #5708 ) ) ;
#3023 = CARTESIAN_POINT ( 'NONE',  ( 21.09785597605719687, 40.56454579224780588, 17.04930799450051637 ) ) ;
#3024 = DIRECTION ( 'NONE',  ( -1.101824276508909887E-16, 1.000000000000000000, -0.000000000000000000 ) ) ;
#3025 = CARTESIAN_POINT ( 'NONE',  ( 51.92400919103565116, -5.935454207752198563, -37.95069200549950494 ) ) ;
#3026 = ADVANCED_FACE ( 'NONE', ( #17143 ), #18019, .F. ) ;
#3027 = CARTESIAN_POINT ( 'NONE',  ( 53.25347890682692054, -5.581242224118425632, -11.00365297242568374 ) ) ;
#3028 = ORIENTED_EDGE ( 'NONE', *, *, #4339, .F. ) ;
#3029 = CARTESIAN_POINT ( 'NONE',  ( 21.09785597605719687, -13.30631372918550959, -8.763520691563154941 ) ) ;
#3030 = ORIENTED_EDGE ( 'NONE', *, *, #14643, .T. ) ;
#3031 = EDGE_CURVE ( 'NONE', #16525, #8364, #3873, .T. ) ;
#3032 = ORIENTED_EDGE ( 'NONE', *, *, #1070, .F. ) ;
#3033 = EDGE_CURVE ( 'NONE', #23532, #9452, #20647, .T. ) ;
#3034 = VECTOR ( 'NONE', #6705, 1000.000000000000114 ) ;
#3035 = AXIS2_PLACEMENT_3D ( 'NONE', #2073, #9793, #12757 ) ;
#3036 = CIRCLE ( 'NONE', #25588, 0.1250000000000001110 ) ;
#3037 = TOROIDAL_SURFACE ( 'NONE', #20331, 12.61792373059890693, 0.1250000000000019429 ) ;
#3038 = CARTESIAN_POINT ( 'NONE',  ( 49.98072202819531640, 27.64488759933318818, 47.19902993264913960 ) ) ;
#3039 = DIRECTION ( 'NONE',  ( 0.4848096202463430537, 0.8746197071393926326, 9.920727850371700117E-18 ) ) ;
#3040 = CARTESIAN_POINT ( 'NONE',  ( 48.23388202445966755, 15.77906836436399374, 49.27628909396055690 ) ) ;
#3041 = EDGE_LOOP ( 'NONE', ( #31383, #31666, #14852, #21465 ) ) ;
#3042 = AXIS2_PLACEMENT_3D ( 'NONE', #2653, #7742, #10050 ) ;
#3043 = ORIENTED_EDGE ( 'NONE', *, *, #3175, .F. ) ;
#3044 = DIRECTION ( 'NONE',  ( -0.8907924160295463967, -1.100109261771873301E-16, 0.4544104659272754088 ) ) ;
#3045 = CARTESIAN_POINT ( 'NONE',  ( 21.09785597605720753, 13.95840365082257151, 47.04930799450052348 ) ) ;
#3046 = CARTESIAN_POINT ( 'NONE',  ( 33.46699938050303302, 38.56284415653841791, 47.04930799450051637 ) ) ;
#3047 = CARTESIAN_POINT ( 'NONE',  ( 21.09785597605719332, 42.30003263981368633, 47.04930799450051637 ) ) ;
#3048 = ORIENTED_EDGE ( 'NONE', *, *, #2780, .F. ) ;
#3049 = CARTESIAN_POINT ( 'NONE',  ( 21.09992658989239089, 26.84184655352419568, 47.04930799450051637 ) ) ;
#3050 = VERTEX_POINT ( 'NONE', #8962 ) ;
#3051 = FACE_OUTER_BOUND ( 'NONE', #24335, .T. ) ;
#3052 = DIRECTION ( 'NONE',  ( -1.000000000000000000, 0.000000000000000000, 0.000000000000000000 ) ) ;
#3053 = ORIENTED_EDGE ( 'NONE', *, *, #5071, .T. ) ;
#3054 = CARTESIAN_POINT ( 'NONE',  ( -40.18454328187963398, 7.548069831825862330, 53.64930799450051779 ) ) ;
#3055 = DIRECTION ( 'NONE',  ( -1.101824276508909887E-16, 1.000000000000000000, -0.000000000000000000 ) ) ;
#3056 = CARTESIAN_POINT ( 'NONE',  ( -44.16550389150962985, 1.558238629217584492, 34.54930799450052348 ) ) ;
#3057 = DIRECTION ( 'NONE',  ( 0.000000000000000000, 0.000000000000000000, -1.000000000000000000 ) ) ;
#3058 = LINE ( 'NONE', #23093, #26228 ) ;
#3059 = DIRECTION ( 'NONE',  ( -1.000000000000000000, 0.000000000000000000, 0.000000000000000000 ) ) ;
#3060 = DIRECTION ( 'NONE',  ( -1.000000000000000000, 0.000000000000000000, 0.000000000000000000 ) ) ;
#3061 = ORIENTED_EDGE ( 'NONE', *, *, #10945, .T. ) ;
#3062 = CARTESIAN_POINT ( 'NONE',  ( -40.90015969217747482, 8.955334253785164123, 57.04930799450051637 ) ) ;
#3063 = AXIS2_PLACEMENT_3D ( 'NONE', #26093, #16082, #6241 ) ;
#3064 = CARTESIAN_POINT ( 'NONE',  ( 45.96182992765472619, 28.00087065737811898, 44.82232689504102296 ) ) ;
#3065 = CIRCLE ( 'NONE', #25607, 78.39999999999999147 ) ;
#3066 = VERTEX_POINT ( 'NONE', #18955 ) ;
#3067 = CIRCLE ( 'NONE', #10926, 19.25826962553310295 ) ;
#3068 = ORIENTED_EDGE ( 'NONE', *, *, #25059, .F. ) ;
#3069 = DIRECTION ( 'NONE',  ( -1.000000000000000000, -1.101824276508910010E-16, 0.000000000000000000 ) ) ;
#3070 = EDGE_CURVE ( 'NONE', #9009, #25296, #26523, .T. ) ;
#3071 = CIRCLE ( 'NONE', #6753, 1.300000000000002487 ) ;
#3072 = ORIENTED_EDGE ( 'NONE', *, *, #16965, .F. ) ;
#3073 = EDGE_CURVE ( 'NONE', #9700, #17034, #4934, .T. ) ;
#3074 = ORIENTED_EDGE ( 'NONE', *, *, #2484, .T. ) ;
#3075 = DIRECTION ( 'NONE',  ( 0.000000000000000000, 1.000000000000000000, -0.000000000000000000 ) ) ;
#3076 = CIRCLE ( 'NONE', #462, 2.500000000000003553 ) ;
#3077 = AXIS2_PLACEMENT_3D ( 'NONE', #1533, #1059, #1374 ) ;
#3078 = VERTEX_POINT ( 'NONE', #10430 ) ;
#3079 = AXIS2_PLACEMENT_3D ( 'NONE', #16869, #3916, #19495 ) ;
#3080 = CARTESIAN_POINT ( 'NONE',  ( -14.40214402394279780, 14.86454579224779948, 47.04930799450052348 ) ) ;
#3081 = CYLINDRICAL_SURFACE ( 'NONE', #23837, 1.500000000000001332 ) ;
#3082 = FACE_OUTER_BOUND ( 'NONE', #52, .T. ) ;
#3083 = PRODUCT_RELATED_PRODUCT_CATEGORY ( 'part', '', ( #14546 ) ) ;
#3084 = CARTESIAN_POINT ( 'NONE',  ( 48.80717017713595141, 28.67622849631042570, 48.15820438821415195 ) ) ;
#3085 = ORIENTED_EDGE ( 'NONE', *, *, #30114, .T. ) ;
#3086 = ORIENTED_EDGE ( 'NONE', *, *, #29203, .F. ) ;
#3087 = LINE ( 'NONE', #13127, #6941 ) ;
#3088 = ORIENTED_EDGE ( 'NONE', *, *, #28269, .T. ) ;
#3089 = DIRECTION ( 'NONE',  ( -1.000000000000000000, 0.000000000000000000, 0.000000000000000000 ) ) ;
#3090 = CARTESIAN_POINT ( 'NONE',  ( 21.09992658989238734, 32.34184655352418503, 47.04930799450051637 ) ) ;
#3091 = CARTESIAN_POINT ( 'NONE',  ( 21.09992658989239089, 28.59164230456639544, 47.04930799450051637 ) ) ;
#3092 = CIRCLE ( 'NONE', #25726, 66.44011198581388555 ) ;
#3093 = DIRECTION ( 'NONE',  ( 0.2756373558170013283, -0.9612616959383183390, 0.000000000000000000 ) ) ;
#3094 = CYLINDRICAL_SURFACE ( 'NONE', #25774, 12.36707279061065101 ) ;
#3095 = ORIENTED_EDGE ( 'NONE', *, *, #26603, .T. ) ;
#3096 = DIRECTION ( 'NONE',  ( -1.101824276508909887E-16, 1.000000000000000000, -0.000000000000000000 ) ) ;
#3097 = DIRECTION ( 'NONE',  ( -1.101824276508909887E-16, 1.000000000000000000, -0.000000000000000000 ) ) ;
#3098 = CARTESIAN_POINT ( 'NONE',  ( -37.42114908093812176, 11.86897798031838391, 60.54930799450051637 ) ) ;
#3099 = CARTESIAN_POINT ( 'NONE',  ( 45.79384627280941800, 25.76618040159426926, 49.05938063676250493 ) ) ;
#3100 = ORIENTED_EDGE ( 'NONE', *, *, #20202, .T. ) ;
#3101 = DIRECTION ( 'NONE',  ( 0.4544104193609903586, 0.000000000000000000, 0.8907924397839087627 ) ) ;
#3102 = CYLINDRICAL_SURFACE ( 'NONE', #22976, 12.62506659569710266 ) ;
#3104 = EDGE_CURVE ( 'NONE', #7358, #18405, #20104, .T. ) ;
#3103 = AXIS2_PLACEMENT_3D ( 'NONE', #14838, #26969, #4490 ) ;
#3105 = DIRECTION ( 'NONE',  ( -0.000000000000000000, -1.000000000000000000, 0.000000000000000000 ) ) ;
#3106 = VERTEX_POINT ( 'NONE', #5347 ) ;
#3107 = EDGE_CURVE ( 'NONE', #3673, #2441, #17504, .T. ) ;
#3108 = EDGE_CURVE ( 'NONE', #17233, #18486, #24710, .T. ) ;
#3109 = EDGE_CURVE ( 'NONE', #529, #11769, #28510, .T. ) ;
#3110 = EDGE_CURVE ( 'NONE', #13235, #26545, #31136, .T. ) ;
#3111 = TOROIDAL_SURFACE ( 'NONE', #15197, 12.40141737965285706, 0.1250000000000007494 ) ;
#3112 = CIRCLE ( 'NONE', #23030, 2.950930354263400890 ) ;
#3113 = VERTEX_POINT ( 'NONE', #19939 ) ;
#3114 = EDGE_LOOP ( 'NONE', ( #20878, #24219, #4831, #4347 ) ) ;
#3115 = CARTESIAN_POINT ( 'NONE',  ( 48.55603101936429056, 22.91413368675619111, 45.98877541807350156 ) ) ;
#3116 = VECTOR ( 'NONE', #20424, 1000.000000000000114 ) ;
#3117 = DIRECTION ( 'NONE',  ( -1.101824276508909887E-16, 1.000000000000000000, -0.000000000000000000 ) ) ;
#3118 = CARTESIAN_POINT ( 'NONE',  ( 21.09785597605720042, -13.59284023713420630, 47.04930799450051637 ) ) ;
#3119 = VERTEX_POINT ( 'NONE', #12410 ) ;
#3120 = CARTESIAN_POINT ( 'NONE',  ( -29.27613032885505007, 2.267353962593735339, 79.30155859000750240 ) ) ;
#3121 = CARTESIAN_POINT ( 'NONE',  ( -40.73091736380679606, 9.483895492497158131, 39.44930799450052206 ) ) ;
#3122 = DIRECTION ( 'NONE',  ( -1.101824276508909887E-16, 1.000000000000000000, -0.000000000000000000 ) ) ;
#3123 = DIRECTION ( 'NONE',  ( -1.101824276508909887E-16, 1.000000000000000000, -0.000000000000000000 ) ) ;
#3124 = CIRCLE ( 'NONE', #28819, 4.000000000000000000 ) ;
#3125 = AXIS2_PLACEMENT_3D ( 'NONE', #29089, #6607, #16286 ) ;
#3126 = DIRECTION ( 'NONE',  ( -0.000000000000000000, 1.000000000000000000, -0.000000000000000000 ) ) ;
#3127 = DIRECTION ( 'NONE',  ( 1.431146867680865853E-17, 2.558717127065790464E-17, 1.000000000000000000 ) ) ;
#3128 = CARTESIAN_POINT ( 'NONE',  ( 21.09992658989239089, 28.34164230456639544, 47.04930799450051637 ) ) ;
#3129 = DIRECTION ( 'NONE',  ( 0.4544104193609900810, 0.000000000000000000, 0.8907924397839089847 ) ) ;
#3130 = PLANE ( 'NONE',  #9431 ) ;
#3131 = CARTESIAN_POINT ( 'NONE',  ( 48.46535932150934656, 28.28954579807170688, 49.73005965046827015 ) ) ;
#3132 = ORIENTED_EDGE ( 'NONE', *, *, #13461, .T. ) ;
#3133 = EDGE_LOOP ( 'NONE', ( #16009, #187, #22875, #25955 ) ) ;
#3134 = EDGE_CURVE ( 'NONE', #27738, #29931, #10692, .T. ) ;
#3135 = DIRECTION ( 'NONE',  ( 1.000000000000000000, 0.000000000000000000, 0.000000000000000000 ) ) ;
#3136 = CARTESIAN_POINT ( 'NONE',  ( 47.35966831703180446, 25.13711290387551855, 44.54181020796264079 ) ) ;
#3137 = CARTESIAN_POINT ( 'NONE',  ( 21.09785597605719332, -16.63545420775219696, 123.7593585008393831 ) ) ;
#3138 = VERTEX_POINT ( 'NONE', #12570 ) ;
#3139 = DIRECTION ( 'NONE',  ( -1.000000000000000000, 0.000000000000000000, 0.000000000000000000 ) ) ;
#3140 = AXIS2_PLACEMENT_3D ( 'NONE', #11063, #16290, #28937 ) ;
#3141 = CARTESIAN_POINT ( 'NONE',  ( -40.02667234278160890, 7.000595883235202876, 39.42620813939996793 ) ) ;
#3142 = ORIENTED_EDGE ( 'NONE', *, *, #26856, .T. ) ;
#3143 = EDGE_LOOP ( 'NONE', ( #3357, #5469, #5179, #30796 ) ) ;
#3144 = DIRECTION ( 'NONE',  ( -1.000000000000000000, 0.000000000000000000, 0.000000000000000000 ) ) ;
#3145 = CONICAL_SURFACE ( 'NONE', #21477, 67.36417311134205477, 1.291543646476234874 ) ;
#3146 = CARTESIAN_POINT ( 'NONE',  ( 47.20547626766766314, 28.27451373492759501, 44.97710074790751378 ) ) ;
#3147 = TOROIDAL_SURFACE ( 'NONE', #7361, 19.31976987914897848, 0.2000000000000029809 ) ;
#3148 = CARTESIAN_POINT ( 'NONE',  ( 44.70507715278255745, 29.76291119454914380, 46.92503878583764987 ) ) ;
#3149 = CARTESIAN_POINT ( 'NONE',  ( -34.55638539710868429, 11.69883593934741128, 53.11441734066968934 ) ) ;
#3150 = ADVANCED_FACE ( 'NONE', ( #17312 ), #16955, .T. ) ;
#3151 = ADVANCED_FACE ( 'NONE', ( #27335 ), #21146, .T. ) ;
#3152 = AXIS2_PLACEMENT_3D ( 'NONE', #1511, #6768, #28768 ) ;
#3153 = ORIENTED_EDGE ( 'NONE', *, *, #29232, .T. ) ;
#3154 = CARTESIAN_POINT ( 'NONE',  ( 51.92400919103563695, -5.935454207752202116, -13.56214536183033381 ) ) ;
#3155 = DIRECTION ( 'NONE',  ( -1.000000000000000000, 0.000000000000000000, 0.000000000000000000 ) ) ;
#3156 = AXIS2_PLACEMENT_3D ( 'NONE', #31133, #8483, #18478 ) ;
#3157 = AXIS2_PLACEMENT_3D ( 'NONE', #31995, #2729, #25374 ) ;
#3158 = ORIENTED_EDGE ( 'NONE', *, *, #6146, .T. ) ;
#3159 = AXIS2_PLACEMENT_3D ( 'NONE', #32179, #14457, #32009 ) ;
#3160 = CYLINDRICAL_SURFACE ( 'NONE', #25404, 12.62506659569710266 ) ;
#3161 = CARTESIAN_POINT ( 'NONE',  ( 46.48525799733394592, 23.04411619146717882, 47.99360027521537830 ) ) ;
#3162 = CIRCLE ( 'NONE', #17846, 55.87116166729571631 ) ;
#3163 = DIRECTION ( 'NONE',  ( -0.7141240004913222972, 0.3958453973320028019, 0.5773502691896303940 ) ) ;
#3164 = PRESENTATION_LAYER_ASSIGNMENT (  '', '', ( #13150 ) ) ;
#3165 = ADVANCED_FACE ( 'NONE', ( #2869 ), #29802, .F. ) ;
#3166 = EDGE_LOOP ( 'NONE', ( #30523, #4042, #31346, #7444 ) ) ;
#3167 = CARTESIAN_POINT ( 'NONE',  ( 33.72499318558949710, 28.34143805560861296, 47.04930799450051637 ) ) ;
#3168 = CARTESIAN_POINT ( 'NONE',  ( 21.09785597605719332, 25.56454579224779877, 47.04930799450051637 ) ) ;
#3169 = CARTESIAN_POINT ( 'NONE',  ( 33.72499318558949000, 38.56284415653841791, 47.04930799450051637 ) ) ;
#3170 = LINE ( 'NONE', #17472, #23870 ) ;
#3171 = ORIENTED_EDGE ( 'NONE', *, *, #28400, .T. ) ;
#3172 = EDGE_CURVE ( 'NONE', #25895, #7948, #8581, .T. ) ;
#3173 = CARTESIAN_POINT ( 'NONE',  ( -37.58300281841709989, 16.01180101885526597, 38.09144330556765112 ) ) ;
#3174 = CARTESIAN_POINT ( 'NONE',  ( 21.09785597605719332, -9.935454207752199451, 47.04930799450051637 ) ) ;
#3175 = EDGE_CURVE ( 'NONE', #2467, #21280, #30595, .T. ) ;
#3176 = DIRECTION ( 'NONE',  ( -1.101824276508909887E-16, 1.000000000000000000, -0.000000000000000000 ) ) ;
#3177 = CARTESIAN_POINT ( 'NONE',  ( 21.09785597605719332, 24.56454579224780232, 47.04930799450051637 ) ) ;
#3178 = CYLINDRICAL_SURFACE ( 'NONE', #10556, 2.500000000000002220 ) ;
#3179 = ORIENTED_EDGE ( 'NONE', *, *, #18966, .T. ) ;
#3180 = DIRECTION ( 'NONE',  ( -0.9612616959383205595, -0.2756373558169932236, 1.660411357259282445E-16 ) ) ;
#3181 = CARTESIAN_POINT ( 'NONE',  ( 49.72060376828096651, 24.89739800709606499, 46.58538876707991960 ) ) ;
#3182 = FACE_OUTER_BOUND ( 'NONE', #27297, .T. ) ;
#3183 = EDGE_LOOP ( 'NONE', ( #25096, #32071, #16042, #7853 ) ) ;
#3184 = DIRECTION ( 'NONE',  ( 0.000000000000000000, -0.000000000000000000, -1.000000000000000000 ) ) ;
#3185 = CARTESIAN_POINT ( 'NONE',  ( -63.90214402394282445, -5.935454207752202116, 16.07118271501078510 ) ) ;
#3186 = DIRECTION ( 'NONE',  ( -1.000000000000000000, 0.000000000000000000, 0.000000000000000000 ) ) ;
#3187 = AXIS2_PLACEMENT_3D ( 'NONE', #7480, #27159, #27498 ) ;
#3188 = CARTESIAN_POINT ( 'NONE',  ( 51.52198844449087289, 5.308358430270121886, -5.044066518274861188 ) ) ;
#3189 = ORIENTED_EDGE ( 'NONE', *, *, #6713, .T. ) ;
#3190 = CARTESIAN_POINT ( 'NONE',  ( 48.77568013947721681, 22.93807716476589675, 47.29834112010470903 ) ) ;
#3191 = AXIS2_PLACEMENT_3D ( 'NONE', #30328, #27374, #7354 ) ;
#3192 = CIRCLE ( 'NONE', #7919, 19.00000000000000000 ) ;
#3193 = ORIENTED_EDGE ( 'NONE', *, *, #14864, .T. ) ;
#3194 = AXIS2_PLACEMENT_3D ( 'NONE', #430, #10455, #23246 ) ;
#3195 = EDGE_CURVE ( 'NONE', #7566, #32110, #18003, .T. ) ;
#3196 = CIRCLE ( 'NONE', #18902, 20.38082872909741994 ) ;
#3197 = EDGE_LOOP ( 'NONE', ( #1318, #3565, #29612, #29507 ) ) ;
#3198 = B_SPLINE_CURVE_WITH_KNOTS ( 'NONE', 3,
 ( #28375, #13595, #25577, #13444, #468, #28048, #3568, #26053, #28208, #794 ),
 .UNSPECIFIED., .F., .F.,
 ( 4, 2, 2, 2, 4 ),
 ( 0.000000000000000000, 0.0008384749106984661516, 0.001257712366047681338, 0.001467331093722273319, 0.001676949821396865299 ),
 .UNSPECIFIED. ) ;
#3199 = AXIS2_PLACEMENT_3D ( 'NONE', #4469, #4630, #11701 ) ;
#3200 = ADVANCED_FACE ( 'NONE', ( #4853 ), #25367, .F. ) ;
#3201 = CARTESIAN_POINT ( 'NONE',  ( 21.09992658989238734, 30.97145308207317171, 47.04930799450051637 ) ) ;
#3202 = DIRECTION ( 'NONE',  ( -1.101824276508909887E-16, 1.000000000000000000, -0.000000000000000000 ) ) ;
#3203 = CARTESIAN_POINT ( 'NONE',  ( 33.72499318558949000, 38.56284415653841791, 47.04930799450051637 ) ) ;
#3204 = EDGE_CURVE ( 'NONE', #14460, #10889, #6476, .T. ) ;
#3205 = ORIENTED_EDGE ( 'NONE', *, *, #15041, .F. ) ;
#3206 = CARTESIAN_POINT ( 'NONE',  ( 45.44030796846719511, 22.86454579224779948, 45.92951929762858043 ) ) ;
#3207 = ORIENTED_EDGE ( 'NONE', *, *, #14170, .F. ) ;
#3208 = AXIS2_PLACEMENT_3D ( 'NONE', #29141, #31767, #3868 ) ;
#3209 = CARTESIAN_POINT ( 'NONE',  ( -9.728297238921257417, -5.935454207752202116, 106.8025418868326284 ) ) ;
#3210 = AXIS2_PLACEMENT_3D ( 'NONE', #25361, #32104, #7646 ) ;
#3211 = FACE_OUTER_BOUND ( 'NONE', #19132, .T. ) ;
#3212 = CARTESIAN_POINT ( 'NONE',  ( -35.20928760015869585, -4.023206877552709670, 80.51010491862120944 ) ) ;
#3213 = DIRECTION ( 'NONE',  ( -1.000000000000000000, 0.000000000000000000, 0.000000000000000000 ) ) ;
#3214 = CIRCLE ( 'NONE', #21551, 12.36707279061065279 ) ;
#3215 = ORIENTED_EDGE ( 'NONE', *, *, #6112, .T. ) ;
#3216 = CLOSED_SHELL ( 'NONE', ( #5387, #22410, #23745, #26164, #7189, #23787, #4533, #20018, #1337, #8499, #20156, #26105, #21236, #5713, #23815, #26573, #30862, #630, #28094, #5545, #1438, #16925, #570, #12981, #24711, #23934, #7824, #30266, #7954, #10399, #9761, #28096, #17342, #31268, #16050, #29813, #3516, #18163, #31132, #22673, #7229, #14594, #29121, #11054, #19746, #20644, #3561, #24605, #3770, #13586, #6080, #6, #23904, #26608, #24436, #22049, #30282, #25126, #27081, #717, #20797, #16148, #6605, #11346, #3717, #10379, #11848, #9338, #13427, #7862, #27433, #3650, #21326, #9363, #26160, #672, #8933, #29983, #4866, #3479, #13432, #8625, #15674, #2925, #13083, #4943, #29953, #10649, #183, #29894, #14873, #28056, #28251, #32214, #26121, #10592, #28452, #28755, #26790, #26753, #6345, #3405, #21279, #31030, #28872, #299, #406, #25268, #21657, #14677, #9296, #14356, #6073, #9265, #17484, #20882, #12422, #4450, #25708, #28324, #995, #449, #28278, #28274, #16479, #13022, #27532, #26489, #22178, #11923, #28706, #2377, #5715, #12464, #27221, #12173, #1627, #19017, #26605, #23653, #23163, #11520, #24385, #10210, #334, #28485, #19245, #24194, #17333, #2964, #31749, #2308, #4863, #31388, #21272, #12659, #28203, #16586, #12956, #1107, #27713, #9857, #10092, #19614, #28796, #30660, #51, #12353, #3416, #6714, #6841, #19131, #17940, #28612, #13358, #14656, #8634, #31671, #18658, #29496, #9382, #15491, #14091, #6348, #2888, #27204, #24945, #1948, #25838, #129, #6673, #28236, #10084, #9123, #5636, #15705, #7642, #16781, #9016, #22292, #23445, #32401, #8181, #19254, #30307, #5718, #1381, #11349, #7543, #1996, #5276, #26304, #25971, #25500, #27879, #31586, #10004, #28396, #9788, #23678, #26571, #25970, #13138, #1253, #15395, #4825, #23992, #84, #23484, #13063, #14310, #22707, #8089, #7418, #19185, #8052, #6429, #28898, #14760, #17168, #27625, #25608, #8340, #6041, #23390, #14209, #13456, #23708, #23275, #15786, #5012, #14304, #25043, #16741, #9499, #16452, #6395, #28948, #27804, #12986, #29990, #10874, #14573, #19856, #13467, #18164, #24982, #7498, #5627, #10770, #18252, #5191, #8266, #5996, #9911, #9946, #20763, #4370, #12702, #30445, #21288, #6117, #21240, #18922, #21068, #26043, #28481, #1539, #23568, #20707, #4658, #24870, #14990, #5082, #24387, #13356, #1738, #10949, #950, #2996, #19420, #11843, #625, #9598, #28128, #12049, #31437, #25923, #130, #2070, #23002, #20758, #4215, #30670, #3591, #10353, #6572, #15125, #26496, #11974, #2760, #4414, #26080, #18010, #26269, #21386, #31548, #32215, #1171, #31309, #20057, #23058, #15013, #8010, #21430, #14083, #11818, #17449, #12871, #24401, #377, #16836, #13681, #24848, #220, #3150, #24380, #5319, #23571, #3300, #30399, #30831, #5758, #31214, #2258, #12949, #13186, #22562, #26604, #5794, #10352, #26201, #20928, #29721, #8656, #11087, #18025, #24717 ) ) ;
#3217 = DIRECTION ( 'NONE',  ( -1.000000000000000000, 0.000000000000000000, 0.000000000000000000 ) ) ;
#3218 = VERTEX_POINT ( 'NONE', #12743 ) ;
#3219 = CARTESIAN_POINT ( 'NONE',  ( 46.20008674485251987, 20.53597436367637030, 48.43317895773266457 ) ) ;
#3220 = CARTESIAN_POINT ( 'NONE',  ( 21.09785597605719332, 30.56454579224779522, 73.04930799450052348 ) ) ;
#3221 = EDGE_CURVE ( 'NONE', #15469, #15557, #29007, .T. ) ;
#3222 = ORIENTED_EDGE ( 'NONE', *, *, #24187, .F. ) ;
#3223 = FACE_OUTER_BOUND ( 'NONE', #6473, .T. ) ;
#3224 = CARTESIAN_POINT ( 'NONE',  ( -36.31236502847541914, 10.17695955431967114, 52.04930799450051637 ) ) ;
#3225 = CARTESIAN_POINT ( 'NONE',  ( 45.37383841111020644, 22.88065857334295217, 47.92876263475718446 ) ) ;
#3226 = CARTESIAN_POINT ( 'NONE',  ( 8.732853799281732776, 38.56284415653841791, 47.04930799450051637 ) ) ;
#3227 = EDGE_CURVE ( 'NONE', #19822, #2124, #29561, .T. ) ;
#3228 = FACE_OUTER_BOUND ( 'NONE', #21323, .T. ) ;
#3229 = AXIS2_PLACEMENT_3D ( 'NONE', #23885, #4022, #11742 ) ;
#3230 = CARTESIAN_POINT ( 'NONE',  ( 47.09785597605719687, 23.12036939723557083, 47.04930799450080059 ) ) ;
#3231 = CARTESIAN_POINT ( 'NONE',  ( 21.09992658989239089, 28.46664230456639899, 47.04930799450051637 ) ) ;
#3232 = ORIENTED_EDGE ( 'NONE', *, *, #2113, .F. ) ;
#3233 = DIRECTION ( 'NONE',  ( 0.000000000000000000, 0.000000000000000000, -1.000000000000000000 ) ) ;
#3234 = VERTEX_POINT ( 'NONE', #20907 ) ;
#3235 = AXIS2_PLACEMENT_3D ( 'NONE', #20134, #5051, #21935 ) ;
#3236 = CARTESIAN_POINT ( 'NONE',  ( -40.20380355051744914, 8.008426694338135476, 40.07149053519532345 ) ) ;
#3237 = ORIENTED_EDGE ( 'NONE', *, *, #20116, .T. ) ;
#3238 = ORIENTED_EDGE ( 'NONE', *, *, #31675, .F. ) ;
#3239 = CARTESIAN_POINT ( 'NONE',  ( -7.669325564611453316, 7.651854857429011503, 98.59257673948808076 ) ) ;
#3240 = UNCERTAINTY_MEASURE_WITH_UNIT (LENGTH_MEASURE( 1.000000000000000082E-05 ), #27118, 'distance_accuracy_value', 'NONE');
#3241 = CIRCLE ( 'NONE', #15827, 2.000000000000001776 ) ;
#3242 = ORIENTED_EDGE ( 'NONE', *, *, #29491, .F. ) ;
#3243 = AXIS2_PLACEMENT_3D ( 'NONE', #9141, #21766, #26376 ) ;
#3244 = AXIS2_PLACEMENT_3D ( 'NONE', #7279, #17273, #2507 ) ;
#3245 = ORIENTED_EDGE ( 'NONE', *, *, #3999, .T. ) ;
#3246 = ADVANCED_FACE ( 'NONE', ( #3182 ), #13226, .F. ) ;
#3247 = CARTESIAN_POINT ( 'NONE',  ( -40.59758774925371938, 7.567737757495683226, 39.54930799450052348 ) ) ;
#3248 = AXIS2_PLACEMENT_3D ( 'NONE', #29635, #4356, #22230 ) ;
#3249 = EDGE_CURVE ( 'NONE', #3066, #22635, #12794, .T. ) ;
#3250 = VERTEX_POINT ( 'NONE', #1201 ) ;
#3251 = AXIS2_PLACEMENT_3D ( 'NONE', #32371, #36, #14975 ) ;
#3252 = CARTESIAN_POINT ( 'NONE',  ( 48.56989418307995976, 22.92747281079970634, 48.00427463845466036 ) ) ;
#3253 = DIRECTION ( 'NONE',  ( -1.234978253042719660E-16, 1.000000000000000000, 1.109335647967047851E-31 ) ) ;
#3254 = CARTESIAN_POINT ( 'NONE',  ( 21.09992658989239089, 29.84184655352422411, 47.04930799450051637 ) ) ;
#3255 = CARTESIAN_POINT ( 'NONE',  ( 49.44739180854976013, 25.23456182964376993, 47.17133137409169308 ) ) ;
#3256 = EDGE_LOOP ( 'NONE', ( #10233, #3596, #9853, #1908 ) ) ;
#3257 = ORIENTED_EDGE ( 'NONE', *, *, #933, .F. ) ;
#3258 =( LENGTH_UNIT ( ) NAMED_UNIT ( * ) SI_UNIT ( .MILLI., .METRE. ) );
#3259 = EDGE_CURVE ( 'NONE', #17919, #18936, #20629, .T. ) ;
#3260 = ORIENTED_EDGE ( 'NONE', *, *, #14759, .T. ) ;
#3261 = CIRCLE ( 'NONE', #21596, 12.36707279061065279 ) ;
#3262 = CARTESIAN_POINT ( 'NONE',  ( 49.76180767062073329, 24.76486642951281780, 48.77751362531136436 ) ) ;
#3263 = DIRECTION ( 'NONE',  ( -1.000000000000000000, 0.000000000000000000, 0.000000000000000000 ) ) ;
#3264 = CARTESIAN_POINT ( 'NONE',  ( -40.15599670534037102, 7.478908884098773413, 38.70582007960419446 ) ) ;
#3265 = TOROIDAL_SURFACE ( 'NONE', #8018, 39.69941114636694834, 1.000000000000000000 ) ;
#3266 = DIRECTION ( 'NONE',  ( -1.101824276508909887E-16, 1.000000000000000000, -0.000000000000000000 ) ) ;
#3267 = CARTESIAN_POINT ( 'NONE',  ( 21.09785597605720753, 14.16454579224779842, 47.04930799450052348 ) ) ;
#3268 = ITEM_DEFINED_TRANSFORMATION ( 'NONE', 'NONE', #7129,  #8172 ) ;
#3269 = ORIENTED_EDGE ( 'NONE', *, *, #2230, .T. ) ;
#3270 = DIRECTION ( 'NONE',  ( -1.101824276508909887E-16, 1.000000000000000000, -0.000000000000000000 ) ) ;
#3271 = DIRECTION ( 'NONE',  ( -1.101824276508909887E-16, 1.000000000000000000, -0.000000000000000000 ) ) ;
#3272 = CARTESIAN_POINT ( 'NONE',  ( 48.01680169312755453, 22.93807716476589675, 45.63279442905645311 ) ) ;
#3273 = CARTESIAN_POINT ( 'NONE',  ( 45.79384627280941800, 26.46618040159426499, 49.05938063676250493 ) ) ;
#3274 = ORIENTED_EDGE ( 'NONE', *, *, #26901, .T. ) ;
#3275 = CARTESIAN_POINT ( 'NONE',  ( 21.09785597605719687, 25.56454579224779877, 87.23645172943334103 ) ) ;
#3276 = CARTESIAN_POINT ( 'NONE',  ( 33.72499318558949000, 38.56284415653841791, 47.04930799450051637 ) ) ;
#3277 = EDGE_LOOP ( 'NONE', ( #21025, #10246, #22649, #9532 ) ) ;
#3278 = CIRCLE ( 'NONE', #20052, 12.62506659569710266 ) ;
#3279 = AXIS2_PLACEMENT_3D ( 'NONE', #1148, #31200, #18065 ) ;
#3280 = AXIS2_PLACEMENT_3D ( 'NONE', #27857, #20132, #12438 ) ;
#3281 = ORIENTED_EDGE ( 'NONE', *, *, #3887, .F. ) ;
#3282 = VECTOR ( 'NONE', #14060, 1000.000000000000114 ) ;
#3283 = VERTEX_POINT ( 'NONE', #26155 ) ;
#3284 = DIRECTION ( 'NONE',  ( -0.8746197071393858602, 0.4848096202463547666, 0.000000000000000000 ) ) ;
#3285 = CYLINDRICAL_SURFACE ( 'NONE', #7179, 22.00000000000000000 ) ;
#3286 = CARTESIAN_POINT ( 'NONE',  ( 33.46699938050304013, 28.71183152705961206, 47.04930799450051637 ) ) ;
#3287 = VERTEX_POINT ( 'NONE', #5828 ) ;
#3288 = CARTESIAN_POINT ( 'NONE',  ( -34.35522249183560461, -13.30632128221581389, 39.74351294429737891 ) ) ;
#3289 = CARTESIAN_POINT ( 'NONE',  ( 81.48020857097124292, -5.936921830459689353, 16.01322791396358625 ) ) ;
#3290 = CARTESIAN_POINT ( 'NONE',  ( 99.49785597605720966, -17.03545420775220265, 47.04930799450051637 ) ) ;
#3291 = CARTESIAN_POINT ( 'NONE',  ( 48.15316146078545501, 22.93807716476589320, 48.40645952689865084 ) ) ;
#3292 = EDGE_CURVE ( 'NONE', #7831, #23399, #14353, .T. ) ;
#3293 = CARTESIAN_POINT ( 'NONE',  ( 21.09785597605720042, -13.37218737171702543, 47.04930799450051637 ) ) ;
#3294 = CARTESIAN_POINT ( 'NONE',  ( 21.09992658989239089, 27.46664230456639899, 47.04930799450051637 ) ) ;
#3295 = CARTESIAN_POINT ( 'NONE',  ( 21.09992658989239089, 27.71183152705960850, 47.04930799450051637 ) ) ;
#3296 = EDGE_CURVE ( 'NONE', #23946, #25889, #5451, .T. ) ;
#3298 = EDGE_CURVE ( 'NONE', #26367, #19002, #23535, .T. ) ;
#3297 = CARTESIAN_POINT ( 'NONE',  ( 47.09785597605719687, 24.76454579224779806, 47.04930799450078638 ) ) ;
#3299 = PRODUCT ( 'Magnet', 'Magnet', '', ( #30204 ) ) ;
#3300 = ADVANCED_FACE ( 'NONE', ( #8446 ), #32157, .T. ) ;
#3301 = CYLINDRICAL_SURFACE ( 'NONE', #7374, 2.500000000000002220 ) ;
#3302 = AXIS2_PLACEMENT_3D ( 'NONE', #32289, #11932, #29504 ) ;
#3303 = CARTESIAN_POINT ( 'NONE',  ( 21.09785597605719332, -16.93042895458276575, 47.04930799450051637 ) ) ;
#3304 = EDGE_LOOP ( 'NONE', ( #14921, #19098, #10073, #24712 ) ) ;
#3305 = ORIENTED_EDGE ( 'NONE', *, *, #32444, .T. ) ;
#3306 = CARTESIAN_POINT ( 'NONE',  ( 8.474859994195286461, 30.09184655352422411, 47.04930799450051637 ) ) ;
#3307 = FACE_OUTER_BOUND ( 'NONE', #6013, .T. ) ;
#3308 = DIRECTION ( 'NONE',  ( -1.101824276508909887E-16, 1.000000000000000000, -0.000000000000000000 ) ) ;
#3309 = ORIENTED_EDGE ( 'NONE', *, *, #32473, .F. ) ;
#3310 = CIRCLE ( 'NONE', #21643, 2.500000000000002220 ) ;
#3311 = DIRECTION ( 'NONE',  ( 0.000000000000000000, -9.185193130005556732E-17, 1.000000000000000000 ) ) ;
#3312 = VECTOR ( 'NONE', #28867, 1000.000000000000000 ) ;
#3313 = ORIENTED_EDGE ( 'NONE', *, *, #32207, .T. ) ;
#3314 = CARTESIAN_POINT ( 'NONE',  ( -40.75848109938849717, 9.580021662090986823, 35.54930799450052348 ) ) ;
#3315 = CARTESIAN_POINT ( 'NONE',  ( 47.23302798462060537, 29.28121246473837047, 44.44659793406428605 ) ) ;
#3316 = CARTESIAN_POINT ( 'NONE',  ( 49.49063479933183629, 28.71291119454914664, 47.17357720316391578 ) ) ;
#3317 = CARTESIAN_POINT ( 'NONE',  ( -39.40475928260197946, -5.936129750639523195, 77.92715501466686590 ) ) ;
#3318 = ORIENTED_EDGE ( 'NONE', *, *, #17652, .F. ) ;
#3319 = CIRCLE ( 'NONE', #14866, 65.75844861871132707 ) ;
#3320 = TOROIDAL_SURFACE ( 'NONE', #31565, 12.40141737965284996, 0.1250000000000002776 ) ;
#3321 = DIRECTION ( 'NONE',  ( -1.000000000000000000, 0.000000000000000000, 0.000000000000000000 ) ) ;
#3322 = EDGE_CURVE ( 'NONE', #21428, #30206, #196, .T. ) ;
#3323 = DIRECTION ( 'NONE',  ( -1.000000000000000000, 0.000000000000000000, 0.000000000000000000 ) ) ;
#3324 = EDGE_LOOP ( 'NONE', ( #390, #19888, #25132, #6051 ) ) ;
#3325 = CIRCLE ( 'NONE', #4907, 71.29999999999996874 ) ;
#3326 = CIRCLE ( 'NONE', #11684, 0.1000000000000006301 ) ;
#3327 = VECTOR ( 'NONE', #5269, 999.9999999999998863 ) ;
#3328 = CIRCLE ( 'NONE', #2282, 2.000000000000001776 ) ;
#3329 = DIRECTION ( 'NONE',  ( 0.000000000000000000, 0.000000000000000000, 1.000000000000000000 ) ) ;
#3330 = PLANE ( 'NONE',  #15126 ) ;
#3331 = CARTESIAN_POINT ( 'NONE',  ( -40.76967387488526384, 8.530668925462080665, 39.44930799450052206 ) ) ;
#3332 = ORIENTED_EDGE ( 'NONE', *, *, #6264, .T. ) ;
#3333 = CARTESIAN_POINT ( 'NONE',  ( 75.39785597605721534, 14.56454579224780232, 47.04930799450051637 ) ) ;
#3334 = CARTESIAN_POINT ( 'NONE',  ( -40.59783212598352264, 7.538197204814764518, 53.99316187147203294 ) ) ;
#3336 = EDGE_CURVE ( 'NONE', #26270, #6305, #23780, .T. ) ;
#3335 = DIRECTION ( 'NONE',  ( 0.000000000000000000, 0.000000000000000000, 1.000000000000000000 ) ) ;
#3337 = EDGE_CURVE ( 'NONE', #25278, #286, #24298, .T. ) ;
#3338 = CARTESIAN_POINT ( 'NONE',  ( -2.054138246187894534, 11.56016961077985350, 98.98610059691263530 ) ) ;
#3339 = ADVANCED_FACE ( 'NONE', ( #13058 ), #4378, .F. ) ;
#3340 =( NAMED_UNIT ( * ) PLANE_ANGLE_UNIT ( ) SI_UNIT ( $, .RADIAN. ) );
#3341 = ORIENTED_EDGE ( 'NONE', *, *, #16604, .T. ) ;
#3342 = CARTESIAN_POINT ( 'NONE',  ( 46.77981311948828846, 23.11533908250407165, 46.84298161117587966 ) ) ;
#3343 = CARTESIAN_POINT ( 'NONE',  ( 8.698509210239571132, 30.84164230456639544, 47.04930799450051637 ) ) ;
#3344 = B_SPLINE_CURVE_WITH_KNOTS ( 'NONE', 3,
 ( #1737, #18641, #31775, #11595, #21417, #28665, #21752, #18794, #6179, #24223, #21266, #23738, #31297, #9288 ),
 .UNSPECIFIED., .F., .F.,
 ( 4, 2, 2, 2, 2, 2, 4 ),
 ( 0.0002010756753325377709, 0.001030312595864772912, 0.001444931056130880969, 0.001859549516396989026, 0.002274167976663097300, 0.002688786436929205791, 0.003518023357461414966 ),
 .UNSPECIFIED. ) ;
#3345 = CARTESIAN_POINT ( 'NONE',  ( -15.90214402394279958, 13.86454579224779948, 47.04930799450052348 ) ) ;
#3346 = CARTESIAN_POINT ( 'NONE',  ( -40.11669538345027064, 6.804256812083823824, 34.64773285490134214 ) ) ;
#3347 = DIRECTION ( 'NONE',  ( 0.000000000000000000, 0.000000000000000000, 1.000000000000000000 ) ) ;
#3348 = ORIENTED_EDGE ( 'NONE', *, *, #30107, .F. ) ;
#3349 = DIRECTION ( 'NONE',  ( -0.9996573249755574819, -1.344306794811909066E-16, 0.02617694830786587712 ) ) ;
#3350 = DIRECTION ( 'NONE',  ( -1.000000000000000000, 0.000000000000000000, 0.000000000000000000 ) ) ;
#3351 = DIRECTION ( 'NONE',  ( 0.9612616959383205595, 0.2756373558169932236, -1.660411357259282445E-16 ) ) ;
#3352 = ORIENTED_EDGE ( 'NONE', *, *, #29648, .F. ) ;
#3353 = DIRECTION ( 'NONE',  ( 0.4848096202463430537, 0.8746197071393926326, 9.920727850371700117E-18 ) ) ;
#3354 = DIRECTION ( 'NONE',  ( -1.101824276508909887E-16, 1.000000000000000000, -0.000000000000000000 ) ) ;
#3355 = CARTESIAN_POINT ( 'NONE',  ( -43.64073206722599707, 1.267352857069780736, 39.54930799450052348 ) ) ;
#3356 = CARTESIAN_POINT ( 'NONE',  ( 49.32263122391440646, 8.279996179725067407, -4.396176344842519512 ) ) ;
#3357 = ORIENTED_EDGE ( 'NONE', *, *, #30511, .F. ) ;
#3358 = CARTESIAN_POINT ( 'NONE',  ( 8.732853799281734553, 38.56284415653841791, 47.04930799450051637 ) ) ;
#3359 = ORIENTED_EDGE ( 'NONE', *, *, #32430, .T. ) ;
#3360 = ORIENTED_EDGE ( 'NONE', *, *, #4615, .F. ) ;
#3361 = EDGE_CURVE ( 'NONE', #12208, #15228, #6136, .T. ) ;
#3362 = EDGE_CURVE ( 'NONE', #777, #16797, #18442, .T. ) ;
#3363 = AXIS2_PLACEMENT_3D ( 'NONE', #26945, #4463, #9061 ) ;
#3364 = CARTESIAN_POINT ( 'NONE',  ( -36.76418579970419387, 10.14130568307076352, 56.14611646155296398 ) ) ;
#3365 = FACE_OUTER_BOUND ( 'NONE', #21547, .T. ) ;
#3366 = AXIS2_PLACEMENT_3D ( 'NONE', #9560, #6010, #28811 ) ;
#3367 = CARTESIAN_POINT ( 'NONE',  ( 47.22751897799751220, 27.11988759933318960, 44.55267275764142454 ) ) ;
#3368 = AXIS2_PLACEMENT_3D ( 'NONE', #21853, #6447, #16448 ) ;
#3369 = VERTEX_POINT ( 'NONE', #15662 ) ;
#3370 = ORIENTED_EDGE ( 'NONE', *, *, #21556, .T. ) ;
#3371 = CIRCLE ( 'NONE', #19084, 0.09999999999999795164 ) ;
#3372 = FACE_OUTER_BOUND ( 'NONE', #28614, .T. ) ;
#3373 = CARTESIAN_POINT ( 'NONE',  ( -31.01722238679535337, 5.224609680351743002, 77.52734172137031976 ) ) ;
#3374 = DIRECTION ( 'NONE',  ( -0.000000000000000000, -1.000000000000000000, 0.000000000000000000 ) ) ;
#3375 = ADVANCED_FACE ( 'NONE', ( #23378 ), #25677, .T. ) ;
#3376 = ORIENTED_EDGE ( 'NONE', *, *, #25213, .T. ) ;
#3377 = CARTESIAN_POINT ( 'NONE',  ( -40.45528000798979917, 8.522633796558835684, 34.54930799450052348 ) ) ;
#3378 = EDGE_LOOP ( 'NONE', ( #399, #10481, #30354, #20357 ) ) ;
#3379 = DIRECTION ( 'NONE',  ( 0.000000000000000000, -1.000000000000000000, 0.000000000000000000 ) ) ;
#3380 = CARTESIAN_POINT ( 'NONE',  ( 21.09992658989239089, 30.47145308207317882, 47.04930799450051637 ) ) ;
#3381 = ORIENTED_EDGE ( 'NONE', *, *, #25020, .F. ) ;
#3382 = DIRECTION ( 'NONE',  ( -0.000000000000000000, -1.000000000000000000, -0.000000000000000000 ) ) ;
#3383 = CARTESIAN_POINT ( 'NONE',  ( -35.57732732147984223, 11.39140128989992817, 52.68243506491521799 ) ) ;
#3384 = CARTESIAN_POINT ( 'NONE',  ( -43.95628906790246759, -0.1269931775117038586, 32.04930799450052348 ) ) ;
#3385 = CARTESIAN_POINT ( 'NONE',  ( 21.09785597605720042, -16.73545420775220194, 47.04930799450051637 ) ) ;
#3386 = CARTESIAN_POINT ( 'NONE',  ( 48.94625023931840957, 25.97124452788249371, 46.10640627770150246 ) ) ;
#3387 = VERTEX_POINT ( 'NONE', #11229 ) ;
#3388 = FACE_OUTER_BOUND ( 'NONE', #23219, .T. ) ;
#3389 = VERTEX_POINT ( 'NONE', #30772 ) ;
#3390 = CARTESIAN_POINT ( 'NONE',  ( 47.09785597605719687, 15.77906836436399374, 47.04930799450078638 ) ) ;
#3391 = FACE_OUTER_BOUND ( 'NONE', #18985, .T. ) ;
#3392 = VERTEX_POINT ( 'NONE', #5503 ) ;
#3393 = AXIS2_PLACEMENT_3D ( 'NONE', #22988, #25620, #502 ) ;
#3394 = EDGE_CURVE ( 'NONE', #15480, #14564, #3325, .T. ) ;
#3395 = ORIENTED_EDGE ( 'NONE', *, *, #31507, .F. ) ;
#3396 = CARTESIAN_POINT ( 'NONE',  ( -12.59179267514473821, -3.218976025668840002, 102.6991991216207936 ) ) ;
#3397 = VECTOR ( 'NONE', #7915, 1000.000000000000000 ) ;
#3398 = AXIS2_PLACEMENT_3D ( 'NONE', #26704, #11778, #9309 ) ;
#3399 = TOROIDAL_SURFACE ( 'NONE', #27514, 15.27594751018003194, 0.2551199516247882326 ) ;
#3400 = ADVANCED_FACE ( 'NONE', ( #20590 ), #13812, .T. ) ;
#3401 = AXIS2_PLACEMENT_3D ( 'NONE', #3445, #13629, #5759 ) ;
#3402 = ORIENTED_EDGE ( 'NONE', *, *, #8220, .T. ) ;
#3403 = ADVANCED_FACE ( 'NONE', ( #28954 ), #19237, .T. ) ;
#3404 = EDGE_CURVE ( 'NONE', #6754, #6409, #29438, .T. ) ;
#3405 = ADVANCED_FACE ( 'NONE', ( #6948 ), #11547, .F. ) ;
#3406 = ORIENTED_EDGE ( 'NONE', *, *, #820, .F. ) ;
#3407 = CARTESIAN_POINT ( 'NONE',  ( 71.49893360114317886, -3.295808585244882849, 11.79002343214940041 ) ) ;
#3408 = B_SPLINE_CURVE_WITH_KNOTS ( 'NONE', 3,
 ( #3626, #21171, #31209, #8717, #28427, #30573, #20864, #8087, #5941, #5779, #18397, #25790, #13338, #23335, #846, #10870, #4440, #1481, #21982, #3953, #14296, #16574, #26760, #11834, #9366, #16418, #13974, #14461, #23965, #9038, #4280, #31850, #11497, #26279 ),
 .UNSPECIFIED., .F., .F.,
 ( 4, 2, 2, 2, 2, 2, 2, 2, 2, 2, 2, 2, 2, 2, 2, 2, 4 ),
 ( 0.5000000000000000000, 0.5312500000000000000, 0.5625000000000000000, 0.5937500000000000000, 0.6250000000000000000, 0.6562500000000000000, 0.6875000000000001110, 0.7187500000000002220, 0.7500000000000002220, 0.7812500000000002220, 0.8125000000000002220, 0.8437500000000002220, 0.8750000000000002220, 0.9062500000000002220, 0.9375000000000001110, 0.9687500000000000000, 1.000000000000000000 ),
 .UNSPECIFIED. ) ;
#3409 = VERTEX_POINT ( 'NONE', #1527 ) ;
#3410 = CIRCLE ( 'NONE', #12335, 12.36707279061065101 ) ;
#3411 =( BOUNDED_CURVE ( )  B_SPLINE_CURVE ( 3, ( #31654, #4238, #26715, #9317 ),
 .UNSPECIFIED., .F., .F. ) 
 B_SPLINE_CURVE_WITH_KNOTS ( ( 4, 4 ),
 ( 1.570796326794888342, 1.630650672327995210 ),
 .UNSPECIFIED. ) 
 CURVE ( )  GEOMETRIC_REPRESENTATION_ITEM ( )  RATIONAL_B_SPLINE_CURVE ( ( 1.000000000000000000, 0.9997014770583808607, 0.9997014770583808607, 1.000000000000000000 ) ) 
 REPRESENTATION_ITEM ( '' )  );
#3412 = DIRECTION ( 'NONE',  ( 0.9612616959383205595, 0.2756373558169932236, -1.660411357259282445E-16 ) ) ;
#3413 = CYLINDRICAL_SURFACE ( 'NONE', #26900, 2.499999999999997335 ) ;
#3414 = CIRCLE ( 'NONE', #18103, 58.46397533894063514 ) ;
#3415 = CARTESIAN_POINT ( 'NONE',  ( 44.74832014356462651, 28.38456182964376495, 46.92728461490987257 ) ) ;
#3416 = ADVANCED_FACE ( 'NONE', ( #2018 ), #26377, .T. ) ;
#3417 = ORIENTED_EDGE ( 'NONE', *, *, #24032, .T. ) ;
#3418 = ORIENTED_EDGE ( 'NONE', *, *, #4412, .T. ) ;
#3419 = FACE_OUTER_BOUND ( 'NONE', #19613, .T. ) ;
#3420 = CIRCLE ( 'NONE', #23346, 20.58349629884742882 ) ;
#3421 = ORIENTED_EDGE ( 'NONE', *, *, #5597, .T. ) ;
#3422 = CARTESIAN_POINT ( 'NONE',  ( -43.37834615508418068, 1.121909970995877082, 39.44930799450052916 ) ) ;
#3423 = AXIS2_PLACEMENT_3D ( 'NONE', #16638, #4015, #27148 ) ;
#3424 = CARTESIAN_POINT ( 'NONE',  ( 49.32092071431622315, 8.281585831149220311, 98.49472633489467910 ) ) ;
#3425 = FACE_OUTER_BOUND ( 'NONE', #1946, .T. ) ;
#3426 = CARTESIAN_POINT ( 'NONE',  ( 48.35473289974375177, 22.86454579224779948, 45.11188864597616544 ) ) ;
#3427 = ORIENTED_EDGE ( 'NONE', *, *, #16067, .F. ) ;
#3428 = DIRECTION ( 'NONE',  ( -1.000000000000000000, 0.000000000000000000, 0.000000000000000000 ) ) ;
#3429 = FACE_OUTER_BOUND ( 'NONE', #7693, .T. ) ;
#3430 = DIRECTION ( 'NONE',  ( 0.000000000000000000, -0.000000000000000000, -1.000000000000000000 ) ) ;
#3431 = CARTESIAN_POINT ( 'NONE',  ( -6.902144023942789808, 13.86454579224779948, 47.04930799450052348 ) ) ;
#3432 = CARTESIAN_POINT ( 'NONE',  ( 21.09785597605720753, 17.36467600858027183, 47.04930799450052348 ) ) ;
#3433 = EDGE_CURVE ( 'NONE', #18578, #20832, #31415, .T. ) ;
#3434 = ORIENTED_EDGE ( 'NONE', *, *, #5360, .T. ) ;
#3435 = FACE_OUTER_BOUND ( 'NONE', #7203, .T. ) ;
#3436 = CARTESIAN_POINT ( 'NONE',  ( -40.50726676055793973, 7.559560307024990600, 53.80788663826320573 ) ) ;
#3437 =( REPRESENTATION_RELATIONSHIP ('NONE','NONE', #20382, #17018 ) REPRESENTATION_RELATIONSHIP_WITH_TRANSFORMATION ( #22643 )SHAPE_REPRESENTATION_RELATIONSHIP( ) );
#3438 = ADVANCED_FACE ( 'NONE', ( #11714 ), #16616, .F. ) ;
#3439 = VERTEX_POINT ( 'NONE', #31738 ) ;
#3440 = AXIS2_PLACEMENT_3D ( 'NONE', #29927, #10380, #12364 ) ;
#3441 = COLOUR_RGB ( '',0.7921568627450980005, 0.8196078431372548767, 0.9333333333333333481 ) ;
#3442 = EDGE_CURVE ( 'NONE', #3984, #15332, #16746, .T. ) ;
#3443 = ADVANCED_FACE ( 'NONE', ( #6298 ), #14015, .T. ) ;
#3444 = VERTEX_POINT ( 'NONE', #6783 ) ;
#3445 = CARTESIAN_POINT ( 'NONE',  ( -40.41018466243807694, 8.365367637131765122, 40.47149053519531492 ) ) ;
#3446 = CARTESIAN_POINT ( 'NONE',  ( -44.97602486328538163, -5.513888518307795472, 52.81728120461330889 ) ) ;
#3447 = DIRECTION ( 'NONE',  ( -1.101824276508909887E-16, 1.000000000000000000, -0.000000000000000000 ) ) ;
#3448 = CIRCLE ( 'NONE', #12899, 0.1000000000000004774 ) ;
#3449 = ORIENTED_EDGE ( 'NONE', *, *, #27458, .F. ) ;
#3450 = CARTESIAN_POINT ( 'NONE',  ( -15.78477032795855273, -13.30632128221581034, 5.000640598253890623 ) ) ;
#3451 = CARTESIAN_POINT ( 'NONE',  ( 81.47887257101615432, -5.936379232154268770, 15.96372277398939588 ) ) ;
#3452 = DIRECTION ( 'NONE',  ( 0.000000000000000000, 0.9550631830612811290, 0.2964022880492887535 ) ) ;
#3453 = ORIENTED_EDGE ( 'NONE', *, *, #12042, .F. ) ;
#3454 = DIRECTION ( 'NONE',  ( 0.000000000000000000, 0.000000000000000000, 1.000000000000000000 ) ) ;
#3455 = ORIENTED_EDGE ( 'NONE', *, *, #20389, .T. ) ;
#3456 = CARTESIAN_POINT ( 'NONE',  ( -43.29088418437023478, 1.073429008971242382, 34.64930799450052490 ) ) ;
#3457 = FACE_OUTER_BOUND ( 'NONE', #20170, .T. ) ;
#3458 = CARTESIAN_POINT ( 'NONE',  ( 46.37506696020427910, 29.22387735013030152, 44.70869714466342515 ) ) ;
#3459 = DIRECTION ( 'NONE',  ( 0.2756373558169932236, -0.9612616959383204485, 1.479773560108267395E-16 ) ) ;
#3460 = CARTESIAN_POINT ( 'NONE',  ( 33.50134396954526039, 25.59164230456639899, 47.04930799450051637 ) ) ;
#3461 = FILL_AREA_STYLE_COLOUR ( '', #24962 ) ;
#3462 = EDGE_LOOP ( 'NONE', ( #11825, #22006, #19417, #25704 ) ) ;
#3463 = VERTEX_POINT ( 'NONE', #1859 ) ;
#3464 = CARTESIAN_POINT ( 'NONE',  ( 21.09785597605719332, 25.56454579224779877, 49.97284587932492883 ) ) ;
#3465 = AXIS2_PLACEMENT_3D ( 'NONE', #24622, #14945, #2790 ) ;
#3466 = PRESENTATION_LAYER_ASSIGNMENT (  '', '', ( #24430 ) ) ;
#3467 = CYLINDRICAL_SURFACE ( 'NONE', #16188, 12.36707279061065101 ) ;
#3468 = CARTESIAN_POINT ( 'NONE',  ( 21.09785597605720042, -9.935454207752199451, 115.0493079945004951 ) ) ;
#3469 = ORIENTED_EDGE ( 'NONE', *, *, #6527, .F. ) ;
#3470 = CARTESIAN_POINT ( 'NONE',  ( -42.12525683681430877, 14.70933063813549424, 35.90717268343339441 ) ) ;
#3471 = FACE_OUTER_BOUND ( 'NONE', #4263, .T. ) ;
#3472 = ORIENTED_EDGE ( 'NONE', *, *, #28398, .T. ) ;
#3473 = LINE ( 'NONE', #13344, #15733 ) ;
#3474 = CARTESIAN_POINT ( 'NONE',  ( 47.23302798462060537, 28.58121246473837118, 44.44659793406428605 ) ) ;
#3475 = AXIS2_PLACEMENT_3D ( 'NONE', #22053, #1542, #21886 ) ;
#3476 = DIRECTION ( 'NONE',  ( -0.6184495258776654403, 0.3428121700606547861, -0.7071067811865443531 ) ) ;
#3477 = EDGE_CURVE ( 'NONE', #18541, #2754, #20404, .T. ) ;
#3478 = ORIENTED_EDGE ( 'NONE', *, *, #24071, .F. ) ;
#3479 = ADVANCED_FACE ( 'NONE', ( #18752 ), #16304, .F. ) ;
#3480 = CARTESIAN_POINT ( 'NONE',  ( 52.07077173907278933, -5.935668157269684109, -13.53804821299738492 ) ) ;
#3481 = AXIS2_PLACEMENT_3D ( 'NONE', #10835, #30852, #3428 ) ;
#3482 = CARTESIAN_POINT ( 'NONE',  ( 21.09785597605719332, -15.93545420775219945, 47.04930799450051637 ) ) ;
#3483 = VERTEX_POINT ( 'NONE', #19076 ) ;
#3484 = CARTESIAN_POINT ( 'NONE',  ( 44.87087493598345134, 26.77587066347689415, 48.18533415931919706 ) ) ;
#3485 = CARTESIAN_POINT ( 'NONE',  ( -41.94956971822180947, 3.905757428664828890, 47.04930799450051637 ) ) ;
#3486 = DIRECTION ( 'NONE',  ( 0.000000000000000000, 1.000000000000000000, 0.000000000000000000 ) ) ;
#3487 = AXIS2_PLACEMENT_3D ( 'NONE', #20010, #12151, #7709 ) ;
#3488 = ORIENTED_EDGE ( 'NONE', *, *, #4254, .F. ) ;
#3489 = CARTESIAN_POINT ( 'NONE',  ( -25.43703420551703687, 14.16454579224779842, 47.04930799450052348 ) ) ;
#3490 = CARTESIAN_POINT ( 'NONE',  ( -42.28301147118429526, 15.25948642862022986, 38.44930799450052206 ) ) ;
#3491 = DIRECTION ( 'NONE',  ( 1.234978253042719660E-16, -1.000000000000000000, -1.109335647967047851E-31 ) ) ;
#3492 = PRODUCT_RELATED_PRODUCT_CATEGORY ( 'part', '', ( #7202 ) ) ;
#3493 = CARTESIAN_POINT ( 'NONE',  ( -5.145516081992131951, 10.07216359114295479, 98.42132851406103100 ) ) ;
#3494 = CARTESIAN_POINT ( 'NONE',  ( 0.000000000000000000, 0.000000000000000000, 0.000000000000000000 ) ) ;
#3495 = ORIENTED_EDGE ( 'NONE', *, *, #7611, .F. ) ;
#3496 = DIRECTION ( 'NONE',  ( -1.101824276508909887E-16, 1.000000000000000000, -0.000000000000000000 ) ) ;
#3497 = CARTESIAN_POINT ( 'NONE',  ( 48.40186567930498285, 29.52957786121581663, 45.03923535223908203 ) ) ;
#3498 = CARTESIAN_POINT ( 'NONE',  ( -40.38492706200820948, 8.640065911210484728, 34.64831079233957212 ) ) ;
#3499 = FACE_OUTER_BOUND ( 'NONE', #11549, .T. ) ;
#3500 = DIRECTION ( 'NONE',  ( 0.000000000000000000, 0.000000000000000000, -1.000000000000000000 ) ) ;
#3501 = ORIENTED_EDGE ( 'NONE', *, *, #25610, .F. ) ;
#3502 = CARTESIAN_POINT ( 'NONE',  ( 21.09992658989239089, 27.09143805560860940, 47.04930799450051637 ) ) ;
#3503 = CARTESIAN_POINT ( 'NONE',  ( 21.09992658989238734, 38.56284415653841791, 47.04930799450051637 ) ) ;
#3504 = CARTESIAN_POINT ( 'NONE',  ( 21.09992658989239089, 24.21183152705959785, 47.04930799450051637 ) ) ;
#3505 = ORIENTED_EDGE ( 'NONE', *, *, #24683, .T. ) ;
#3506 = DIRECTION ( 'NONE',  ( 0.8746197071393926326, -0.4848096202463430537, -8.676864087101709653E-18 ) ) ;
#3507 = DIRECTION ( 'NONE',  ( 0.9612616959383205595, 0.2756373558169932236, -1.660411357259282445E-16 ) ) ;
#3508 = AXIS2_PLACEMENT_3D ( 'NONE', #7108, #11871, #4484 ) ;
#3509 = LINE ( 'NONE', #23539, #16210 ) ;
#3510 = LINE ( 'NONE', #891, #2281 ) ;
#3511 = VERTEX_POINT ( 'NONE', #3833 ) ;
#3512 = CARTESIAN_POINT ( 'NONE',  ( -40.58856461370174173, 7.499380836222960589, 60.14930799450051779 ) ) ;
#3513 = ORIENTED_EDGE ( 'NONE', *, *, #25758, .T. ) ;
#3514 = B_SPLINE_CURVE_WITH_KNOTS ( 'NONE', 3,
 ( #400, #8604, #28151, #10600, #30616, #31095, #8128, #10759 ),
 .UNSPECIFIED., .F., .F.,
 ( 4, 2, 2, 4 ),
 ( 0.000000000000000000, 0.0002680696438040274616, 0.0005361392876080549232, 0.001072278575216109846 ),
 .UNSPECIFIED. ) ;
#3515 = VERTEX_POINT ( 'NONE', #16463 ) ;
#3516 = ADVANCED_FACE ( 'NONE', ( #14340 ), #2089, .T. ) ;
#3517 = EDGE_CURVE ( 'NONE', #31078, #18206, #13625, .T. ) ;
#3518 = EDGE_CURVE ( 'NONE', #25493, #16293, #19371, .T. ) ;
#3519 = EDGE_CURVE ( 'NONE', #13529, #23253, #4154, .T. ) ;
#3520 = EDGE_CURVE ( 'NONE', #2165, #20059, #21994, .T. ) ;
#3521 = VECTOR ( 'NONE', #18862, 1000.000000000000114 ) ;
#3522 = AXIS2_PLACEMENT_3D ( 'NONE', #9220, #1341, #11357 ) ;
#3523 = CARTESIAN_POINT ( 'NONE',  ( 33.46699938050304013, 28.22145308207318237, 47.04930799450050927 ) ) ;
#3524 = FACE_OUTER_BOUND ( 'NONE', #14074, .T. ) ;
#3525 = CARTESIAN_POINT ( 'NONE',  ( -40.70335362822509495, 9.387769322903324110, 34.54930799450052348 ) ) ;
#3526 = VECTOR ( 'NONE', #1326, 1000.000000000000114 ) ;
#3527 = ORIENTED_EDGE ( 'NONE', *, *, #27906, .T. ) ;
#3528 = CARTESIAN_POINT ( 'NONE',  ( -43.29088418437023478, 1.073429008971243492, 39.54930799450052348 ) ) ;
#3529 = ORIENTED_EDGE ( 'NONE', *, *, #7650, .F. ) ;
#3530 = CARTESIAN_POINT ( 'NONE',  ( 45.84097905237065618, 19.96454579224779380, 48.98672734302541443 ) ) ;
#3531 = DIRECTION ( 'NONE',  ( 0.000000000000000000, 1.000000000000000000, -0.000000000000000000 ) ) ;
#3532 = CARTESIAN_POINT ( 'NONE',  ( 21.09785597605719332, 25.56454579224779877, 47.04930799450051637 ) ) ;
#3533 = CIRCLE ( 'NONE', #26076, 12.62506659569710443 ) ;
#3534 = DIRECTION ( 'NONE',  ( -1.101824276508909887E-16, 1.000000000000000000, -0.000000000000000000 ) ) ;
#3535 = ORIENTED_EDGE ( 'NONE', *, *, #30269, .F. ) ;
#3536 = FACE_OUTER_BOUND ( 'NONE', #12646, .T. ) ;
#3537 = ORIENTED_EDGE ( 'NONE', *, *, #24064, .F. ) ;
#3538 = CARTESIAN_POINT ( 'NONE',  ( -43.38408989745150990, 1.111547985471239786, 60.44930799450051495 ) ) ;
#3539 = CARTESIAN_POINT ( 'NONE',  ( 46.04844006429464542, 22.80400562401889530, 44.99211097489548905 ) ) ;
#3540 = ORIENTED_EDGE ( 'NONE', *, *, #15853, .F. ) ;
#3541 = CARTESIAN_POINT ( 'NONE',  ( -42.38687957179149635, 4.148162238787999279, 38.94930799450052206 ) ) ;
#3542 = DIRECTION ( 'NONE',  ( 0.9612616959383164517, 0.2756373558170082116, -1.660411357259305371E-16 ) ) ;
#3543 = CIRCLE ( 'NONE', #21348, 0.1250000000000001110 ) ;
#3544 = CARTESIAN_POINT ( 'NONE',  ( 21.09785597605717555, 77.37241625295546044, 131.0041668858331150 ) ) ;
#3545 = CARTESIAN_POINT ( 'NONE',  ( 49.49063479933183629, 25.91291119454915304, 47.17357720316391578 ) ) ;
#3546 = ORIENTED_EDGE ( 'NONE', *, *, #16556, .T. ) ;
#3547 = CARTESIAN_POINT ( 'NONE',  ( 21.09992658989238734, 30.71183152705961916, 47.04930799450051637 ) ) ;
#3548 = CYLINDRICAL_SURFACE ( 'NONE', #13332, 0.1000000000000018235 ) ;
#3549 = VERTEX_POINT ( 'NONE', #22696 ) ;
#3551 = EDGE_CURVE ( 'NONE', #2570, #29229, #21449, .T. ) ;
#3550 = DIRECTION ( 'NONE',  ( -0.000000000000000000, -1.000000000000000000, -0.000000000000000000 ) ) ;
#3552 = CARTESIAN_POINT ( 'NONE',  ( -9.970446611220443955, -5.937394852768786535, -13.32263710021335612 ) ) ;
#3553 = VERTEX_POINT ( 'NONE', #22523 ) ;
#3554 = VERTEX_POINT ( 'NONE', #19901 ) ;
#3555 = CARTESIAN_POINT ( 'NONE',  ( -6.244038915535443657, 9.161285963347376438, 98.41684214693681554 ) ) ;
#3556 = VECTOR ( 'NONE', #1616, 1000.000000000000000 ) ;
#3557 = PRODUCT_DEFINITION_CONTEXT ( 'detailed design', #20836, 'design' ) ;
#3558 = CIRCLE ( 'NONE', #21366, 0.09999999999999939493 ) ;
#3559 = VERTEX_POINT ( 'NONE', #10230 ) ;
#3560 = AXIS2_PLACEMENT_3D ( 'NONE', #9657, #24583, #9496 ) ;
#3561 = ADVANCED_FACE ( 'NONE', ( #9901 ), #14143, .T. ) ;
#3562 = CIRCLE ( 'NONE', #29798, 0.1000000000000027811 ) ;
#3563 = ORIENTED_EDGE ( 'NONE', *, *, #8136, .T. ) ;
#3564 = FACE_OUTER_BOUND ( 'NONE', #24438, .T. ) ;
#3565 = ORIENTED_EDGE ( 'NONE', *, *, #9477, .F. ) ;
#3566 = FACE_OUTER_BOUND ( 'NONE', #20244, .T. ) ;
#3567 = CARTESIAN_POINT ( 'NONE',  ( 21.09992658989239089, 27.59164230456639544, 47.04930799450051637 ) ) ;
#3568 = CARTESIAN_POINT ( 'NONE',  ( 52.31247960063809899, -5.928581419070744651, 106.5177822622708703 ) ) ;
#3569 = EDGE_CURVE ( 'NONE', #29858, #2915, #25326, .T. ) ;
#3570 = CARTESIAN_POINT ( 'NONE',  ( 48.37829923888483563, 25.35122849631043351, 45.07556196625585443 ) ) ;
#3571 = ORIENTED_EDGE ( 'NONE', *, *, #22749, .F. ) ;
#3572 = VECTOR ( 'NONE', #23189, 1000.000000000000000 ) ;
#3573 = EDGE_LOOP ( 'NONE', ( #10658, #5418, #25603, #19859 ) ) ;
#3574 = DIRECTION ( 'NONE',  ( 0.4848096202463427762, 0.8746197071393925215, -2.220446049250312588E-16 ) ) ;
#3575 = ORIENTED_EDGE ( 'NONE', *, *, #17900, .F. ) ;
#3576 = EDGE_CURVE ( 'NONE', #286, #16387, #9579, .T. ) ;
#3577 = CIRCLE ( 'NONE', #26122, 4.200000000000000178 ) ;
#3578 = CARTESIAN_POINT ( 'NONE',  ( -40.56500720768295309, 7.149487417332511363, 38.92324275860853078 ) ) ;
#3579 = CARTESIAN_POINT ( 'NONE',  ( -40.68422973805265030, 6.807290781432339344, 39.32248954417796227 ) ) ;
#3580 = FACE_OUTER_BOUND ( 'NONE', #11296, .T. ) ;
#3581 = AXIS2_PLACEMENT_3D ( 'NONE', #8277, #28146, #10753 ) ;
#3582 = VECTOR ( 'NONE', #13741, 1000.000000000000227 ) ;
#3583 = CARTESIAN_POINT ( 'NONE',  ( 46.04844006429464542, 22.86454579224779948, 44.99211097489548905 ) ) ;
#3584 = FACE_OUTER_BOUND ( 'NONE', #23361, .T. ) ;
#3585 = ITEM_DEFINED_TRANSFORMATION ( 'NONE', 'NONE', #11323,  #8172 ) ;
#3586 = VERTEX_POINT ( 'NONE', #2676 ) ;
#3587 = DIRECTION ( 'NONE',  ( -0.000000000000000000, -1.000000000000000000, -0.000000000000000000 ) ) ;
#3589 = EDGE_CURVE ( 'NONE', #4416, #28214, #7280, .T. ) ;
#3588 = CARTESIAN_POINT ( 'NONE',  ( -34.34161333937292682, -4.095223881812850131, 13.61950888151727312 ) ) ;
#3590 = LINE ( 'NONE', #6218, #24504 ) ;
#3591 = ADVANCED_FACE ( 'NONE', ( #27785 ), #12707, .F. ) ;
#3592 = AXIS2_PLACEMENT_3D ( 'NONE', #8090, #12855, #17925 ) ;
#3593 = CARTESIAN_POINT ( 'NONE',  ( 47.54376155772514778, 23.10527865767145528, 46.66768365041815514 ) ) ;
#3594 = CYLINDRICAL_SURFACE ( 'NONE', #27750, 12.62506659569710266 ) ;
#3595 = CARTESIAN_POINT ( 'NONE',  ( 21.09992658989238734, 38.56284415653841791, 47.04930799450051637 ) ) ;
#3596 = ORIENTED_EDGE ( 'NONE', *, *, #25354, .T. ) ;
#3597 = DIRECTION ( 'NONE',  ( -0.000000000000000000, -1.000000000000000000, 0.000000000000000000 ) ) ;
#3598 = DIRECTION ( 'NONE',  ( -1.101824276508909887E-16, 1.000000000000000000, -0.000000000000000000 ) ) ;
#3599 = ORIENTED_EDGE ( 'NONE', *, *, #19250, .F. ) ;
#3600 = EDGE_CURVE ( 'NONE', #28668, #15332, #31965, .T. ) ;
#3601 = AXIS2_PLACEMENT_3D ( 'NONE', #32164, #24117, #9676 ) ;
#3602 = AXIS2_PLACEMENT_3D ( 'NONE', #4162, #14189, #1211 ) ;
#3603 = CIRCLE ( 'NONE', #20350, 58.09216821878681003 ) ;
#3604 = SHAPE_REPRESENTATION ( 'Frame', ( #8172 ), #19670 ) ;
#3605 = ORIENTED_EDGE ( 'NONE', *, *, #22293, .F. ) ;
#3606 = CYLINDRICAL_SURFACE ( 'NONE', #7617, 0.1000000000000006301 ) ;
#3607 = CARTESIAN_POINT ( 'NONE',  ( 21.09992658989239089, 24.34143805560860940, 47.04930799450051637 ) ) ;
#3608 = DIRECTION ( 'NONE',  ( -1.000000000000000000, 0.000000000000000000, 0.000000000000000000 ) ) ;
#3609 = AXIS2_PLACEMENT_3D ( 'NONE', #10434, #4734, #12129 ) ;
#3610 = ORIENTED_EDGE ( 'NONE', *, *, #1336, .F. ) ;
#3611 = CARTESIAN_POINT ( 'NONE',  ( -12.94741462430177315, -13.30632128221581389, 2.672082950226038367 ) ) ;
#3612 = DIRECTION ( 'NONE',  ( -1.101824276508909887E-16, 1.000000000000000000, -0.000000000000000000 ) ) ;
#3613 = CARTESIAN_POINT ( 'NONE',  ( 47.86511985000206693, 22.93807716476589320, 48.55339511290479493 ) ) ;
#3614 = EDGE_CURVE ( 'NONE', #7068, #14556, #5138, .T. ) ;
#3615 = ORIENTED_EDGE ( 'NONE', *, *, #29434, .T. ) ;
#3616 = CARTESIAN_POINT ( 'NONE',  ( 21.09992658989238734, 38.56284415653841791, 47.04930799450051637 ) ) ;
#3617 = ORIENTED_EDGE ( 'NONE', *, *, #4028, .T. ) ;
#3618 = EDGE_CURVE ( 'NONE', #18804, #31321, #17268, .T. ) ;
#3619 = CARTESIAN_POINT ( 'NONE',  ( -39.58809650894544774, 2.596771453999702661, 48.94930799450051495 ) ) ;
#3620 = DIRECTION ( 'NONE',  ( 0.000000000000000000, 0.000000000000000000, -1.000000000000000000 ) ) ;
#3621 = DIRECTION ( 'NONE',  ( 0.000000000000000000, 0.000000000000000000, -1.000000000000000000 ) ) ;
#3622 = SPHERICAL_SURFACE ( 'NONE', #17842, 0.1000000000000000056 ) ;
#3623 = ORIENTED_EDGE ( 'NONE', *, *, #6150, .T. ) ;
#3624 = VERTEX_POINT ( 'NONE', #9744 ) ;
#3625 = APPLICATION_CONTEXT ( 'automotive_design' ) ;
#3626 = CARTESIAN_POINT ( 'NONE',  ( 21.09785597605719687, -13.30631372918550959, 102.8621366805641770 ) ) ;
#3627 = AXIS2_PLACEMENT_3D ( 'NONE', #30311, #27846, #22258 ) ;
#3628 = DIRECTION ( 'NONE',  ( 0.000000000000000000, -0.000000000000000000, -1.000000000000000000 ) ) ;
#3629 = EDGE_CURVE ( 'NONE', #27949, #20704, #24670, .T. ) ;
#3630 = AXIS2_PLACEMENT_3D ( 'NONE', #19080, #3507, #13857 ) ;
#3631 = EDGE_CURVE ( 'NONE', #13895, #27622, #17605, .T. ) ;
#3632 = CARTESIAN_POINT ( 'NONE',  ( -10.74933306299440083, -5.721341737285946749, 105.3592130793008721 ) ) ;
#3633 = ORIENTED_EDGE ( 'NONE', *, *, #5533, .T. ) ;
#3634 = DIRECTION ( 'NONE',  ( -1.000000000000000000, -1.101824276508909887E-16, 0.000000000000000000 ) ) ;
#3635 = CARTESIAN_POINT ( 'NONE',  ( 49.98072202819531640, 28.34488759933318747, 47.19902993264913960 ) ) ;
#3636 = ORIENTED_EDGE ( 'NONE', *, *, #13642, .F. ) ;
#3637 = CARTESIAN_POINT ( 'NONE',  ( -40.61463551858322063, 9.441168033762318501, 34.67959690138647488 ) ) ;
#3638 = CARTESIAN_POINT ( 'NONE',  ( 45.24946171279598417, 25.00784706826093640, 47.99220971130007030 ) ) ;
#3639 = AXIS2_PLACEMENT_3D ( 'NONE', #11718, #21544, #23859 ) ;
#3640 = DIRECTION ( 'NONE',  ( -3.761114140369701376E-15, -1.000000000000000000, 0.000000000000000000 ) ) ;
#3641 = CIRCLE ( 'NONE', #32489, 2.500000000000002220 ) ;
#3642 = ORIENTED_EDGE ( 'NONE', *, *, #31100, .T. ) ;
#3643 = CYLINDRICAL_SURFACE ( 'NONE', #21914, 12.36707279061065101 ) ;
#3644 = SPHERICAL_SURFACE ( 'NONE', #7897, 0.1000000000000000056 ) ;
#3645 = LINE ( 'NONE', #25811, #24845 ) ;
#3646 = AXIS2_PLACEMENT_3D ( 'NONE', #14142, #1980, #27092 ) ;
#3647 = ORIENTED_EDGE ( 'NONE', *, *, #21276, .F. ) ;
#3648 = DIRECTION ( 'NONE',  ( -1.000000000000000000, 0.000000000000000000, 0.000000000000000000 ) ) ;
#3649 = CARTESIAN_POINT ( 'NONE',  ( 21.09785597605719332, 24.86454579224779948, 73.04930799450052348 ) ) ;
#3650 = ADVANCED_FACE ( 'NONE', ( #30253 ), #6265, .T. ) ;
#3651 = CARTESIAN_POINT ( 'NONE',  ( 71.60181765360115946, 8.510833471476306755, 19.03915849818731232 ) ) ;
#3652 = TOROIDAL_SURFACE ( 'NONE', #15709, 1.299999999999999822, 0.1000000000000000056 ) ;
#3653 = ORIENTED_EDGE ( 'NONE', *, *, #429, .T. ) ;
#3654 = AXIS2_PLACEMENT_3D ( 'NONE', #24340, #4001, #31900 ) ;
#3655 = DIRECTION ( 'NONE',  ( -1.000000000000000000, 0.000000000000000000, 0.000000000000000000 ) ) ;
#3656 = CARTESIAN_POINT ( 'NONE',  ( 21.09785597605719332, 11.92558985988973497, 47.04930799450051637 ) ) ;
#3657 = CIRCLE ( 'NONE', #19947, 12.36707279061065101 ) ;
#3658 = CYLINDRICAL_SURFACE ( 'NONE', #9530, 10.00000000000000178 ) ;
#3659 = AXIS2_PLACEMENT_3D ( 'NONE', #20627, #13096, #8164 ) ;
#3660 = FILL_AREA_STYLE_COLOUR ( '', #1333 ) ;
#3661 = VERTEX_POINT ( 'NONE', #22361 ) ;
#3662 = AXIS2_PLACEMENT_3D ( 'NONE', #736, #2714, #20752 ) ;
#3663 = CARTESIAN_POINT ( 'NONE',  ( 8.732853799281734553, 38.56284415653841791, 47.04930799450051637 ) ) ;
#3664 = CARTESIAN_POINT ( 'NONE',  ( 48.94625023931840246, 28.07124452788248803, 46.10640627770149536 ) ) ;
#3665 = DIRECTION ( 'NONE',  ( -1.101824276508909887E-16, 1.000000000000000000, -0.000000000000000000 ) ) ;
#3666 = EDGE_CURVE ( 'NONE', #17152, #7388, #17536, .T. ) ;
#3667 = CARTESIAN_POINT ( 'NONE',  ( -40.28779227465695101, 2.984619150196775372, 35.04930799450051637 ) ) ;
#3668 = DIRECTION ( 'NONE',  ( 0.8746197071393926326, -0.4848096202463430537, -8.676864087101709653E-18 ) ) ;
#3669 = ORIENTED_EDGE ( 'NONE', *, *, #371, .T. ) ;
#3670 = CYLINDRICAL_SURFACE ( 'NONE', #10858, 0.1000000000000028644 ) ;
#3671 = CARTESIAN_POINT ( 'NONE',  ( 49.68665970317314873, 24.91671509559730069, 46.58149026817019944 ) ) ;
#3672 = CARTESIAN_POINT ( 'NONE',  ( -41.74593813222361405, 15.43463958587387808, 35.54930799450051637 ) ) ;
#3673 = VERTEX_POINT ( 'NONE', #25483 ) ;
#3674 = DIRECTION ( 'NONE',  ( 0.2756373558170093774, -0.9612616959383158965, 3.469446951953606616E-14 ) ) ;
#3675 = CIRCLE ( 'NONE', #3152, 70.59901951359279337 ) ;
#3676 = LINE ( 'NONE', #3355, #31966 ) ;
#3677 = DIRECTION ( 'NONE',  ( -1.101824276508909887E-16, 1.000000000000000000, -0.000000000000000000 ) ) ;
#3678 = ORIENTED_EDGE ( 'NONE', *, *, #30035, .T. ) ;
#3679 = VERTEX_POINT ( 'NONE', #23179 ) ;
#3680 = AXIS2_PLACEMENT_3D ( 'NONE', #5413, #15417, #25429 ) ;
#3681 = AXIS2_PLACEMENT_3D ( 'NONE', #15156, #32392, #29939 ) ;
#3682 = VERTEX_POINT ( 'NONE', #23340 ) ;
#3683 = AXIS2_PLACEMENT_3D ( 'NONE', #24617, #21661, #27237 ) ;
#3684 = PRODUCT_RELATED_PRODUCT_CATEGORY ( 'part', '', ( #19779 ) ) ;
#3685 = AXIS2_PLACEMENT_3D ( 'NONE', #26675, #26190, #1237 ) ;
#3686 = AXIS2_PLACEMENT_3D ( 'NONE', #10722, #30256, #30584 ) ;
#3687 = TOROIDAL_SURFACE ( 'NONE', #25729, 12.40141737965283930, 0.1250000000000007216 ) ;
#3688 = CARTESIAN_POINT ( 'NONE',  ( 21.09785597605720753, 13.61454579224779771, 47.04930799450052348 ) ) ;
#3689 = CARTESIAN_POINT ( 'NONE',  ( -36.06597331586808508, -5.586840335632118126, 79.16021068330404376 ) ) ;
#3690 = CARTESIAN_POINT ( 'NONE',  ( 48.04075769285628894, 25.18284706826092290, 48.89770225776209145 ) ) ;
#3691 = AXIS2_PLACEMENT_3D ( 'NONE', #5934, #840, #25627 ) ;
#3692 = ORIENTED_EDGE ( 'NONE', *, *, #5002, .F. ) ;
#3693 = LINE ( 'NONE', #3528, #6700 ) ;
#3694 = VERTEX_POINT ( 'NONE', #20712 ) ;
#3695 = DIRECTION ( 'NONE',  ( -1.000000000000000000, 0.000000000000000000, 0.000000000000000000 ) ) ;
#3696 = DIRECTION ( 'NONE',  ( -1.101824276508909887E-16, 1.000000000000000000, -0.000000000000000000 ) ) ;
#3697 = LINE ( 'NONE', #13724, #29945 ) ;
#3698 = ORIENTED_EDGE ( 'NONE', *, *, #20818, .F. ) ;
#3699 = CARTESIAN_POINT ( 'NONE',  ( 8.698509210239565803, 29.84164230456639899, 47.04930799450051637 ) ) ;
#3700 = CARTESIAN_POINT ( 'NONE',  ( -39.81647664150466426, 8.705807714305638711, 34.54930799450052348 ) ) ;
#3701 = CARTESIAN_POINT ( 'NONE',  ( -40.13606231985500017, 7.635531802539802015, 60.54930799450051637 ) ) ;
#3702 = ORIENTED_EDGE ( 'NONE', *, *, #29908, .T. ) ;
#3703 = DIRECTION ( 'NONE',  ( 0.000000000000000000, 0.000000000000000000, -1.000000000000000000 ) ) ;
#3704 = ADVANCED_FACE ( 'NONE', ( #15619 ), #3652, .T. ) ;
#3705 = AXIS2_PLACEMENT_3D ( 'NONE', #5534, #5694, #12772 ) ;
#3706 = FACE_OUTER_BOUND ( 'NONE', #6938, .T. ) ;
#3707 = DIRECTION ( 'NONE',  ( -1.101824276508909887E-16, 1.000000000000000000, -0.000000000000000000 ) ) ;
#3708 = DIRECTION ( 'NONE',  ( -1.000000000000000000, -1.101824276508910010E-16, 0.000000000000000000 ) ) ;
#3709 = EDGE_CURVE ( 'NONE', #5045, #14332, #24600, .T. ) ;
#3710 = ADVANCED_FACE ( 'NONE', ( #8406, #30895 ), #11037, .F. ) ;
#3711 = CARTESIAN_POINT ( 'NONE',  ( 48.18662509608405031, 25.79624452788248945, 49.18364984542562013 ) ) ;
#3712 = EDGE_CURVE ( 'NONE', #24927, #14398, #16156, .T. ) ;
#3713 = ORIENTED_EDGE ( 'NONE', *, *, #8139, .F. ) ;
#3714 = AXIS2_PLACEMENT_3D ( 'NONE', #23451, #28545, #20981 ) ;
#3715 = DIRECTION ( 'NONE',  ( -1.000000000000000000, 0.000000000000000000, 0.000000000000000000 ) ) ;
#3716 = CARTESIAN_POINT ( 'NONE',  ( 3.597855976057204419, 14.86454579224779948, 47.04930799450052348 ) ) ;
#3717 = ADVANCED_FACE ( 'NONE', ( #3471 ), #3111, .T. ) ;
#3718 = ORIENTED_EDGE ( 'NONE', *, *, #28578, .T. ) ;
#3719 = VECTOR ( 'NONE', #16013, 1000.000000000000000 ) ;
#3720 = CARTESIAN_POINT ( 'NONE',  ( 47.09785597605719687, 25.56454579224779877, 44.54930799450042400 ) ) ;
#3721 = CIRCLE ( 'NONE', #8458, 0.2999999999999999334 ) ;
#3722 = DIRECTION ( 'NONE',  ( 2.779292025043186357E-18, -1.288349127009862211E-17, 1.000000000000000000 ) ) ;
#3723 = VERTEX_POINT ( 'NONE', #694 ) ;
#3724 = ORIENTED_EDGE ( 'NONE', *, *, #23274, .F. ) ;
#3725 = CIRCLE ( 'NONE', #11093, 12.27641737965286239 ) ;
#3726 = EDGE_LOOP ( 'NONE', ( #27510, #3449 ) ) ;
#3727 = TOROIDAL_SURFACE ( 'NONE', #6353, 18.86195243859455672, 0.5000000000000000000 ) ;
#3728 = ORIENTED_EDGE ( 'NONE', *, *, #31274, .F. ) ;
#3729 = AXIS2_PLACEMENT_3D ( 'NONE', #12399, #17471, #15020 ) ;
#3730 = FACE_OUTER_BOUND ( 'NONE', #28754, .T. ) ;
#3731 = CIRCLE ( 'NONE', #12060, 31.29999999999997229 ) ;
#3732 = ORIENTED_EDGE ( 'NONE', *, *, #20264, .T. ) ;
#3733 = DIRECTION ( 'NONE',  ( 1.000000000000000000, 0.000000000000000000, 0.000000000000000000 ) ) ;
#3734 = DIRECTION ( 'NONE',  ( -1.101824276508909887E-16, 1.000000000000000000, -0.000000000000000000 ) ) ;
#3735 = DIRECTION ( 'NONE',  ( 0.000000000000000000, 0.000000000000000000, -1.000000000000000000 ) ) ;
#3736 = CARTESIAN_POINT ( 'NONE',  ( 45.81741271322955100, 29.24452976649964597, 49.02305402274571122 ) ) ;
#3737 = VERTEX_POINT ( 'NONE', #28433 ) ;
#3738 = VERTEX_POINT ( 'NONE', #21023 ) ;
#3739 = DIRECTION ( 'NONE',  ( 0.4848096202463430537, 0.8746197071393926326, -1.125439520643636483E-16 ) ) ;
#3740 = VECTOR ( 'NONE', #4058, 1000.000000000000000 ) ;
#3741 = ORIENTED_EDGE ( 'NONE', *, *, #18376, .T. ) ;
#3742 = CARTESIAN_POINT ( 'NONE',  ( -41.01929587258828036, 9.401204285752060130, 34.64930799450051779 ) ) ;
#3743 = CARTESIAN_POINT ( 'NONE',  ( -40.57119026524328831, 6.941393190194602880, 39.15667507985590845 ) ) ;
#3744 = LINE ( 'NONE', #23763, #27015 ) ;
#3745 = LINE ( 'NONE', #11304, #27933 ) ;
#3746 = EDGE_CURVE ( 'NONE', #21198, #15433, #6100, .T. ) ;
#3747 = ADVANCED_FACE ( 'NONE', ( #365 ), #12829, .T. ) ;
#3748 = CARTESIAN_POINT ( 'NONE',  ( -3.661041915257567947, 10.95084857405595713, -4.515295244921526674 ) ) ;
#3749 = DIRECTION ( 'NONE',  ( -1.101824276508909887E-16, 1.000000000000000000, -0.000000000000000000 ) ) ;
#3750 = ADVANCED_FACE ( 'NONE', ( #11839 ), #8723, .T. ) ;
#3751 = ORIENTED_EDGE ( 'NONE', *, *, #11564, .T. ) ;
#3752 = DIRECTION ( 'NONE',  ( -1.101824276508909887E-16, 1.000000000000000000, -0.000000000000000000 ) ) ;
#3753 = DIRECTION ( 'NONE',  ( -1.000000000000000000, 0.000000000000000000, 0.000000000000000000 ) ) ;
#3754 = DIRECTION ( 'NONE',  ( -0.2756373558169954441, 0.9612616959383198934, -1.479773560108263204E-16 ) ) ;
#3755 = VECTOR ( 'NONE', #19603, 1000.000000000000114 ) ;
#3756 = CARTESIAN_POINT ( 'NONE',  ( 47.40417757965286683, 23.10527845304106620, 46.57712699531703038 ) ) ;
#3757 = DIRECTION ( 'NONE',  ( -1.000000000000000000, 0.000000000000000000, 0.000000000000000000 ) ) ;
#3758 = EDGE_LOOP ( 'NONE', ( #26479, #12252, #8267 ) ) ;
#3759 = CARTESIAN_POINT ( 'NONE',  ( -40.02540636251513462, 2.839176264122873050, 37.04930799450052348 ) ) ;
#3760 = AXIS2_PLACEMENT_3D ( 'NONE', #7446, #17441, #24497 ) ;
#3761 = ORIENTED_EDGE ( 'NONE', *, *, #13645, .T. ) ;
#3762 = CARTESIAN_POINT ( 'NONE',  ( 48.35473289974373756, 19.96454579224779380, 45.11188864597615833 ) ) ;
#3763 = DIRECTION ( 'NONE',  ( -1.000000000000000000, 0.000000000000000000, 0.000000000000000000 ) ) ;
#3764 = VERTEX_POINT ( 'NONE', #16910 ) ;
#3765 = ORIENTED_EDGE ( 'NONE', *, *, #1816, .F. ) ;
#3766 = CARTESIAN_POINT ( 'NONE',  ( 48.28750925852675380, 22.93328494799376571, 45.80964605384927069 ) ) ;
#3767 = ADVANCED_FACE ( 'NONE', ( #26930 ), #18710, .F. ) ;
#3768 = FACE_OUTER_BOUND ( 'NONE', #18350, .T. ) ;
#3769 = CARTESIAN_POINT ( 'NONE',  ( -4.902144023942810236, 30.56554579224779644, 44.54930799450042400 ) ) ;
#3770 = ADVANCED_FACE ( 'NONE', ( #28742 ), #12580, .T. ) ;
#3771 = ORIENTED_EDGE ( 'NONE', *, *, #2724, .F. ) ;
#3772 = CARTESIAN_POINT ( 'NONE',  ( -12.94741462430176249, -13.30632128221581212, 91.42653303877501969 ) ) ;
#3773 = CIRCLE ( 'NONE', #3760, 78.39999999999999147 ) ;
#3774 = CARTESIAN_POINT ( 'NONE',  ( 21.09785597605720753, 15.23758267881771111, 47.04930799450052348 ) ) ;
#3775 = CARTESIAN_POINT ( 'NONE',  ( 74.92883917873734845, 0.05876815387845962801, 13.86745137419974050 ) ) ;
#3776 = ORIENTED_EDGE ( 'NONE', *, *, #19702, .F. ) ;
#3777 = CARTESIAN_POINT ( 'NONE',  ( 33.72499318558949000, 38.56284415653841791, 47.04930799450051637 ) ) ;
#3778 = ORIENTED_EDGE ( 'NONE', *, *, #5714, .T. ) ;
#3779 = CARTESIAN_POINT ( 'NONE',  ( -40.17244512953781310, 6.931285263614340053, 34.54930799450052348 ) ) ;
#3780 = CARTESIAN_POINT ( 'NONE',  ( 48.40423897560355471, 29.16454579224780019, 44.91779129072006072 ) ) ;
#3781 = CARTESIAN_POINT ( 'NONE',  ( -40.41647043964083252, 8.356895951721259763, 59.64930799450051779 ) ) ;
#3782 = EDGE_CURVE ( 'NONE', #14790, #23072, #11508, .T. ) ;
#3783 = FILL_AREA_STYLE ('',( #3461 ) ) ;
#3784 = ORIENTED_EDGE ( 'NONE', *, *, #31237, .F. ) ;
#3785 = ORIENTED_EDGE ( 'NONE', *, *, #9760, .F. ) ;
#3786 = DIRECTION ( 'NONE',  ( 0.8746197071393925215, -0.4848096202463429982, -8.676864087101708112E-18 ) ) ;
#3787 = DIRECTION ( 'NONE',  ( -1.000000000000000000, -1.101824276508909887E-16, 0.000000000000000000 ) ) ;
#3788 = CARTESIAN_POINT ( 'NONE',  ( 21.09992658989239089, 30.21183152705961561, 47.04930799450051637 ) ) ;
#3789 = TOROIDAL_SURFACE ( 'NONE', #16359, 0.2000000000000000111, 0.1000000000000000056 ) ;
#3790 = ORIENTED_EDGE ( 'NONE', *, *, #5673, .F. ) ;
#3791 = DIRECTION ( 'NONE',  ( -1.000000000000000000, 0.000000000000000000, 0.000000000000000000 ) ) ;
#3792 = CARTESIAN_POINT ( 'NONE',  ( 28.71925248772579664, -13.74047052604243291, -10.79927602576051093 ) ) ;
#3793 = ORIENTED_EDGE ( 'NONE', *, *, #25292, .F. ) ;
#3794 = CARTESIAN_POINT ( 'NONE',  ( -36.38930206846553261, 9.511667899829566508, 59.64930799450051779 ) ) ;
#3795 = CARTESIAN_POINT ( 'NONE',  ( 49.28428300279882990, 28.34787913140504045, 48.46772541801551171 ) ) ;
#3796 = CIRCLE ( 'NONE', #8014, 45.99866570866061011 ) ;
#3797 = DIRECTION ( 'NONE',  ( -0.000000000000000000, 1.000000000000000000, -0.000000000000000000 ) ) ;
#3798 = VECTOR ( 'NONE', #11155, 1000.000000000000000 ) ;
#3799 = EDGE_CURVE ( 'NONE', #26085, #8602, #29337, .T. ) ;
#3800 = ADVANCED_FACE ( 'NONE', ( #1820 ), #8372, .F. ) ;
#3801 = ORIENTED_EDGE ( 'NONE', *, *, #29455, .F. ) ;
#3802 = CARTESIAN_POINT ( 'NONE',  ( 21.09785597605719332, 38.31023907818019580, 47.04930799450051637 ) ) ;
#3803 = CARTESIAN_POINT ( 'NONE',  ( 21.09992658989239089, 30.09143805560860585, 47.04930799450051637 ) ) ;
#3804 = EDGE_CURVE ( 'NONE', #27622, #26389, #6424, .T. ) ;
#3805 = DIRECTION ( 'NONE',  ( 1.000000000000000000, 0.000000000000000000, 0.000000000000000000 ) ) ;
#3806 = CARTESIAN_POINT ( 'NONE',  ( 45.24946171279598417, 29.20784706826092503, 47.99220971130007030 ) ) ;
#3807 = EDGE_CURVE ( 'NONE', #22296, #20658, #11678, .T. ) ;
#3808 = ORIENTED_EDGE ( 'NONE', *, *, #30736, .F. ) ;
#3809 = ADVANCED_FACE ( 'NONE', ( #18879 ), #11193, .T. ) ;
#3810 = AXIS2_PLACEMENT_3D ( 'NONE', #3091, #13131, #645 ) ;
#3811 = CARTESIAN_POINT ( 'NONE',  ( 21.09785597605719332, 30.36454579224777461, 15.54930799450051460 ) ) ;
#3813 = CARTESIAN_POINT ( 'NONE',  ( 21.09785597605721108, -16.73545420775220194, 125.5493079945005093 ) ) ;
#3812 = AXIS2_PLACEMENT_3D ( 'NONE', #26913, #19184, #28897 ) ;
#3814 = SPHERICAL_SURFACE ( 'NONE', #25683, 0.1000000000000000056 ) ;
#3815 = EDGE_LOOP ( 'NONE', ( #26910, #21990, #8716, #2870 ) ) ;
#3816 = LINE ( 'NONE', #12019, #20735 ) ;
#3817 = CARTESIAN_POINT ( 'NONE',  ( -40.58856461370174173, 7.499380836222961477, 53.94930799450051495 ) ) ;
#3818 = CARTESIAN_POINT ( 'NONE',  ( 48.74520800137798204, 20.53597436367637030, 47.13486347384411346 ) ) ;
#3819 = VECTOR ( 'NONE', #6668, 1000.000000000000114 ) ;
#3820 = CIRCLE ( 'NONE', #21121, 2.500000000000002220 ) ;
#3821 = DIRECTION ( 'NONE',  ( -0.000000000000000000, -0.000000000000000000, -1.000000000000000000 ) ) ;
#3822 = EDGE_CURVE ( 'NONE', #18054, #23177, #20677, .T. ) ;
#3823 =( NAMED_UNIT ( * ) PLANE_ANGLE_UNIT ( ) SI_UNIT ( $, .RADIAN. ) );
#3824 = VERTEX_POINT ( 'NONE', #7070 ) ;
#3825 = CARTESIAN_POINT ( 'NONE',  ( 46.59785597605721108, 14.86454579224779948, 47.04930799450052348 ) ) ;
#3826 = CARTESIAN_POINT ( 'NONE',  ( 47.20547626766764893, 26.08791119454915730, 44.97710074790751378 ) ) ;
#3827 = FACE_OUTER_BOUND ( 'NONE', #4604, .T. ) ;
#3828 = CARTESIAN_POINT ( 'NONE',  ( 8.823575513742486720, 34.59164230456639899, 47.37072134000479906 ) ) ;
#3829 = DIRECTION ( 'NONE',  ( -1.101824276508909887E-16, 1.000000000000000000, -0.000000000000000000 ) ) ;
#3830 = EDGE_LOOP ( 'NONE', ( #3332, #16596, #29855, #32387, #24060, #13101 ) ) ;
#3831 = DIRECTION ( 'NONE',  ( -1.000000000000000000, 0.000000000000000000, 0.000000000000000000 ) ) ;
#3832 = CARTESIAN_POINT ( 'NONE',  ( -40.38516919650994197, 8.640923867788874446, 34.64930799450051779 ) ) ;
#3833 = CARTESIAN_POINT ( 'NONE',  ( 48.35473289974373756, 22.80400562401889530, 45.11188864597615833 ) ) ;
#3834 = ORIENTED_EDGE ( 'NONE', *, *, #14912, .T. ) ;
#3835 = CARTESIAN_POINT ( 'NONE',  ( 21.09992658989239089, 24.59164230456639544, 47.04930799450051637 ) ) ;
#3836 = FACE_OUTER_BOUND ( 'NONE', #5344, .T. ) ;
#3837 = DIRECTION ( 'NONE',  ( -0.8746197071393790878, 0.4848096202463673676, 1.277302113040196197E-17 ) ) ;
#3838 = DIRECTION ( 'NONE',  ( -1.000000000000000000, 0.000000000000000000, 0.000000000000000000 ) ) ;
#3839 = AXIS2_PLACEMENT_3D ( 'NONE', #30325, #2904, #12934 ) ;
#3840 = VERTEX_POINT ( 'NONE', #2149 ) ;
#3841 = CARTESIAN_POINT ( 'NONE',  ( 47.96808403254358666, 29.45344092395630753, 49.08756527095943056 ) ) ;
#3842 = VERTEX_POINT ( 'NONE', #22161 ) ;
#3843 = CIRCLE ( 'NONE', #1735, 55.62393233686778160 ) ;
#3844 = ADVANCED_FACE ( 'NONE', ( #32351 ), #2314, .T. ) ;
#3845 = B_SPLINE_CURVE_WITH_KNOTS ( 'NONE', 3,
 ( #10261, #30274, #22876, #23032, #30118, #17626, #18109, #27642 ),
 .UNSPECIFIED., .F., .F.,
 ( 4, 2, 2, 4 ),
 ( 4.856180139528653963E-16, 0.0004427811193179412167, 0.0008855622386353968192, 0.001771124477270308133 ),
 .UNSPECIFIED. ) ;
#3846 = EDGE_CURVE ( 'NONE', #10801, #17800, #22516, .T. ) ;
#3847 = ORIENTED_EDGE ( 'NONE', *, *, #6040, .F. ) ;
#3848 = AXIS2_PLACEMENT_3D ( 'NONE', #29111, #24333, #22031 ) ;
#3849 = TOROIDAL_SURFACE ( 'NONE', #2799, 12.40141737965280733, 0.1250000000000013878 ) ;
#3850 = CIRCLE ( 'NONE', #22186, 12.27641737965281621 ) ;
#3851 = EDGE_CURVE ( 'NONE', #9420, #893, #4775, .T. ) ;
#3852 = EDGE_CURVE ( 'NONE', #7282, #1140, #1061, .T. ) ;
#3853 = DIRECTION ( 'NONE',  ( 0.8746197071393926326, -0.4848096202463430537, -8.676864087101709653E-18 ) ) ;
#3854 = CARTESIAN_POINT ( 'NONE',  ( -36.69065127708124407, -5.900665263871069932, 78.38950784583703069 ) ) ;
#3855 = DIRECTION ( 'NONE',  ( -1.101824276508909887E-16, 1.000000000000000000, -0.000000000000000000 ) ) ;
#3856 = AXIS2_PLACEMENT_3D ( 'NONE', #13829, #19048, #21514 ) ;
#3857 = EDGE_LOOP ( 'NONE', ( #5635, #21578, #18371, #28721 ) ) ;
#3858 = DIRECTION ( 'NONE',  ( 0.8746197071393926326, -0.4848096202463430537, -8.676864087101709653E-18 ) ) ;
#3859 = ORIENTED_EDGE ( 'NONE', *, *, #4413, .F. ) ;
#3860 = AXIS2_PLACEMENT_3D ( 'NONE', #25966, #13511, #18572 ) ;
#3861 = DIRECTION ( 'NONE',  ( -1.000000000000000000, 0.000000000000000000, 0.000000000000000000 ) ) ;
#3862 = CARTESIAN_POINT ( 'NONE',  ( -40.54828680531408480, 6.846271790121642553, 34.54930799450052348 ) ) ;
#3863 = DIRECTION ( 'NONE',  ( -1.101824276508909887E-16, 1.000000000000000000, -0.000000000000000000 ) ) ;
#3864 = VERTEX_POINT ( 'NONE', #22325 ) ;
#3865 = CARTESIAN_POINT ( 'NONE',  ( 8.732853799281738105, 28.46183152705961206, 47.04930799450051637 ) ) ;
#3866 = CARTESIAN_POINT ( 'NONE',  ( 8.732853799281732776, 29.47145308207317527, 47.04930799450051637 ) ) ;
#3867 = CARTESIAN_POINT ( 'NONE',  ( 21.09992658989239089, 24.96183152705960140, 47.04930799450051637 ) ) ;
#3868 = DIRECTION ( 'NONE',  ( -0.9612616959383198934, -0.2756373558169956106, 0.000000000000000000 ) ) ;
#3869 = ORIENTED_EDGE ( 'NONE', *, *, #21978, .F. ) ;
#3870 = DIRECTION ( 'NONE',  ( 0.000000000000000000, 1.000000000000000000, 0.000000000000000000 ) ) ;
#3871 = DIRECTION ( 'NONE',  ( 0.000000000000000000, 0.000000000000000000, 1.000000000000000000 ) ) ;
#3872 = DIRECTION ( 'NONE',  ( 8.659560562354931626E-17, 0.7071067811865474617, -0.7071067811865475727 ) ) ;
#3873 = CIRCLE ( 'NONE', #22212, 1.899999999999999023 ) ;
#3874 = CARTESIAN_POINT ( 'NONE',  ( -42.36334586133935431, 13.70277685985800709, 54.62588685591540383 ) ) ;
#3875 = ORIENTED_EDGE ( 'NONE', *, *, #28499, .T. ) ;
#3876 = CARTESIAN_POINT ( 'NONE',  ( -40.02353495526242710, 6.996741961792352527, 34.54930799450051637 ) ) ;
#3877 = CARTESIAN_POINT ( 'NONE',  ( -40.56083369918835047, 7.405617721157512712, 35.30738027510436439 ) ) ;
#3878 = ORIENTED_EDGE ( 'NONE', *, *, #18336, .F. ) ;
#3879 = FACE_OUTER_BOUND ( 'NONE', #2224, .T. ) ;
#3880 = FACE_OUTER_BOUND ( 'NONE', #26735, .T. ) ;
#3881 = ORIENTED_EDGE ( 'NONE', *, *, #14421, .F. ) ;
#3882 = EDGE_LOOP ( 'NONE', ( #19031, #25314, #19077, #25480 ) ) ;
#3883 = UNCERTAINTY_MEASURE_WITH_UNIT (LENGTH_MEASURE( 1.000000000000000082E-05 ), #21486, 'distance_accuracy_value', 'NONE');
#3884 = ORIENTED_EDGE ( 'NONE', *, *, #24193, .F. ) ;
#3885 = CIRCLE ( 'NONE', #22223, 0.09999999999999774347 ) ;
#3886 = AXIS2_PLACEMENT_3D ( 'NONE', #17092, #9880, #4626 ) ;
#3887 = EDGE_CURVE ( 'NONE', #13889, #32220, #14468, .T. ) ;
#3888 = AXIS2_PLACEMENT_3D ( 'NONE', #4950, #30225, #27593 ) ;
#3889 = EDGE_CURVE ( 'NONE', #6416, #13529, #21989, .T. ) ;
#3890 = ORIENTED_EDGE ( 'NONE', *, *, #848, .F. ) ;
#3891 = CARTESIAN_POINT ( 'NONE',  ( 21.09785597605720042, 16.86454579224779948, 95.68336035963606889 ) ) ;
#3892 = VERTEX_POINT ( 'NONE', #21841 ) ;
#3893 = DIRECTION ( 'NONE',  ( 0.000000000000000000, 1.517883041479704827E-15, -1.000000000000000000 ) ) ;
#3894 = CARTESIAN_POINT ( 'NONE',  ( 46.95686452149019630, 22.86454579224779948, 49.04468102550210773 ) ) ;
#3895 = DIRECTION ( 'NONE',  ( 0.9612616959383206705, 0.2756373558169927240, 2.454997878969170293E-14 ) ) ;
#3896 = DIRECTION ( 'NONE',  ( 0.1949050434465267878, -0.6797146636928667052, 0.7071067811865480168 ) ) ;
#3897 = CARTESIAN_POINT ( 'NONE',  ( 48.91284552371730143, 28.83619643316631453, 46.12344667017377020 ) ) ;
#3898 = ORIENTED_EDGE ( 'NONE', *, *, #19488, .T. ) ;
#3899 = ORIENTED_EDGE ( 'NONE', *, *, #18068, .T. ) ;
#3900 = CARTESIAN_POINT ( 'NONE',  ( -12.13387836560771582, -4.491775094913932342, -8.765527212216683850 ) ) ;
#3901 = ORIENTED_EDGE ( 'NONE', *, *, #30886, .F. ) ;
#3902 = DIRECTION ( 'NONE',  ( 1.000000000000000000, 0.000000000000000000, 0.000000000000000000 ) ) ;
#3903 = CARTESIAN_POINT ( 'NONE',  ( -40.59758774925372649, 7.567737757495682338, 38.66054537865625917 ) ) ;
#3904 = DIRECTION ( 'NONE',  ( -1.224646799147353207E-16, 0.000000000000000000, -1.000000000000000000 ) ) ;
#3905 = DIRECTION ( 'NONE',  ( 0.000000000000000000, -0.000000000000000000, -1.000000000000000000 ) ) ;
#3906 = CARTESIAN_POINT ( 'NONE',  ( 48.73570333863616355, 25.72287913140504756, 44.52463952959527660 ) ) ;
#3907 = AXIS2_PLACEMENT_3D ( 'NONE', #833, #30875, #17909 ) ;
#3908 = AXIS2_PLACEMENT_3D ( 'NONE', #22141, #29549, #21655 ) ;
#3909 = FACE_OUTER_BOUND ( 'NONE', #20286, .T. ) ;
#3910 = DIRECTION ( 'NONE',  ( 0.8746197071393926326, -0.4848096202463430537, -8.676864087101709653E-18 ) ) ;
#3911 = AXIS2_PLACEMENT_3D ( 'NONE', #5524, #10130, #25056 ) ;
#3912 = VERTEX_POINT ( 'NONE', #10981 ) ;
#3913 = CARTESIAN_POINT ( 'NONE',  ( 21.09785597605719332, 44.06454579224779877, 47.04930799450051637 ) ) ;
#3914 = FACE_BOUND ( 'NONE', #701, .T. ) ;
#3915 = CIRCLE ( 'NONE', #26990, 78.50000000000000000 ) ;
#3916 = DIRECTION ( 'NONE',  ( 0.9612616959383205595, 0.2756373558169932236, -1.660411357259282445E-16 ) ) ;
#3917 = AXIS2_PLACEMENT_3D ( 'NONE', #15584, #10691, #25602 ) ;
#3918 = AXIS2_PLACEMENT_3D ( 'NONE', #26048, #3075, #30672 ) ;
#3919 = CARTESIAN_POINT ( 'NONE',  ( 21.09785597605719332, 30.36454579224779238, 34.04930799450050927 ) ) ;
#3920 = CARTESIAN_POINT ( 'NONE',  ( 47.22751897799751220, 25.71988759933319102, 44.55267275764142454 ) ) ;
#3921 = ORIENTED_EDGE ( 'NONE', *, *, #5538, .T. ) ;
#3922 = DIRECTION ( 'NONE',  ( -0.000000000000000000, -1.000000000000000000, -0.000000000000000000 ) ) ;
#3923 = ORIENTED_EDGE ( 'NONE', *, *, #32133, .F. ) ;
#3924 = CARTESIAN_POINT ( 'NONE',  ( 21.09785597605720753, 13.86454579224779948, 47.04930799450052348 ) ) ;
#3925 = FACE_OUTER_BOUND ( 'NONE', #31699, .T. ) ;
#3926 = ORIENTED_EDGE ( 'NONE', *, *, #17786, .F. ) ;
#3927 = B_SPLINE_CURVE_WITH_KNOTS ( 'NONE', 3,
 ( #26709, #31650, #16531, #11621 ),
 .UNSPECIFIED., .F., .F.,
 ( 4, 4 ),
 ( 0.07242793514135081878, 0.08828840816840291539 ),
 .UNSPECIFIED. ) ;
#3928 = EDGE_CURVE ( 'NONE', #10149, #6712, #14396, .T. ) ;
#3929 = ADVANCED_FACE ( 'NONE', ( #15570 ), #17880, .T. ) ;
#3930 = AXIS2_PLACEMENT_3D ( 'NONE', #12303, #17542, #27561 ) ;
#3931 = EDGE_CURVE ( 'NONE', #4981, #14884, #8218, .T. ) ;
#3932 = ORIENTED_EDGE ( 'NONE', *, *, #25696, .F. ) ;
#3933 = EDGE_CURVE ( 'NONE', #17034, #31739, #10335, .T. ) ;
#3934 = CIRCLE ( 'NONE', #21203, 0.09999999999999795164 ) ;
#3935 = EDGE_CURVE ( 'NONE', #27622, #30194, #9457, .T. ) ;
#3936 = DIRECTION ( 'NONE',  ( -1.101824276508909887E-16, 1.000000000000000000, -0.000000000000000000 ) ) ;
#3937 = CARTESIAN_POINT ( 'NONE',  ( -12.40214402394279603, 14.86454579224779948, 47.04930799450052348 ) ) ;
#3939 = CYLINDRICAL_SURFACE ( 'NONE', #6830, 12.62506659569710266 ) ;
#3938 = CIRCLE ( 'NONE', #14960, 12.27641737965287305 ) ;
#3940 = CIRCLE ( 'NONE', #16002, 12.36707279061065101 ) ;
#3941 = CIRCLE ( 'NONE', #18095, 46.27992121592387065 ) ;
#3942 = ORIENTED_EDGE ( 'NONE', *, *, #14008, .F. ) ;
#3943 = CARTESIAN_POINT ( 'NONE',  ( -34.71499704722533153, -13.30632128221581034, 50.70225068270534052 ) ) ;
#3944 = DIRECTION ( 'NONE',  ( -0.000000000000000000, -1.000000000000000000, -0.000000000000000000 ) ) ;
#3945 = CARTESIAN_POINT ( 'NONE',  ( 77.48905355674300210, -4.114116020023757869, 13.63154984733677644 ) ) ;
#3946 = EDGE_LOOP ( 'NONE', ( #32120, #21776, #17000, #11287 ) ) ;
#3947 = DIRECTION ( 'NONE',  ( -1.101824276508909887E-16, 1.000000000000000000, -0.000000000000000000 ) ) ;
#3948 = ORIENTED_EDGE ( 'NONE', *, *, #29480, .F. ) ;
#3949 = CARTESIAN_POINT ( 'NONE',  ( 49.54111243405073139, 29.13489273995354267, 47.87666846268844267 ) ) ;
#3950 = DIRECTION ( 'NONE',  ( 1.000000000000000000, 0.000000000000000000, 0.000000000000000000 ) ) ;
#3951 = ORIENTED_EDGE ( 'NONE', *, *, #31908, .F. ) ;
#3952 = VERTEX_POINT ( 'NONE', #10829 ) ;
#3953 = CARTESIAN_POINT ( 'NONE',  ( 75.12562691325332764, -13.30632128221581212, 32.57800810680159032 ) ) ;
#3954 = DIRECTION ( 'NONE',  ( -1.000000000000000000, 0.000000000000000000, 0.000000000000000000 ) ) ;
#3955 = CARTESIAN_POINT ( 'NONE',  ( 21.09992658989239089, 24.34164230456639544, 47.04930799450051637 ) ) ;
#3956 = VECTOR ( 'NONE', #9637, 1000.000000000000114 ) ;
#3957 = ORIENTED_EDGE ( 'NONE', *, *, #19251, .F. ) ;
#3958 = CARTESIAN_POINT ( 'NONE',  ( 48.96852009960340268, 19.86454579224779948, 46.09504611384270589 ) ) ;
#3959 = CARTESIAN_POINT ( 'NONE',  ( 67.39212317433589305, -13.74047052604243824, 11.53332310724655230 ) ) ;
#3960 = ORIENTED_EDGE ( 'NONE', *, *, #23675, .T. ) ;
#3961 = CARTESIAN_POINT ( 'NONE',  ( -40.50726676055796105, 7.559560307024983494, 60.27956441091988182 ) ) ;
#3962 = CARTESIAN_POINT ( 'NONE',  ( 44.09250526802607340, 27.35621246473837331, 46.89322480343881949 ) ) ;
#3963 = EDGE_CURVE ( 'NONE', #4744, #17141, #18339, .T. ) ;
#3964 = VECTOR ( 'NONE', #7440, 1000.000000000000000 ) ;
#3965 = EDGE_CURVE ( 'NONE', #14754, #4855, #5249, .T. ) ;
#3966 = CARTESIAN_POINT ( 'NONE',  ( 21.09992658989238734, 38.56284415653841791, 47.04930799450051637 ) ) ;
#3967 = CIRCLE ( 'NONE', #1335, 0.1250000000000001110 ) ;
#3968 = VERTEX_POINT ( 'NONE', #8353 ) ;
#3969 = CARTESIAN_POINT ( 'NONE',  ( 21.09992658989239089, 24.47145308207319303, 47.04930799450051637 ) ) ;
#3970 = ADVANCED_FACE ( 'NONE', ( #13297 ), #30429, .T. ) ;
#3971 = DIRECTION ( 'NONE',  ( -0.7848668881104262640, -0.2250569586005336520, -0.5773502691896258421 ) ) ;
#3972 = DIRECTION ( 'NONE',  ( -1.000000000000000000, 0.000000000000000000, 0.000000000000000000 ) ) ;
#3973 = CARTESIAN_POINT ( 'NONE',  ( 47.20547626766766314, 28.27451373492759501, 44.97710074790751378 ) ) ;
#3974 = ORIENTED_EDGE ( 'NONE', *, *, #10954, .T. ) ;
#3975 = DIRECTION ( 'NONE',  ( 0.000000000000000000, 0.000000000000000000, 1.000000000000000000 ) ) ;
#3976 = CARTESIAN_POINT ( 'NONE',  ( 33.46699938050304013, 26.71183152705960495, 47.04930799450051637 ) ) ;
#3977 = VECTOR ( 'NONE', #3786, 1000.000000000000114 ) ;
#3978 = PLANE ( 'NONE',  #24103 ) ;
#3979 = MECHANICAL_DESIGN_GEOMETRIC_PRESENTATION_REPRESENTATION (  '', ( #24430 ), #21804 ) ;
#3980 = DIRECTION ( 'NONE',  ( -1.101824276508909887E-16, 1.000000000000000000, -0.000000000000000000 ) ) ;
#3981 = CARTESIAN_POINT ( 'NONE',  ( 8.732853799281734553, 38.56284415653841791, 47.04930799450051637 ) ) ;
#3982 = EDGE_CURVE ( 'NONE', #13490, #18781, #6829, .T. ) ;
#3983 = CARTESIAN_POINT ( 'NONE',  ( 21.09785597605719332, 44.06454579224779877, 47.04930799450051637 ) ) ;
#3984 = VERTEX_POINT ( 'NONE', #7878 ) ;
#3985 = CARTESIAN_POINT ( 'NONE',  ( -39.58809650894544774, 2.596771453999702661, 47.04930799450051637 ) ) ;
#3986 = CARTESIAN_POINT ( 'NONE',  ( 49.49063479933183629, 25.91291119454916014, 47.17357720316391578 ) ) ;
#3987 = FACE_OUTER_BOUND ( 'NONE', #11241, .T. ) ;
#3988 = EDGE_CURVE ( 'NONE', #7332, #10562, #29362, .T. ) ;
#3989 = DIRECTION ( 'NONE',  ( 0.000000000000000000, 0.000000000000000000, -1.000000000000000000 ) ) ;
#3990 = CIRCLE ( 'NONE', #24964, 40.00000000000000000 ) ;
#3991 = DIRECTION ( 'NONE',  ( 0.000000000000000000, 0.000000000000000000, -1.000000000000000000 ) ) ;
#3992 = ORIENTED_EDGE ( 'NONE', *, *, #3477, .T. ) ;
#3993 = CARTESIAN_POINT ( 'NONE',  ( -39.57297000773472462, -5.936060209327997939, 77.91230730958153572 ) ) ;
#3994 = CARTESIAN_POINT ( 'NONE',  ( -40.23847960489091236, 6.935107575317838169, 39.54930799450052348 ) ) ;
#3995 = DIRECTION ( 'NONE',  ( -1.000000000000000000, 0.000000000000000000, 0.000000000000000000 ) ) ;
#3996 = EDGE_LOOP ( 'NONE', ( #6785, #27567, #29701, #28632 ) ) ;
#3997 = DIRECTION ( 'NONE',  ( -1.000000000000000000, 0.000000000000000000, 0.000000000000000000 ) ) ;
#3998 = DIRECTION ( 'NONE',  ( 1.202146588165213953E-16, -0.1908089953765421121, 0.9816271834476645308 ) ) ;
#3999 = EDGE_CURVE ( 'NONE', #9462, #25082, #8400, .T. ) ;
#4000 = EDGE_CURVE ( 'NONE', #23526, #19268, #475, .T. ) ;
#4001 = DIRECTION ( 'NONE',  ( 0.000000000000000000, -1.000000000000000000, 0.000000000000000000 ) ) ;
#4002 = CARTESIAN_POINT ( 'NONE',  ( 21.09785597605720753, 13.86454579224779948, 47.04930799450052348 ) ) ;
#4003 = EDGE_LOOP ( 'NONE', ( #6018, #29108, #2802, #29688 ) ) ;
#4004 = CARTESIAN_POINT ( 'NONE',  ( -40.60330327974818232, 7.565477138576673255, 60.21714911875709220 ) ) ;
#4005 = ORIENTED_EDGE ( 'NONE', *, *, #24067, .F. ) ;
#4006 = AXIS2_PLACEMENT_3D ( 'NONE', #5579, #20826, #5740 ) ;
#4007 = APPLICATION_PROTOCOL_DEFINITION ( 'draft international standard', 'automotive_design', 1998, #17040 ) ;
#4008 = ORIENTED_EDGE ( 'NONE', *, *, #32492, .T. ) ;
#4009 = EDGE_CURVE ( 'NONE', #11017, #22098, #7346, .T. ) ;
#4010 = CONICAL_SURFACE ( 'NONE', #1922, 55.00000000000000000, 0.7853981633974552734 ) ;
#4011 = CARTESIAN_POINT ( 'NONE',  ( 21.09785597605719332, 24.86454579224779948, 21.04930799450051282 ) ) ;
#4012 = DIRECTION ( 'NONE',  ( -1.000000000000000000, 0.000000000000000000, 0.000000000000000000 ) ) ;
#4013 = CARTESIAN_POINT ( 'NONE',  ( 47.09785597605719687, 30.56554579224779644, 49.54930799450078638 ) ) ;
#4014 = ORIENTED_EDGE ( 'NONE', *, *, #20879, .T. ) ;
#4015 = DIRECTION ( 'NONE',  ( -0.000000000000000000, -1.000000000000000000, 0.000000000000000000 ) ) ;
#4016 = ORIENTED_EDGE ( 'NONE', *, *, #3073, .T. ) ;
#4017 = FACE_OUTER_BOUND ( 'NONE', #22898, .T. ) ;
#4018 = EDGE_CURVE ( 'NONE', #2537, #17110, #20459, .T. ) ;
#4019 = SURFACE_STYLE_FILL_AREA ( #11407 ) ;
#4020 = EDGE_LOOP ( 'NONE', ( #12850, #30333, #22793, #3771 ) ) ;
#4021 = DIRECTION ( 'NONE',  ( -1.000000000000000000, 0.000000000000000000, 0.000000000000000000 ) ) ;
#4022 = DIRECTION ( 'NONE',  ( -1.101824276508909887E-16, 1.000000000000000000, -0.000000000000000000 ) ) ;
#4023 = DIRECTION ( 'NONE',  ( -1.101824276508909887E-16, 1.000000000000000000, -0.000000000000000000 ) ) ;
#4025 = DIRECTION ( 'NONE',  ( -1.000000000000000000, 0.000000000000000000, 0.000000000000000000 ) ) ;
#4024 = AXIS2_PLACEMENT_3D ( 'NONE', #24331, #19573, #11545 ) ;
#4026 = ORIENTED_EDGE ( 'NONE', *, *, #14312, .F. ) ;
#4027 = CARTESIAN_POINT ( 'NONE',  ( 47.17436303681730436, 22.98765316579147466, 45.57618128815960290 ) ) ;
#4028 = EDGE_CURVE ( 'NONE', #9505, #19596, #19390, .T. ) ;
#4029 = DIRECTION ( 'NONE',  ( 0.000000000000000000, 0.000000000000000000, 1.000000000000000000 ) ) ;
#4030 = CARTESIAN_POINT ( 'NONE',  ( -40.69193635511749108, 9.347952559758585522, 39.54930799450052348 ) ) ;
#4031 = CARTESIAN_POINT ( 'NONE',  ( 33.50134396954525329, 26.34164230456639899, 47.04930799450051637 ) ) ;
#4032 = DIRECTION ( 'NONE',  ( 0.000000000000000000, 0.000000000000000000, -1.000000000000000000 ) ) ;
#4033 = ORIENTED_EDGE ( 'NONE', *, *, #11886, .T. ) ;
#4034 = CARTESIAN_POINT ( 'NONE',  ( 21.09992658989239089, 24.09164230456639544, 47.04930799450051637 ) ) ;
#4035 = CARTESIAN_POINT ( 'NONE',  ( -30.89605511857140741, 11.92558985988973497, 26.63511333407100423 ) ) ;
#4036 = EDGE_LOOP ( 'NONE', ( #5706, #21425, #18800, #10206 ) ) ;
#4037 = DIRECTION ( 'NONE',  ( 0.4544104193609903586, 0.000000000000000000, 0.8907924397839087627 ) ) ;
#4038 = EDGE_CURVE ( 'NONE', #18056, #7765, #31988, .T. ) ;
#4039 = FACE_OUTER_BOUND ( 'NONE', #9124, .T. ) ;
#4040 = ADVANCED_FACE ( 'NONE', ( #23762 ), #16258, .T. ) ;
#4041 = ORIENTED_EDGE ( 'NONE', *, *, #9572, .F. ) ;
#4042 = ORIENTED_EDGE ( 'NONE', *, *, #1385, .F. ) ;
#4043 = ORIENTED_EDGE ( 'NONE', *, *, #23890, .F. ) ;
#4044 = AXIS2_PLACEMENT_3D ( 'NONE', #26598, #8880, #6741 ) ;
#4045 = CIRCLE ( 'NONE', #1419, 1.999999999999998224 ) ;
#4046 = CARTESIAN_POINT ( 'NONE',  ( -40.91899271407989858, 10.13979218557001616, 37.04930799450052348 ) ) ;
#4047 = ORIENTED_EDGE ( 'NONE', *, *, #20264, .F. ) ;
#4048 = PLANE ( 'NONE',  #18437 ) ;
#4049 = CARTESIAN_POINT ( 'NONE',  ( 21.09992658989238734, 38.56284415653841791, 47.04930799450051637 ) ) ;
#4050 = DIRECTION ( 'NONE',  ( 0.000000000000000000, 1.000000000000000000, -0.000000000000000000 ) ) ;
#4051 = DIRECTION ( 'NONE',  ( -0.9612616959383194493, -0.2756373558169974980, -8.795445018804946186E-19 ) ) ;
#4052 = ADVANCED_FACE ( 'NONE', ( #14253 ), #21292, .T. ) ;
#4053 = CARTESIAN_POINT ( 'NONE',  ( 48.16694854572211426, 27.26119643316631880, 49.14507740233662503 ) ) ;
#4054 = EDGE_LOOP ( 'NONE', ( #31986, #7662, #22931, #16979 ) ) ;
#4055 = ORIENTED_EDGE ( 'NONE', *, *, #10445, .T. ) ;
#4056 = DIRECTION ( 'NONE',  ( -1.101824276508909887E-16, 1.000000000000000000, -0.000000000000000000 ) ) ;
#4057 = ORIENTED_EDGE ( 'NONE', *, *, #16753, .F. ) ;
#4058 = DIRECTION ( 'NONE',  ( 0.000000000000000000, -0.7071067811865426878, -0.7071067811865524577 ) ) ;
#4059 = DIRECTION ( 'NONE',  ( 0.000000000000000000, 0.000000000000000000, -1.000000000000000000 ) ) ;
#4060 = DIRECTION ( 'NONE',  ( -2.779292025043186357E-18, 1.288349127009862211E-17, -1.000000000000000000 ) ) ;
#4061 = CARTESIAN_POINT ( 'NONE',  ( 21.09785597605720753, -5.098646251524523443, 47.04930799450052348 ) ) ;
#4062 = CARTESIAN_POINT ( 'NONE',  ( 99.49785597605720966, -16.63545420775220052, 47.04930799450051637 ) ) ;
#4063 = CARTESIAN_POINT ( 'NONE',  ( 50.10320668408830613, 24.90621246473838468, 47.20539118556276037 ) ) ;
#4064 = CARTESIAN_POINT ( 'NONE',  ( 46.59799852009219734, 22.98879437201065912, 48.43017694493634195 ) ) ;
#4065 = CARTESIAN_POINT ( 'NONE',  ( 106.0978559760576019, 9.702389020015065313, 20.34850893876566857 ) ) ;
#4066 = ORIENTED_EDGE ( 'NONE', *, *, #26002, .F. ) ;
#4067 = CARTESIAN_POINT ( 'NONE',  ( -63.90214402394282445, -3.935454207752200340, 54.04930799450051637 ) ) ;
#4068 = CARTESIAN_POINT ( 'NONE',  ( -43.64647580959332629, 1.256990871545142330, 60.44930799450051495 ) ) ;
#4069 = AXIS2_PLACEMENT_3D ( 'NONE', #11640, #31502, #6552 ) ;
#4070 = CARTESIAN_POINT ( 'NONE',  ( -40.11286833322908052, 2.887657226147511302, 57.04930799450051637 ) ) ;
#4071 = AXIS2_PLACEMENT_3D ( 'NONE', #21137, #25916, #31175 ) ;
#4072 = ADVANCED_FACE ( 'NONE', ( #16370 ), #1569, .T. ) ;
#4073 = DIRECTION ( 'NONE',  ( 1.177206059073821606E-16, -0.2756373558169902815, 0.9612616959383214477 ) ) ;
#4074 = DIRECTION ( 'NONE',  ( -1.101824276508909887E-16, 1.000000000000000000, -0.000000000000000000 ) ) ;
#4075 = ORIENTED_EDGE ( 'NONE', *, *, #9216, .F. ) ;
#4076 = LINE ( 'NONE', #16873, #9868 ) ;
#4077 = AXIS2_PLACEMENT_3D ( 'NONE', #6217, #16219, #3753 ) ;
#4078 = ORIENTED_EDGE ( 'NONE', *, *, #1662, .F. ) ;
#4079 = FACE_OUTER_BOUND ( 'NONE', #31918, .T. ) ;
#4080 = CARTESIAN_POINT ( 'NONE',  ( 9.016997203727582288, 34.59164230456639899, 47.36565641480107303 ) ) ;
#4081 = CIRCLE ( 'NONE', #25568, 2.500000000000002220 ) ;
#4082 = ORIENTED_EDGE ( 'NONE', *, *, #11049, .F. ) ;
#4083 = ORIENTED_EDGE ( 'NONE', *, *, #20853, .T. ) ;
#4084 = LINE ( 'NONE', #31347, #263 ) ;
#4085 = CIRCLE ( 'NONE', #27700, 12.62506659569710266 ) ;
#4086 = CARTESIAN_POINT ( 'NONE',  ( 52.59785597605720397, -5.098646251524523443, 47.04930799450051637 ) ) ;
#4087 = CARTESIAN_POINT ( 'NONE',  ( -40.61685141166179136, 7.997713659873190828, 39.96793714460204683 ) ) ;
#4088 = CIRCLE ( 'NONE', #24519, 0.9999999999999940048 ) ;
#4089 = ORIENTED_EDGE ( 'NONE', *, *, #10087, .F. ) ;
#4090 = AXIS2_PLACEMENT_3D ( 'NONE', #29104, #1194, #5979 ) ;
#4091 = LINE ( 'NONE', #9351, #15643 ) ;
#4092 = CIRCLE ( 'NONE', #13044, 12.36707279061065101 ) ;
#4093 = CARTESIAN_POINT ( 'NONE',  ( 78.85204100697130514, -5.379633064793138963, 14.58826358935728607 ) ) ;
#4094 = ORIENTED_EDGE ( 'NONE', *, *, #14875, .F. ) ;
#4095 = PRESENTATION_STYLE_ASSIGNMENT (( #2293 ) ) ;
#4096 = ORIENTED_EDGE ( 'NONE', *, *, #5611, .F. ) ;
#4097 = AXIS2_PLACEMENT_3D ( 'NONE', #11526, #21522, #29581 ) ;
#4098 = FACE_BOUND ( 'NONE', #31253, .T. ) ;
#4099 = CARTESIAN_POINT ( 'NONE',  ( 49.59034552300744281, 29.16454579224780019, 47.24294646780535345 ) ) ;
#4100 = DIRECTION ( 'NONE',  ( 0.000000000000000000, 0.000000000000000000, -1.000000000000000000 ) ) ;
#4101 = CARTESIAN_POINT ( 'NONE',  ( 0.000000000000000000, 0.000000000000000000, 0.000000000000000000 ) ) ;
#4102 = EDGE_LOOP ( 'NONE', ( #22436, #25184, #20452, #30552 ) ) ;
#4103 = ORIENTED_EDGE ( 'NONE', *, *, #30107, .T. ) ;
#4104 = DIRECTION ( 'NONE',  ( -1.101824276508909887E-16, 1.000000000000000000, -0.000000000000000000 ) ) ;
#4105 = DIRECTION ( 'NONE',  ( 0.8746197071393925215, -0.4848096202463429982, -8.676864087101708112E-18 ) ) ;
#4106 = EDGE_CURVE ( 'NONE', #29845, #14608, #27798, .T. ) ;
#4107 = EDGE_CURVE ( 'NONE', #28880, #11449, #6056, .T. ) ;
#4108 = CARTESIAN_POINT ( 'NONE',  ( -10.50890583686613233, -5.822320178462002893, 105.8904890469746221 ) ) ;
#4109 = EDGE_CURVE ( 'NONE', #14664, #32344, #24650, .T. ) ;
#4110 = EDGE_CURVE ( 'NONE', #10069, #13562, #28321, .T. ) ;
#4111 = VERTEX_POINT ( 'NONE', #26713 ) ;
#4112 = PLANE ( 'NONE',  #5628 ) ;
#4113 = CARTESIAN_POINT ( 'NONE',  ( 59.57376688280871946, -13.74047052604243646, 3.184189302845370495 ) ) ;
#4114 = ADVANCED_FACE ( 'NONE', ( #6534 ), #23065, .T. ) ;
#4115 = ORIENTED_EDGE ( 'NONE', *, *, #25644, .T. ) ;
#4116 = DIRECTION ( 'NONE',  ( 0.000000000000000000, 1.000000000000000000, -0.000000000000000000 ) ) ;
#4117 = EDGE_CURVE ( 'NONE', #18405, #4732, #25187, .T. ) ;
#4118 = DIRECTION ( 'NONE',  ( -1.224646799147353207E-16, -1.349345573449484691E-32, 1.000000000000000000 ) ) ;
#4119 = AXIS2_PLACEMENT_3D ( 'NONE', #23476, #15771, #21316 ) ;
#4120 = AXIS2_PLACEMENT_3D ( 'NONE', #11962, #17647, #12578 ) ;
#4121 = CARTESIAN_POINT ( 'NONE',  ( 21.09785597605720753, -13.59284023713420630, 102.7732403313682994 ) ) ;
#4122 = AXIS2_PLACEMENT_3D ( 'NONE', #28429, #6255, #3787 ) ;
#4123 = AXIS2_PLACEMENT_3D ( 'NONE', #22239, #9455, #21910 ) ;
#4124 = CIRCLE ( 'NONE', #7798, 3.299999999999997158 ) ;
#4125 = ORIENTED_EDGE ( 'NONE', *, *, #29280, .F. ) ;
#4126 = FACE_OUTER_BOUND ( 'NONE', #31906, .T. ) ;
#4127 = DIRECTION ( 'NONE',  ( 0.9612616959383145643, 0.2756373558170139848, 8.795445018807193747E-19 ) ) ;
#4128 = DIRECTION ( 'NONE',  ( 0.8746197071393926326, -0.4848096202463430537, -8.676864087101709653E-18 ) ) ;
#4129 = CARTESIAN_POINT ( 'NONE',  ( 46.99023568444673060, 27.92451373492759714, 49.12151524109405898 ) ) ;
#4130 = EDGE_LOOP ( 'NONE', ( #2015, #19239 ) ) ;
#4131 = DIRECTION ( 'NONE',  ( 1.234978253042719660E-16, -1.000000000000000000, -1.109335647967047851E-31 ) ) ;
#4132 = CARTESIAN_POINT ( 'NONE',  ( 21.09785597605719332, 13.06454579224779877, 47.04930799450051637 ) ) ;
#4133 = EDGE_CURVE ( 'NONE', #5692, #12300, #5781, .T. ) ;
#4134 = CARTESIAN_POINT ( 'NONE',  ( -40.18454328187963398, 7.548069831825862330, 53.64930799450051779 ) ) ;
#4135 = AXIS2_PLACEMENT_3D ( 'NONE', #7384, #2453, #12470 ) ;
#4136 = CIRCLE ( 'NONE', #31269, 12.27641737965282687 ) ;
#4137 = DIRECTION ( 'NONE',  ( -1.101824276508909887E-16, 1.000000000000000000, -0.000000000000000000 ) ) ;
#4138 = DIRECTION ( 'NONE',  ( -0.000000000000000000, -1.000000000000000000, -0.000000000000000000 ) ) ;
#4139 = LINE ( 'NONE', #27768, #25246 ) ;
#4140 = DIRECTION ( 'NONE',  ( -0.8746197071393925215, 0.4848096202463429982, 8.676864087101708112E-18 ) ) ;
#4141 = DIRECTION ( 'NONE',  ( 0.000000000000000000, 0.000000000000000000, -1.000000000000000000 ) ) ;
#4142 = FILL_AREA_STYLE ('',( #7099 ) ) ;
#4143 = ORIENTED_EDGE ( 'NONE', *, *, #2721, .T. ) ;
#4144 = CYLINDRICAL_SURFACE ( 'NONE', #10283, 12.62506659569710266 ) ;
#4145 = CARTESIAN_POINT ( 'NONE',  ( 44.26921014953015288, 25.23153309617947926, 48.49225502104211927 ) ) ;
#4146 = CARTESIAN_POINT ( 'NONE',  ( 21.09785597605719332, 25.13358275951983956, 47.04930799450051637 ) ) ;
#4147 = VECTOR ( 'NONE', #27086, 1000.000000000000000 ) ;
#4148 = DIRECTION ( 'NONE',  ( -1.000000000000000000, 0.000000000000000000, 0.000000000000000000 ) ) ;
#4149 = EDGE_CURVE ( 'NONE', #19482, #30996, #10519, .T. ) ;
#4150 = ORIENTED_EDGE ( 'NONE', *, *, #18011, .F. ) ;
#4151 = CARTESIAN_POINT ( 'NONE',  ( -39.57027300287975180, -5.936134875209708284, 77.92680640967554950 ) ) ;
#4152 = AXIS2_PLACEMENT_3D ( 'NONE', #17893, #13142, #15111 ) ;
#4153 = DIRECTION ( 'NONE',  ( -0.000000000000000000, -0.000000000000000000, -1.000000000000000000 ) ) ;
#4154 = LINE ( 'NONE', #7764, #6798 ) ;
#4155 = ORIENTED_EDGE ( 'NONE', *, *, #11166, .F. ) ;
#4156 = DIRECTION ( 'NONE',  ( -1.224646799147353207E-16, -1.349345573449484691E-32, 1.000000000000000000 ) ) ;
#4157 = EDGE_CURVE ( 'NONE', #11938, #12012, #2639, .T. ) ;
#4158 = CARTESIAN_POINT ( 'NONE',  ( 21.09992658989239089, 27.84164230456639544, 47.04930799450051637 ) ) ;
#4159 = DIRECTION ( 'NONE',  ( -1.000000000000000000, 0.000000000000000000, 0.000000000000000000 ) ) ;
#4160 = FACE_OUTER_BOUND ( 'NONE', #14723, .T. ) ;
#4161 = VERTEX_POINT ( 'NONE', #12609 ) ;
#4162 = CARTESIAN_POINT ( 'NONE',  ( 21.09785597605719332, 38.31023907818019580, 47.04930799450051637 ) ) ;
#4163 = ORIENTED_EDGE ( 'NONE', *, *, #23422, .T. ) ;
#4164 = AXIS2_PLACEMENT_3D ( 'NONE', #16848, #26699, #24072 ) ;
#4165 = VECTOR ( 'NONE', #31582, 1000.000000000000000 ) ;
#4166 = ORIENTED_EDGE ( 'NONE', *, *, #27096, .T. ) ;
#4167 = FACE_OUTER_BOUND ( 'NONE', #5039, .T. ) ;
#4168 = EDGE_CURVE ( 'NONE', #10736, #16068, #7347, .T. ) ;
#4169 = AXIS2_PLACEMENT_3D ( 'NONE', #24838, #30097, #27128 ) ;
#4170 = AXIS2_PLACEMENT_3D ( 'NONE', #1371, #11553, #9088 ) ;
#4171 = TOROIDAL_SURFACE ( 'NONE', #15200, 12.40141737965284463, 0.1250000000000005274 ) ;
#4172 = FACE_OUTER_BOUND ( 'NONE', #7776, .T. ) ;
#4173 = CARTESIAN_POINT ( 'NONE',  ( 48.05211795450447454, 25.13954579807170120, 48.91997206816282784 ) ) ;
#4174 = CARTESIAN_POINT ( 'NONE',  ( 48.23388202445966755, 29.05087065737811969, 49.27628909396056400 ) ) ;
#4175 = CIRCLE ( 'NONE', #3662, 12.62506659569710266 ) ;
#4176 = EDGE_CURVE ( 'NONE', #3842, #3511, #29596, .T. ) ;
#4177 = ADVANCED_FACE ( 'NONE', ( #19973 ), #17836, .T. ) ;
#4178 = VERTEX_POINT ( 'NONE', #31967 ) ;
#4179 = DIRECTION ( 'NONE',  ( 0.2756373558170404081, -0.9612616959383071258, 1.479773560108186044E-16 ) ) ;
#4180 = ORIENTED_EDGE ( 'NONE', *, *, #17896, .T. ) ;
#4181 = DIRECTION ( 'NONE',  ( 0.000000000000000000, 0.000000000000000000, 1.000000000000000000 ) ) ;
#4182 = ADVANCED_BREP_SHAPE_REPRESENTATION ( '', ( #1196, #8172 ), #27017 ) ;
#4183 = LINE ( 'NONE', #8632, #8426 ) ;
#4184 = DIRECTION ( 'NONE',  ( -0.000000000000000000, -1.000000000000000000, 0.000000000000000000 ) ) ;
#4185 = ORIENTED_EDGE ( 'NONE', *, *, #15938, .T. ) ;
#4186 = DIRECTION ( 'NONE',  ( 0.000000000000000000, 0.000000000000000000, 1.000000000000000000 ) ) ;
#4187 = CARTESIAN_POINT ( 'NONE',  ( 21.09992658989239089, 30.09143805560860585, 47.04930799450051637 ) ) ;
#4188 = CARTESIAN_POINT ( 'NONE',  ( 21.09785597605721108, -16.63545420775220407, 125.4493079945005150 ) ) ;
#4189 = B_SPLINE_CURVE_WITH_KNOTS ( 'NONE', 3,
 ( #1270, #23925, #18670, #16057, #8681, #11453, #18823, #4237, #31806, #23609, #9316, #26714, #3579 ),
 .UNSPECIFIED., .F., .F.,
 ( 4, 3, 3, 3, 4 ),
 ( 0.000000000000000000, 3.644429809543512820E-05, 7.713354915361920658E-05, 0.0001101572536102696351, 0.0001291034991527052127 ),
 .UNSPECIFIED. ) ;
#4190 = AXIS2_PLACEMENT_3D ( 'NONE', #30921, #5814, #25981 ) ;
#4191 = AXIS2_PLACEMENT_3D ( 'NONE', #17329, #28132, #15813 ) ;
#4192 = ORIENTED_EDGE ( 'NONE', *, *, #12171, .T. ) ;
#4193 = CARTESIAN_POINT ( 'NONE',  ( -40.99628586177130529, 8.927770518203464789, 57.04930799450051637 ) ) ;
#4194 = LINE ( 'NONE', #21257, #9997 ) ;
#4195 = DIRECTION ( 'NONE',  ( 2.946248497964555786E-19, 3.001156285468303092E-19, 1.000000000000000000 ) ) ;
#4196 = LINE ( 'NONE', #14218, #2278 ) ;
#4197 = DIRECTION ( 'NONE',  ( -1.000000000000000000, 0.000000000000000000, 0.000000000000000000 ) ) ;
#4198 = VERTEX_POINT ( 'NONE', #19641 ) ;
#4199 = FACE_OUTER_BOUND ( 'NONE', #17319, .T. ) ;
#4200 = DIRECTION ( 'NONE',  ( 0.9612616959383221138, 0.2756373558169876170, 0.000000000000000000 ) ) ;
#4201 = ORIENTED_EDGE ( 'NONE', *, *, #20155, .T. ) ;
#4202 = EDGE_CURVE ( 'NONE', #16708, #2250, #10489, .T. ) ;
#4203 = DIRECTION ( 'NONE',  ( 1.234978253042719660E-16, -1.000000000000000000, -1.109335647967047851E-31 ) ) ;
#4204 = AXIS2_PLACEMENT_3D ( 'NONE', #11785, #4060, #1122 ) ;
#4205 = CIRCLE ( 'NONE', #26199, 0.1000000000000014905 ) ;
#4206 = PLANE ( 'NONE',  #22692 ) ;
#4207 = EDGE_LOOP ( 'NONE', ( #21113, #24059, #31568, #17443 ) ) ;
#4208 = AXIS2_PLACEMENT_3D ( 'NONE', #30602, #385, #8112 ) ;
#4209 = ORIENTED_EDGE ( 'NONE', *, *, #4708, .T. ) ;
#4210 = CIRCLE ( 'NONE', #22542, 0.1249999999999966416 ) ;
#4211 = VECTOR ( 'NONE', #12710, 1000.000000000000000 ) ;
#4212 = ORIENTED_EDGE ( 'NONE', *, *, #21642, .T. ) ;
#4213 = EDGE_CURVE ( 'NONE', #26728, #28996, #20961, .T. ) ;
#4214 = AXIS2_PLACEMENT_3D ( 'NONE', #27448, #4963, #19885 ) ;
#4215 = ADVANCED_FACE ( 'NONE', ( #12442 ), #6863, .F. ) ;
#4216 = CYLINDRICAL_SURFACE ( 'NONE', #2529, 0.1000000000000014905 ) ;
#4217 = EDGE_CURVE ( 'NONE', #1940, #28369, #517, .T. ) ;
#4218 = CIRCLE ( 'NONE', #15242, 0.1000000000000006301 ) ;
#4219 = EDGE_LOOP ( 'NONE', ( #12264, #18361, #29054, #29638 ) ) ;
#4220 = DIRECTION ( 'NONE',  ( -1.101824276508909887E-16, 1.000000000000000000, -0.000000000000000000 ) ) ;
#4221 = ADVANCED_FACE ( 'NONE', ( #22270 ), #14159, .T. ) ;
#4222 = DIRECTION ( 'NONE',  ( -0.000000000000000000, -1.000000000000000000, -0.000000000000000000 ) ) ;
#4223 = AXIS2_PLACEMENT_3D ( 'NONE', #9362, #19356, #15573 ) ;
#4224 = DIRECTION ( 'NONE',  ( -0.000000000000000000, -1.000000000000000000, -0.000000000000000000 ) ) ;
#4225 = DIRECTION ( 'NONE',  ( -0.000000000000000000, 1.000000000000000000, -0.000000000000000000 ) ) ;
#4226 = CARTESIAN_POINT ( 'NONE',  ( 46.99218062947583974, 29.30286309983297954, 49.08406571254116102 ) ) ;
#4227 = AXIS2_PLACEMENT_3D ( 'NONE', #5372, #15374, #7995 ) ;
#4228 = CIRCLE ( 'NONE', #17243, 0.1250000000000001110 ) ;
#4229 = EDGE_LOOP ( 'NONE', ( #3086, #2109, #18719, #13884, #1873, #12457, #27366, #9754, #1869, #10125, #28331, #6387, #19755, #31230, #16179, #22211 ) ) ;
#4230 = DIRECTION ( 'NONE',  ( 0.2756373558169959437, -0.9612616959383197823, 0.000000000000000000 ) ) ;
#4231 = ORIENTED_EDGE ( 'NONE', *, *, #30871, .F. ) ;
#4232 = CARTESIAN_POINT ( 'NONE',  ( 21.09992658989238734, 31.71664230456639544, 47.04930799450051637 ) ) ;
#4233 = ORIENTED_EDGE ( 'NONE', *, *, #6806, .F. ) ;
#4234 = DIRECTION ( 'NONE',  ( -0.000000000000000000, -1.000000000000000000, -0.000000000000000000 ) ) ;
#4235 = DIRECTION ( 'NONE',  ( -1.000000000000000000, 0.000000000000000000, 0.000000000000000000 ) ) ;
#4236 = CARTESIAN_POINT ( 'NONE',  ( 21.09785597605720753, 14.86454579224779948, 47.04930799450052348 ) ) ;
#4237 = CARTESIAN_POINT ( 'NONE',  ( -40.68879370032178144, 6.799057175545572207, 39.36235710484030648 ) ) ;
#4238 = CARTESIAN_POINT ( 'NONE',  ( -40.52064562223811350, 7.631811404637807605, 60.17616806781843763 ) ) ;
#4239 = CARTESIAN_POINT ( 'NONE',  ( 44.09250526802607340, 28.05621246473836905, 46.89322480343881949 ) ) ;
#4240 = CARTESIAN_POINT ( 'NONE',  ( 47.57660806753134608, 22.93328494799376216, 48.69940892914074482 ) ) ;
#4241 = CARTESIAN_POINT ( 'NONE',  ( 21.09785597605720042, 13.74476430820393347, -7.250692005499486115 ) ) ;
#4242 = ORIENTED_EDGE ( 'NONE', *, *, #18829, .F. ) ;
#4243 = DIRECTION ( 'NONE',  ( -1.101824276508909887E-16, 1.000000000000000000, -0.000000000000000000 ) ) ;
#4244 = CARTESIAN_POINT ( 'NONE',  ( 49.40414881150628901, 22.86454579224779948, 47.16908566558146987 ) ) ;
#4245 = CIRCLE ( 'NONE', #25216, 0.1250000000000001110 ) ;
#4246 = CARTESIAN_POINT ( 'NONE',  ( 60.59785597605719687, -5.098646251524523443, 47.04930799450051637 ) ) ;
#4247 = DIRECTION ( 'NONE',  ( 2.779292025043186357E-18, -1.288349127009862211E-17, 1.000000000000000000 ) ) ;
#4248 = ORIENTED_EDGE ( 'NONE', *, *, #25645, .F. ) ;
#4249 = FACE_OUTER_BOUND ( 'NONE', #4675, .T. ) ;
#4250 = EDGE_LOOP ( 'NONE', ( #6915, #11061 ) ) ;
#4251 = DIRECTION ( 'NONE',  ( 0.000000000000000000, -1.000000000000000000, 0.000000000000000000 ) ) ;
#4252 = ORIENTED_EDGE ( 'NONE', *, *, #2598, .F. ) ;
#4253 = TOROIDAL_SURFACE ( 'NONE', #27835, 14.00178401536290806, 0.5000000000000004441 ) ;
#4254 = EDGE_CURVE ( 'NONE', #2898, #12194, #9698, .T. ) ;
#4255 = CIRCLE ( 'NONE', #6355, 0.09999999999999795164 ) ;
#4256 = CONICAL_SURFACE ( 'NONE', #10035, 54.74424859897010975, 1.291543646475813212 ) ;
#4257 = ADVANCED_FACE ( 'NONE', ( #9811 ), #19805, .F. ) ;
#4258 = ORIENTED_EDGE ( 'NONE', *, *, #16249, .T. ) ;
#4259 = CARTESIAN_POINT ( 'NONE',  ( 21.09785597605719332, 34.11266481626051217, 47.04930799450051637 ) ) ;
#4260 = CARTESIAN_POINT ( 'NONE',  ( -9.728297238921268075, -5.935454207752198563, 132.0493079945005377 ) ) ;
#4261 = DIRECTION ( 'NONE',  ( -0.000000000000000000, -1.000000000000000000, 0.000000000000000000 ) ) ;
#4262 = EDGE_CURVE ( 'NONE', #14332, #21437, #12425, .T. ) ;
#4263 = EDGE_LOOP ( 'NONE', ( #12466, #5613, #11706, #20959 ) ) ;
#4264 = ADVANCED_FACE ( 'NONE', ( #30492 ), #22563, .F. ) ;
#4265 = DIRECTION ( 'NONE',  ( -1.000000000000000000, 0.000000000000000000, 0.000000000000000000 ) ) ;
#4266 = CARTESIAN_POINT ( 'NONE',  ( -38.41701585771487260, 6.978388747684010518, 62.04930799450052348 ) ) ;
#4267 = DIRECTION ( 'NONE',  ( -1.101824276508909887E-16, 1.000000000000000000, -0.000000000000000000 ) ) ;
#4268 = ORIENTED_EDGE ( 'NONE', *, *, #7759, .T. ) ;
#4269 = CARTESIAN_POINT ( 'NONE',  ( 21.09785597605719332, 6.671061906060458568, 26.46581169565308755 ) ) ;
#4270 = VERTEX_POINT ( 'NONE', #15539 ) ;
#4271 = CIRCLE ( 'NONE', #7967, 0.1250000000000018319 ) ;
#4272 = CARTESIAN_POINT ( 'NONE',  ( 47.79865503179234310, 9.702389020015065313, 98.41455612196619995 ) ) ;
#4273 = DIRECTION ( 'NONE',  ( -1.101824276508909887E-16, 1.000000000000000000, -0.000000000000000000 ) ) ;
#4274 = CIRCLE ( 'NONE', #28392, 12.36707279061065279 ) ;
#4275 = DIRECTION ( 'NONE',  ( -1.101824276508909887E-16, 1.000000000000000000, -0.000000000000000000 ) ) ;
#4276 = AXIS2_PLACEMENT_3D ( 'NONE', #40, #27452, #29589 ) ;
#4277 = DIRECTION ( 'NONE',  ( 0.6000000000000011990, 0.000000000000000000, 0.7999999999999990452 ) ) ;
#4278 = ORIENTED_EDGE ( 'NONE', *, *, #10988, .F. ) ;
#4279 = ORIENTED_EDGE ( 'NONE', *, *, #583, .T. ) ;
#4280 = CARTESIAN_POINT ( 'NONE',  ( 35.56915586375611582, -13.30632128221581212, -6.978462942695603743 ) ) ;
#4281 = CARTESIAN_POINT ( 'NONE',  ( -42.38687957179150345, 4.148162238788003719, 58.94930799450051495 ) ) ;
#4282 = CARTESIAN_POINT ( 'NONE',  ( -10.18637189516808661, -5.903366343041435371, 106.3819261045487536 ) ) ;
#4283 = ORIENTED_EDGE ( 'NONE', *, *, #26524, .T. ) ;
#4284 = CARTESIAN_POINT ( 'NONE',  ( -12.64433984712379022, -2.833757427854236788, -8.318886203631619125 ) ) ;
#4285 = DIRECTION ( 'NONE',  ( 0.4848096202463637039, 0.8746197071393810862, 0.000000000000000000 ) ) ;
#4286 = ORIENTED_EDGE ( 'NONE', *, *, #11091, .F. ) ;
#4287 = FACE_OUTER_BOUND ( 'NONE', #14635, .T. ) ;
#4288 = DIRECTION ( 'NONE',  ( -1.101824276508909887E-16, 1.000000000000000000, -0.000000000000000000 ) ) ;
#4289 = VECTOR ( 'NONE', #25715, 1000.000000000000114 ) ;
#4290 = DIRECTION ( 'NONE',  ( -0.2756373558169974980, 0.9612616959383193382, 1.315048337272770589E-17 ) ) ;
#4291 = EDGE_LOOP ( 'NONE', ( #12065, #32115, #13056, #24213 ) ) ;
#4292 = AXIS2_PLACEMENT_3D ( 'NONE', #30765, #18115, #27978 ) ;
#4293 = VECTOR ( 'NONE', #23197, 1000.000000000000000 ) ;
#4294 = DIRECTION ( 'NONE',  ( -1.000000000000000000, 0.000000000000000000, 0.000000000000000000 ) ) ;
#4295 = DIRECTION ( 'NONE',  ( 0.000000000000000000, 0.000000000000000000, 1.000000000000000000 ) ) ;
#4296 = CARTESIAN_POINT ( 'NONE',  ( -40.65065394966018175, 6.870367549600009838, 34.94083608680406172 ) ) ;
#4297 = CARTESIAN_POINT ( 'NONE',  ( 48.18662509608405031, 27.98284706826092716, 49.18364984542562013 ) ) ;
#4298 = EDGE_CURVE ( 'NONE', #10117, #14884, #25873, .T. ) ;
#4299 = ORIENTED_EDGE ( 'NONE', *, *, #3928, .T. ) ;
#4300 = EDGE_CURVE ( 'NONE', #18077, #2557, #8928, .T. ) ;
#4301 = EDGE_CURVE ( 'NONE', #23854, #28828, #13144, .T. ) ;
#4302 = DIRECTION ( 'NONE',  ( 0.000000000000000000, 0.000000000000000000, -1.000000000000000000 ) ) ;
#4303 = CARTESIAN_POINT ( 'NONE',  ( 21.09785597605720042, -13.37218737171702543, 47.04930799450051637 ) ) ;
#4304 = AXIS2_PLACEMENT_3D ( 'NONE', #7479, #29300, #27003 ) ;
#4305 = CARTESIAN_POINT ( 'NONE',  ( 49.40959608158721039, 8.185031362399394439, -3.493091127261788387 ) ) ;
#4306 = CARTESIAN_POINT ( 'NONE',  ( 21.09785597605719332, -16.72540370141334520, 47.04930799450051637 ) ) ;
#4307 = CARTESIAN_POINT ( 'NONE',  ( 21.09785597605719332, 24.86454579224780304, 47.04930799450051637 ) ) ;
#4308 = DIRECTION ( 'NONE',  ( -1.101824276508909887E-16, 1.000000000000000000, -0.000000000000000000 ) ) ;
#4309 = DIRECTION ( 'NONE',  ( 0.2756373558169973870, -0.9612616959383193382, -1.315048337272770280E-17 ) ) ;
#4310 = AXIS2_PLACEMENT_3D ( 'NONE', #3532, #16931, #19222 ) ;
#4311 = CARTESIAN_POINT ( 'NONE',  ( -40.56598700578888383, 6.841196339308488028, 39.54930799450052348 ) ) ;
#4312 = SHAPE_REPRESENTATION_RELATIONSHIP ( 'NONE' , 'NONE' ,  #3604, #11641 ) ;
#4313 = ORIENTED_EDGE ( 'NONE', *, *, #4109, .T. ) ;
#4314 = DIRECTION ( 'NONE',  ( -1.000000000000000000, 0.000000000000000000, 0.000000000000000000 ) ) ;
#4315 = DIRECTION ( 'NONE',  ( -0.02617694830786587365, -1.759793992609925531E-18, 0.9996573249755574819 ) ) ;
#4316 = COLOUR_RGB ( '',0.7921568627450980005, 0.8196078431372548767, 0.9333333333333333481 ) ;
#4317 = CARTESIAN_POINT ( 'NONE',  ( -40.15611298324447631, 6.923081382651430360, 34.55058768090939481 ) ) ;
#4318 = CARTESIAN_POINT ( 'NONE',  ( 21.09785597605719332, 40.56454579224779877, 47.04930799450051637 ) ) ;
#4319 = ORIENTED_EDGE ( 'NONE', *, *, #13621, .T. ) ;
#4320 = AXIS2_PLACEMENT_3D ( 'NONE', #30014, #25080, #22611 ) ;
#4321 = CARTESIAN_POINT ( 'NONE',  ( -39.57114867957335491, -5.935958996647427988, 77.90247845943434868 ) ) ;
#4322 = DIRECTION ( 'NONE',  ( -1.000000000000000000, 0.000000000000000000, 0.000000000000000000 ) ) ;
#4323 = DIRECTION ( 'NONE',  ( -0.4848096202463636484, -0.8746197071393810862, 0.000000000000000000 ) ) ;
#4324 = ORIENTED_EDGE ( 'NONE', *, *, #14231, .F. ) ;
#4325 = ORIENTED_EDGE ( 'NONE', *, *, #15361, .T. ) ;
#4326 = CARTESIAN_POINT ( 'NONE',  ( -40.11708823821248160, 6.803395581744264398, 39.44983305153184716 ) ) ;
#4327 = AXIS2_PLACEMENT_3D ( 'NONE', #2386, #7142, #7307 ) ;
#4328 = CARTESIAN_POINT ( 'NONE',  ( 48.94625023931840246, 29.55784706826092645, 46.10640627770150246 ) ) ;
#4329 = DIRECTION ( 'NONE',  ( 0.4441739386572013393, 0.2110602665713099402, 0.8707256032141217350 ) ) ;
#4330 = DIRECTION ( 'NONE',  ( -0.9612616959383194493, -0.2756373558169972759, -8.795445018804905742E-19 ) ) ;
#4331 = ORIENTED_EDGE ( 'NONE', *, *, #31682, .T. ) ;
#4332 = CARTESIAN_POINT ( 'NONE',  ( 45.32865359766977775, 29.36272681631152182, 48.52962753590826850 ) ) ;
#4333 = ORIENTED_EDGE ( 'NONE', *, *, #3746, .T. ) ;
#4334 = EDGE_CURVE ( 'NONE', #29845, #29925, #24684, .T. ) ;
#4335 = ORIENTED_EDGE ( 'NONE', *, *, #14948, .T. ) ;
#4336 = CONICAL_SURFACE ( 'NONE', #15873, 31.29999999999997939, 0.7853981633974482790 ) ;
#4337 = VECTOR ( 'NONE', #8384, 1000.000000000000000 ) ;
#4338 = DIRECTION ( 'NONE',  ( 0.9612616959383167847, 0.2756373558170070459, -6.299214802459322763E-15 ) ) ;
#4339 = EDGE_CURVE ( 'NONE', #29876, #31613, #29914, .T. ) ;
#4340 = EDGE_CURVE ( 'NONE', #5527, #631, #23350, .T. ) ;
#4341 = EDGE_CURVE ( 'NONE', #2499, #28788, #438, .T. ) ;
#4342 = AXIS2_PLACEMENT_3D ( 'NONE', #9129, #1901, #11912 ) ;
#4343 = CYLINDRICAL_SURFACE ( 'NONE', #3475, 1.199999999999999734 ) ;
#4344 = CYLINDRICAL_SURFACE ( 'NONE', #30292, 12.62506659569710266 ) ;
#4345 = DIRECTION ( 'NONE',  ( -1.000000000000000000, -1.101824276508909887E-16, 0.000000000000000000 ) ) ;
#4346 = EDGE_CURVE ( 'NONE', #28560, #5653, #22920, .T. ) ;
#4347 = ORIENTED_EDGE ( 'NONE', *, *, #33, .F. ) ;
#4348 = FACE_OUTER_BOUND ( 'NONE', #22661, .T. ) ;
#4349 = VERTEX_POINT ( 'NONE', #5379 ) ;
#4350 = FACE_OUTER_BOUND ( 'NONE', #5588, .T. ) ;
#4351 = CARTESIAN_POINT ( 'NONE',  ( 21.09785597605720042, -16.03545420775219910, 47.04930799450051637 ) ) ;
#4352 = CARTESIAN_POINT ( 'NONE',  ( -41.01929587258828747, 9.401204285752060130, 39.44930799450052206 ) ) ;
#4353 = ORIENTED_EDGE ( 'NONE', *, *, #18364, .F. ) ;
#4354 = DIRECTION ( 'NONE',  ( -1.000000000000000000, 0.000000000000000000, 0.000000000000000000 ) ) ;
#4355 = DIRECTION ( 'NONE',  ( -1.000000000000000000, 0.000000000000000000, 0.000000000000000000 ) ) ;
#4356 = DIRECTION ( 'NONE',  ( -0.000000000000000000, -1.000000000000000000, 0.000000000000000000 ) ) ;
#4357 = CARTESIAN_POINT ( 'NONE',  ( 33.50134396954520355, 30.84164230456639544, 47.04930799450051637 ) ) ;
#4358 = DIRECTION ( 'NONE',  ( -1.000000000000000000, -1.101824276508909887E-16, 0.000000000000000000 ) ) ;
#4359 = VECTOR ( 'NONE', #6059, 1000.000000000000114 ) ;
#4360 = DIRECTION ( 'NONE',  ( -0.000000000000000000, -1.000000000000000000, 0.000000000000000000 ) ) ;
#4361 = ORIENTED_EDGE ( 'NONE', *, *, #23247, .T. ) ;
#4362 = DIRECTION ( 'NONE',  ( -1.101824276508909887E-16, 1.000000000000000000, -0.000000000000000000 ) ) ;
#4363 = CIRCLE ( 'NONE', #8557, 0.09999999999999815981 ) ;
#4364 = ORIENTED_EDGE ( 'NONE', *, *, #17818, .T. ) ;
#4365 = LINE ( 'NONE', #4856, #30847 ) ;
#4366 = DIRECTION ( 'NONE',  ( -1.224646799147353207E-16, -1.349345573449484691E-32, 1.000000000000000000 ) ) ;
#4367 = ORIENTED_EDGE ( 'NONE', *, *, #8099, .T. ) ;
#4368 = AXIS2_PLACEMENT_3D ( 'NONE', #12576, #3677, #8135 ) ;
#4369 = ORIENTED_EDGE ( 'NONE', *, *, #11634, .F. ) ;
#4370 = ADVANCED_FACE ( 'NONE', ( #7681 ), #23627, .T. ) ;
#4371 = EDGE_CURVE ( 'NONE', #154, #7848, #7372, .T. ) ;
#4372 = VERTEX_POINT ( 'NONE', #769 ) ;
#4373 = TOROIDAL_SURFACE ( 'NONE', #13306, 12.40141737965284996, 0.1250000000000002776 ) ;
#4374 = DIRECTION ( 'NONE',  ( 0.2756373558169926685, -0.9612616959383207815, -1.315048337272770743E-17 ) ) ;
#4375 = ADVANCED_FACE ( 'NONE', ( #25236 ), #22762, .T. ) ;
#4376 = ORIENTED_EDGE ( 'NONE', *, *, #29908, .F. ) ;
#4377 = EDGE_LOOP ( 'NONE', ( #27224, #28856, #6580, #19903 ) ) ;
#4378 = TOROIDAL_SURFACE ( 'NONE', #19035, 2.799999999999998490, 0.2999999999999999334 ) ;
#4379 = CARTESIAN_POINT ( 'NONE',  ( -39.67555847965937943, 2.645252416024336028, 45.84930799450051353 ) ) ;
#4380 = CIRCLE ( 'NONE', #19038, 0.1000000000000018235 ) ;
#4381 = CARTESIAN_POINT ( 'NONE',  ( 33.37634396954523908, 27.84164230456639544, 47.04930799450051637 ) ) ;
#4382 = DIRECTION ( 'NONE',  ( 0.000000000000000000, 0.000000000000000000, -1.000000000000000000 ) ) ;
#4383 = CARTESIAN_POINT ( 'NONE',  ( 45.81741271322955100, 27.84452976649965450, 49.02305402274571122 ) ) ;
#4384 = EDGE_LOOP ( 'NONE', ( #865, #24429, #25277, #4233 ) ) ;
#4385 = CARTESIAN_POINT ( 'NONE',  ( -40.21210701746133509, 7.644196001419694575, 60.29072935073781991 ) ) ;
#4386 = VERTEX_POINT ( 'NONE', #6657 ) ;
#4387 = CARTESIAN_POINT ( 'NONE',  ( -10.13620514147193141, 3.957035103101699480, -4.501820123519951977 ) ) ;
#4388 = ORIENTED_EDGE ( 'NONE', *, *, #18409, .F. ) ;
#4389 = DIRECTION ( 'NONE',  ( 0.000000000000000000, 0.000000000000000000, 1.000000000000000000 ) ) ;
#4390 = DIRECTION ( 'NONE',  ( 0.000000000000000000, 0.000000000000000000, -1.000000000000000000 ) ) ;
#4391 = DIRECTION ( 'NONE',  ( -1.000000000000000000, 0.000000000000000000, 0.000000000000000000 ) ) ;
#4392 = CARTESIAN_POINT ( 'NONE',  ( 33.46699938050304013, 30.96183152705961206, 47.04930799450051637 ) ) ;
#4393 = CARTESIAN_POINT ( 'NONE',  ( -43.37834615508418068, 1.121909970995877082, 39.44930799450052916 ) ) ;
#4394 = CARTESIAN_POINT ( 'NONE',  ( 47.23302798462060537, 25.78121246473837758, 44.44659793406428605 ) ) ;
#4395 = AXIS2_PLACEMENT_3D ( 'NONE', #14861, #24867, #9606 ) ;
#4396 = CARTESIAN_POINT ( 'NONE',  ( 47.00684970613776414, 22.92747281079970278, 48.80161379910075681 ) ) ;
#4397 = DIRECTION ( 'NONE',  ( 0.000000000000000000, 0.000000000000000000, 1.000000000000000000 ) ) ;
#4398 = EDGE_CURVE ( 'NONE', #24757, #20619, #10538, .T. ) ;
#4399 = EDGE_LOOP ( 'NONE', ( #16639, #14822, #774, #8017 ) ) ;
#4400 = DIRECTION ( 'NONE',  ( -1.000000000000000000, -1.101824276508909887E-16, 0.000000000000000000 ) ) ;
#4401 = DIRECTION ( 'NONE',  ( -0.9612616959383198934, -0.2756373558169956106, 0.000000000000000000 ) ) ;
#4402 = DIRECTION ( 'NONE',  ( -1.000000000000000000, -1.101824276508909764E-16, 0.000000000000000000 ) ) ;
#4403 = ADVANCED_FACE ( 'NONE', ( #20942 ), #16500, .T. ) ;
#4404 = CARTESIAN_POINT ( 'NONE',  ( 48.15507178867567717, 22.98879437201065912, 46.03001840850954807 ) ) ;
#4405 = DIRECTION ( 'NONE',  ( -1.000000000000000000, -1.101824276508909887E-16, 0.000000000000000000 ) ) ;
#4406 = VERTEX_POINT ( 'NONE', #921 ) ;
#4407 = CIRCLE ( 'NONE', #18609, 78.39999999999999147 ) ;
#4408 = DIRECTION ( 'NONE',  ( 0.000000000000000000, 0.000000000000000000, -1.000000000000000000 ) ) ;
#4409 = ORIENTED_EDGE ( 'NONE', *, *, #26266, .F. ) ;
#4410 = CARTESIAN_POINT ( 'NONE',  ( 65.59785597605720397, 13.86454579224779948, 47.04930799450051637 ) ) ;
#4411 = CARTESIAN_POINT ( 'NONE',  ( 8.698509210239528500, 26.34164230456639899, 47.04930799450051637 ) ) ;
#4412 = EDGE_CURVE ( 'NONE', #2185, #21311, #4218, .T. ) ;
#4413 = EDGE_CURVE ( 'NONE', #29185, #26331, #2655, .T. ) ;
#4414 = ADVANCED_FACE ( 'NONE', ( #3706 ), #30971, .T. ) ;
#4415 = ORIENTED_EDGE ( 'NONE', *, *, #14632, .F. ) ;
#4416 = VERTEX_POINT ( 'NONE', #6170 ) ;
#4417 = DIRECTION ( 'NONE',  ( -1.101824276508909887E-16, 1.000000000000000000, -0.000000000000000000 ) ) ;
#4418 = EDGE_CURVE ( 'NONE', #27343, #4474, #20481, .T. ) ;
#4419 = DIRECTION ( 'NONE',  ( 0.000000000000000000, -0.000000000000000000, -1.000000000000000000 ) ) ;
#4420 = DIRECTION ( 'NONE',  ( -1.000000000000000000, 0.000000000000000000, 0.000000000000000000 ) ) ;
#4421 = ORIENTED_EDGE ( 'NONE', *, *, #10351, .T. ) ;
#4422 = AXIS2_PLACEMENT_3D ( 'NONE', #8583, #27967, #715 ) ;
#4423 = FACE_OUTER_BOUND ( 'NONE', #31942, .T. ) ;
#4424 = MECHANICAL_DESIGN_GEOMETRIC_PRESENTATION_REPRESENTATION (  '', ( #22245 ), #10615 ) ;
#4425 = CARTESIAN_POINT ( 'NONE',  ( 8.698509210239553369, 28.59164230456639544, 47.04930799450051637 ) ) ;
#4426 = CARTESIAN_POINT ( 'NONE',  ( 78.30589944682461123, -4.922489993312327172, 14.14175782364709022 ) ) ;
#4427 = TOROIDAL_SURFACE ( 'NONE', #236, 12.40141737965280733, 0.1250000000000013878 ) ;
#4428 = ORIENTED_EDGE ( 'NONE', *, *, #5169, .F. ) ;
#4429 = EDGE_LOOP ( 'NONE', ( #11142, #29816 ) ) ;
#4431 = CARTESIAN_POINT ( 'NONE',  ( 21.09785597605719332, -13.49020584019834601, 105.1414762132873193 ) ) ;
#4430 = TOROIDAL_SURFACE ( 'NONE', #9136, 67.99999999999997158, 3.299999999999999822 ) ;
#4432 = CIRCLE ( 'NONE', #11798, 12.62506659569710266 ) ;
#4433 = EDGE_LOOP ( 'NONE', ( #31520, #28479, #26857, #32336 ) ) ;
#4434 = DIRECTION ( 'NONE',  ( 0.000000000000000000, 1.000000000000000000, 0.000000000000000000 ) ) ;
#4435 = FACE_OUTER_BOUND ( 'NONE', #24062, .T. ) ;
#4436 = DIRECTION ( 'NONE',  ( -1.000000000000000000, -1.101824276508909887E-16, 0.000000000000000000 ) ) ;
#4437 = ADVANCED_FACE ( 'NONE', ( #29144 ), #8422, .T. ) ;
#4438 = EDGE_LOOP ( 'NONE', ( #21987, #25905, #2521, #26758 ) ) ;
#4439 = EDGE_LOOP ( 'NONE', ( #9037, #18861 ) ) ;
#4440 = CARTESIAN_POINT ( 'NONE',  ( 76.91070899933976079, -13.30632128221581212, 50.70225068270534763 ) ) ;
#4441 = DIRECTION ( 'NONE',  ( -0.2756373558169956106, 0.9612616959383197823, 0.000000000000000000 ) ) ;
#4442 = ADVANCED_FACE ( 'NONE', ( #16650 ), #20994, .T. ) ;
#4443 = FACE_OUTER_BOUND ( 'NONE', #10671, .T. ) ;
#4444 = EDGE_LOOP ( 'NONE', ( #6813, #8336, #26570, #30583, #8215, #19693 ) ) ;
#4445 = CARTESIAN_POINT ( 'NONE',  ( -11.46327885171858441, 1.504766047489272562, -6.222272583143227287 ) ) ;
#4446 = CARTESIAN_POINT ( 'NONE',  ( 21.09785597605720042, -13.37218737171702543, 47.04930799450051637 ) ) ;
#4447 = ORIENTED_EDGE ( 'NONE', *, *, #5423, .T. ) ;
#4448 = FACE_OUTER_BOUND ( 'NONE', #2255, .T. ) ;
#4449 = LINE ( 'NONE', #19538, #12050 ) ;
#4450 = ADVANCED_FACE ( 'NONE', ( #13891 ), #18787, .F. ) ;
#4451 = CARTESIAN_POINT ( 'NONE',  ( 21.09992658989239089, 30.59184655352422411, 47.04930799450051637 ) ) ;
#4452 = CIRCLE ( 'NONE', #28032, 0.2000000000000005107 ) ;
#4453 = AXIS2_PLACEMENT_3D ( 'NONE', #1808, #8867, #23799 ) ;
#4454 = AXIS2_PLACEMENT_3D ( 'NONE', #22592, #111, #27854 ) ;
#4455 = VECTOR ( 'NONE', #27324, 1000.000000000000000 ) ;
#4456 = CIRCLE ( 'NONE', #16491, 1.500000000000001332 ) ;
#4457 = EDGE_LOOP ( 'NONE', ( #25748, #15735, #1267, #14519 ) ) ;
#4458 = DIRECTION ( 'NONE',  ( 0.000000000000000000, -1.000000000000000000, 0.000000000000000000 ) ) ;
#4459 = DIRECTION ( 'NONE',  ( -1.000000000000000000, 0.000000000000000000, 0.000000000000000000 ) ) ;
#4460 = DIRECTION ( 'NONE',  ( -0.000000000000000000, 1.000000000000000000, -0.000000000000000000 ) ) ;
#4461 = CARTESIAN_POINT ( 'NONE',  ( 48.83862994770794330, 29.44118040159425931, 48.17861352429476796 ) ) ;
#4462 = VERTEX_POINT ( 'NONE', #23891 ) ;
#4463 = DIRECTION ( 'NONE',  ( 0.9612616959383205595, 0.2756373558169932236, -1.660411357259282445E-16 ) ) ;
#4464 = DIRECTION ( 'NONE',  ( 0.2756373558169954441, -0.9612616959383198934, 1.479773560108263204E-16 ) ) ;
#4465 = CARTESIAN_POINT ( 'NONE',  ( -40.11286833322908052, 2.887657226147511302, 57.04930799450051637 ) ) ;
#4466 = FACE_OUTER_BOUND ( 'NONE', #10088, .T. ) ;
#4467 = CARTESIAN_POINT ( 'NONE',  ( 21.09785597605719332, 17.16451738380053271, 47.04930799450051637 ) ) ;
#4468 = CARTESIAN_POINT ( 'NONE',  ( 21.09785597605719332, 47.94190058235918173, 47.04930799450051637 ) ) ;
#4469 = CARTESIAN_POINT ( 'NONE',  ( 21.09785597605719332, 30.56454579224779522, 47.04930799450051637 ) ) ;
#4470 = CYLINDRICAL_SURFACE ( 'NONE', #5281, 7.999999999999999112 ) ;
#4471 =( BOUNDED_CURVE ( )  B_SPLINE_CURVE ( 3, ( #7914, #5770, #18388, #22992 ),
 .UNSPECIFIED., .F., .F. ) 
 B_SPLINE_CURVE_WITH_KNOTS ( ( 4, 4 ),
 ( 1.570796326794896558, 2.093319089163915070 ),
 .UNSPECIFIED. ) 
 CURVE ( )  GEOMETRIC_REPRESENTATION_ITEM ( )  RATIONAL_B_SPLINE_CURVE ( ( 1.000000000000000000, 0.9773766218976396303, 0.9773766218976396303, 1.000000000000000000 ) ) 
 REPRESENTATION_ITEM ( '' )  );
#4472 = DIRECTION ( 'NONE',  ( 1.234978253042719660E-16, -1.000000000000000000, -1.109335647967047851E-31 ) ) ;
#4473 = AXIS2_PLACEMENT_3D ( 'NONE', #12481, #10018, #27570 ) ;
#4474 = VERTEX_POINT ( 'NONE', #26189 ) ;
#4475 = DIRECTION ( 'NONE',  ( -1.000000000000000000, 0.000000000000000000, 0.000000000000000000 ) ) ;
#4476 = CIRCLE ( 'NONE', #2376, 1.500000000000001332 ) ;
#4477 = B_SPLINE_CURVE_WITH_KNOTS ( 'NONE', 3,
 ( #27117, #26953, #32050, #17429, #2339, #4311, #12524 ),
 .UNSPECIFIED., .F., .F.,
 ( 4, 3, 4 ),
 ( 0.000000000000000000, 5.088378629326043544E-05, 0.0001059921926251528864 ),
 .UNSPECIFIED. ) ;
#4478 = AXIS2_PLACEMENT_3D ( 'NONE', #32260, #12233, #29468 ) ;
#4479 = CARTESIAN_POINT ( 'NONE',  ( 45.91356333913565635, 25.13954579807170475, 44.72770895919563117 ) ) ;
#4480 = CARTESIAN_POINT ( 'NONE',  ( -29.36731150373160659, 9.857091600108821794, 20.53851473532732541 ) ) ;
#4481 = AXIS2_PLACEMENT_3D ( 'NONE', #5961, #10573, #20561 ) ;
#4482 = CARTESIAN_POINT ( 'NONE',  ( 48.83059987400640978, 26.98213139976341068, 48.97189179988551899 ) ) ;
#4483 = ORIENTED_EDGE ( 'NONE', *, *, #7310, .T. ) ;
#4484 = DIRECTION ( 'NONE',  ( -1.000000000000000000, 0.000000000000000000, 0.000000000000000000 ) ) ;
#4485 = CARTESIAN_POINT ( 'NONE',  ( 21.09785597605719332, 14.58544108513610027, 59.78332509433494124 ) ) ;
#4486 = CARTESIAN_POINT ( 'NONE',  ( 49.40414881150629611, 22.86454579224779948, 47.16908566558144855 ) ) ;
#4487 = EDGE_LOOP ( 'NONE', ( #26246, #25574, #8529, #24402 ) ) ;
#4488 = ORIENTED_EDGE ( 'NONE', *, *, #10587, .T. ) ;
#4489 = DIRECTION ( 'NONE',  ( -1.000000000000000000, 0.000000000000000000, 0.000000000000000000 ) ) ;
#4490 = DIRECTION ( 'NONE',  ( -0.9612616959383221138, -0.2756373558169876170, 0.000000000000000000 ) ) ;
#4491 = DIRECTION ( 'NONE',  ( -0.000000000000000000, 1.000000000000000000, -0.000000000000000000 ) ) ;
#4492 = EDGE_CURVE ( 'NONE', #29979, #22133, #4194, .T. ) ;
#4493 = CIRCLE ( 'NONE', #28620, 1.042135311067126979 ) ;
#4494 = ADVANCED_FACE ( 'NONE', ( #21409 ), #1086, .T. ) ;
#4495 = ORIENTED_EDGE ( 'NONE', *, *, #32399, .F. ) ;
#4496 = CARTESIAN_POINT ( 'NONE',  ( 44.78102299139906251, 29.29862254614766925, 46.54638771186188961 ) ) ;
#4497 = ORIENTED_EDGE ( 'NONE', *, *, #20853, .F. ) ;
#4498 = ORIENTED_EDGE ( 'NONE', *, *, #5015, .T. ) ;
#4499 = CARTESIAN_POINT ( 'NONE',  ( 52.12082631206856576, -5.937449718911894436, 107.6772108465075490 ) ) ;
#4500 = CIRCLE ( 'NONE', #2922, 1.300000000000002487 ) ;
#4501 = ORIENTED_EDGE ( 'NONE', *, *, #15892, .F. ) ;
#4502 = CARTESIAN_POINT ( 'NONE',  ( 21.09992658989239089, 29.34184655352418858, 47.04930799450051637 ) ) ;
#4503 = CARTESIAN_POINT ( 'NONE',  ( -32.42863249666554282, -1.325152302235995894, 80.65782899193297339 ) ) ;
#4504 = CARTESIAN_POINT ( 'NONE',  ( -38.65545646816406133, 11.92558985988973497, 67.46350265493038023 ) ) ;
#4505 = TOROIDAL_SURFACE ( 'NONE', #28121, 12.61792373059897088, 0.1249999999999973216 ) ;
#4506 = EDGE_LOOP ( 'NONE', ( #3741, #1457, #31664, #1452 ) ) ;
#4507 = DIRECTION ( 'NONE',  ( -1.000000000000000000, 0.000000000000000000, 0.000000000000000000 ) ) ;
#4508 = VERTEX_POINT ( 'NONE', #11113 ) ;
#4509 = DIRECTION ( 'NONE',  ( 0.000000000000000000, 0.000000000000000000, 1.000000000000000000 ) ) ;
#4510 = DIRECTION ( 'NONE',  ( -0.000000000000000000, -1.000000000000000000, -0.000000000000000000 ) ) ;
#4511 = CARTESIAN_POINT ( 'NONE',  ( -40.68921029693431279, 6.794170072703461294, 39.46947734395037344 ) ) ;
#4512 = ORIENTED_EDGE ( 'NONE', *, *, #10803, .T. ) ;
#4513 = DIRECTION ( 'NONE',  ( -0.5442436726714893203, -6.721291001053903893E-17, 0.8389271868029124501 ) ) ;
#4514 = CARTESIAN_POINT ( 'NONE',  ( 21.09785597605719332, 25.56454579224779167, 60.24930799450052632 ) ) ;
#4515 = FILL_AREA_STYLE ('',( #28654 ) ) ;
#4516 = CARTESIAN_POINT ( 'NONE',  ( 21.09785597605720753, 14.86454579224779948, 47.04930799450052348 ) ) ;
#4517 = DIRECTION ( 'NONE',  ( 1.000000000000000000, 0.000000000000000000, 0.000000000000000000 ) ) ;
#4518 = DIRECTION ( 'NONE',  ( 0.4544104193609913023, 0.000000000000000000, 0.8907924397839084296 ) ) ;
#4519 = PRESENTATION_STYLE_ASSIGNMENT (( #24218 ) ) ;
#4520 = ORIENTED_EDGE ( 'NONE', *, *, #17116, .T. ) ;
#4521 = CARTESIAN_POINT ( 'NONE',  ( -40.05987053574653345, 7.506472619680465641, 35.39279590939684539 ) ) ;
#4522 = FACE_OUTER_BOUND ( 'NONE', #28993, .T. ) ;
#4523 = ORIENTED_EDGE ( 'NONE', *, *, #1416, .F. ) ;
#4524 = DIRECTION ( 'NONE',  ( -1.000000000000000000, 0.000000000000000000, 0.000000000000000000 ) ) ;
#4525 = CIRCLE ( 'NONE', #17090, 12.27641737965284641 ) ;
#4526 = ADVANCED_FACE ( 'NONE', ( #6020 ), #13733, .T. ) ;
#4527 = CARTESIAN_POINT ( 'NONE',  ( -40.90015969217747482, 8.955334253785164123, 56.14611646155296398 ) ) ;
#4528 = EDGE_CURVE ( 'NONE', #22254, #14930, #14721, .T. ) ;
#4529 = ORIENTED_EDGE ( 'NONE', *, *, #20159, .F. ) ;
#4530 = EDGE_CURVE ( 'NONE', #7835, #22873, #541, .T. ) ;
#4531 = ORIENTED_EDGE ( 'NONE', *, *, #22002, .T. ) ;
#4532 = ADVANCED_FACE ( 'NONE', ( #24534 ), #6820, .T. ) ;
#4533 = ADVANCED_FACE ( 'NONE', ( #19447 ), #12629, .T. ) ;
#4534 = AXIS2_PLACEMENT_3D ( 'NONE', #19092, #14200, #29129 ) ;
#4535 = ORIENTED_EDGE ( 'NONE', *, *, #1036, .T. ) ;
#4536 = EDGE_CURVE ( 'NONE', #19129, #4851, #18365, .T. ) ;
#4537 = CARTESIAN_POINT ( 'NONE',  ( 21.09785597605719332, 25.56454579224779167, 47.04930799450051637 ) ) ;
#4538 = ORIENTED_EDGE ( 'NONE', *, *, #12418, .F. ) ;
#4539 = VERTEX_POINT ( 'NONE', #19273 ) ;
#4540 = CARTESIAN_POINT ( 'NONE',  ( -42.32583647289406770, 13.67174551105522617, 59.52414500118048579 ) ) ;
#4541 = DIRECTION ( 'NONE',  ( 0.8746197071393928546, -0.4848096202463424986, -1.277302113040826515E-17 ) ) ;
#4542 = DIRECTION ( 'NONE',  ( -0.000000000000000000, -1.000000000000000000, 0.000000000000000000 ) ) ;
#4543 = CARTESIAN_POINT ( 'NONE',  ( -40.02540636251513462, 2.839176264122873050, 37.04930799450052348 ) ) ;
#4544 = CARTESIAN_POINT ( 'NONE',  ( 8.482002859293407582, 25.21664230456640254, 47.04930799450051637 ) ) ;
#4545 = EDGE_CURVE ( 'NONE', #14867, #11885, #26250, .T. ) ;
#4546 = VERTEX_POINT ( 'NONE', #9449 ) ;
#4547 = CARTESIAN_POINT ( 'NONE',  ( -6.282799519003591016, 9.126991894476592648, 97.50906091218828919 ) ) ;
#4548 = EDGE_LOOP ( 'NONE', ( #7695, #20621 ) ) ;
#4549 = CARTESIAN_POINT ( 'NONE',  ( -11.23515816165873993, -5.485531640240842499, -9.925875039342111350 ) ) ;
#4550 = ORIENTED_EDGE ( 'NONE', *, *, #32280, .F. ) ;
#4551 = CARTESIAN_POINT ( 'NONE',  ( -42.66751614955960292, 15.14923148629343430, 35.64930799450052490 ) ) ;
#4552 = CIRCLE ( 'NONE', #27093, 12.36707279061065101 ) ;
#4553 = CARTESIAN_POINT ( 'NONE',  ( -41.08785830660041682, 9.277514380576530328, 39.54930799450052348 ) ) ;
#4554 = FACE_OUTER_BOUND ( 'NONE', #25039, .T. ) ;
#4555 = CARTESIAN_POINT ( 'NONE',  ( 41.51205063648687599, 11.92558985988973497, -4.944603100128015960 ) ) ;
#4556 = CARTESIAN_POINT ( 'NONE',  ( 49.41945501136223839, 26.36454579807171328, 45.86501535757901848 ) ) ;
#4557 = CARTESIAN_POINT ( 'NONE',  ( 46.93112133629608707, 23.10527865767144817, 47.61204104636720302 ) ) ;
#4558 = CARTESIAN_POINT ( 'NONE',  ( 21.09785597605719332, -5.935454207752083988, 47.04930799450039558 ) ) ;
#4559 = VERTEX_POINT ( 'NONE', #32099 ) ;
#4560 = DIRECTION ( 'NONE',  ( 0.000000000000000000, 0.000000000000000000, -1.000000000000000000 ) ) ;
#4561 = DIRECTION ( 'NONE',  ( 0.000000000000000000, -1.000000000000000000, 0.000000000000000000 ) ) ;
#4562 = CARTESIAN_POINT ( 'NONE',  ( 47.86364407361583062, 22.99884124225578930, 45.86888002329718717 ) ) ;
#4563 = CARTESIAN_POINT ( 'NONE',  ( -38.57628410747783221, -5.432165593243111879, 14.50875660354866703 ) ) ;
#4564 = VERTEX_POINT ( 'NONE', #9609 ) ;
#4565 = ORIENTED_EDGE ( 'NONE', *, *, #18730, .T. ) ;
#4566 = DIRECTION ( 'NONE',  ( -1.000000000000000000, 0.000000000000000000, 0.000000000000000000 ) ) ;
#4567 = EDGE_CURVE ( 'NONE', #27545, #27140, #11558, .T. ) ;
#4568 = CIRCLE ( 'NONE', #23944, 39.69941114636694124 ) ;
#4569 = ORIENTED_EDGE ( 'NONE', *, *, #13901, .F. ) ;
#4570 = ORIENTED_EDGE ( 'NONE', *, *, #2683, .T. ) ;
#4571 = EDGE_CURVE ( 'NONE', #12082, #2410, #16796, .T. ) ;
#4572 = DIRECTION ( 'NONE',  ( -0.2756373558169932236, 0.9612616959383205595, -1.479773560108267395E-16 ) ) ;
#4573 = CARTESIAN_POINT ( 'NONE',  ( 33.71785032049137953, 24.96664230456639899, 47.04930799450051637 ) ) ;
#4574 = CARTESIAN_POINT ( 'NONE',  ( -48.34557642001920641, 3.861744873591483440, 60.44930799450051495 ) ) ;
#4575 = EDGE_CURVE ( 'NONE', #14096, #28333, #31930, .T. ) ;
#4576 = VERTEX_POINT ( 'NONE', #29636 ) ;
#4577 = FACE_OUTER_BOUND ( 'NONE', #22028, .T. ) ;
#4578 = DIRECTION ( 'NONE',  ( 0.000000000000000000, 0.000000000000000000, -1.000000000000000000 ) ) ;
#4579 = CARTESIAN_POINT ( 'NONE',  ( 49.32483701613094240, 26.42587066347689984, 45.91328182968236860 ) ) ;
#4580 = ORIENTED_EDGE ( 'NONE', *, *, #30075, .F. ) ;
#4581 = AXIS2_PLACEMENT_3D ( 'NONE', #21865, #12032, #16614 ) ;
#4582 = EDGE_LOOP ( 'NONE', ( #10714, #25149, #27986, #22308 ) ) ;
#4583 = DIRECTION ( 'NONE',  ( -0.8746197071393890798, 0.4848096202463489934, 8.676864087100840673E-18 ) ) ;
#4584 = EDGE_CURVE ( 'NONE', #14930, #7948, #25203, .T. ) ;
#4585 = AXIS2_PLACEMENT_3D ( 'NONE', #26888, #11797, #29524 ) ;
#4586 = ORIENTED_EDGE ( 'NONE', *, *, #1574, .T. ) ;
#4587 = DIRECTION ( 'NONE',  ( -1.000000000000000000, 0.000000000000000000, 0.000000000000000000 ) ) ;
#4588 = CARTESIAN_POINT ( 'NONE',  ( 21.09992658989238734, 31.09143805560860585, 47.04930799450051637 ) ) ;
#4589 = CARTESIAN_POINT ( 'NONE',  ( 33.50134396954523908, 27.09164230456639899, 47.04930799450051637 ) ) ;
#4590 = PRODUCT_DEFINITION_SHAPE ( 'NONE', 'NONE',  #32499 ) ;
#4591 = VECTOR ( 'NONE', #2541, 1000.000000000000000 ) ;
#4592 = DIRECTION ( 'NONE',  ( -1.000000000000000000, -1.101824276508909887E-16, 0.000000000000000000 ) ) ;
#4593 = CARTESIAN_POINT ( 'NONE',  ( 49.49063479933183629, 29.41291119454914593, 47.17357720316391578 ) ) ;
#4594 = CARTESIAN_POINT ( 'NONE',  ( 0.000000000000000000, 0.000000000000000000, 0.000000000000000000 ) ) ;
#4595 = ORIENTED_EDGE ( 'NONE', *, *, #32322, .F. ) ;
#4596 = ORIENTED_EDGE ( 'NONE', *, *, #19838, .T. ) ;
#4597 = CARTESIAN_POINT ( 'NONE',  ( -42.28651568955962858, 14.71554561121750559, 58.98666529074791498 ) ) ;
#4598 = LINE ( 'NONE', #24458, #980 ) ;
#4599 = AXIS2_PLACEMENT_3D ( 'NONE', #29951, #15487, #15329 ) ;
#4600 = CARTESIAN_POINT ( 'NONE',  ( -38.59984781516420327, -5.935454207752198563, 77.87546120947918382 ) ) ;
#4601 = ORIENTED_EDGE ( 'NONE', *, *, #13315, .F. ) ;
#4602 = LINE ( 'NONE', #3958, #417 ) ;
#4603 = DIRECTION ( 'NONE',  ( 0.000000000000000000, -1.000000000000000000, 0.000000000000000000 ) ) ;
#4604 = EDGE_LOOP ( 'NONE', ( #7449, #30645, #7942, #4501 ) ) ;
#4605 = CARTESIAN_POINT ( 'NONE',  ( 33.46699938050304013, 25.71183152705960140, 47.04930799450051637 ) ) ;
#4606 = DIRECTION ( 'NONE',  ( 1.000000000000000000, 0.000000000000000000, 0.000000000000000000 ) ) ;
#4607 = ADVANCED_FACE ( 'NONE', ( #32423 ), #32015, .F. ) ;
#4608 = CARTESIAN_POINT ( 'NONE',  ( -42.36153388572594736, 13.68895619636815653, 60.54930799450051637 ) ) ;
#4609 = TOROIDAL_SURFACE ( 'NONE', #13021, 0.8928932188134564019, 0.1000000000000000056 ) ;
#4610 = AXIS2_PLACEMENT_3D ( 'NONE', #31469, #23749, #11436 ) ;
#4611 = ORIENTED_EDGE ( 'NONE', *, *, #5533, .F. ) ;
#4612 = CIRCLE ( 'NONE', #22954, 12.36707279061065279 ) ;
#4613 = AXIS2_PLACEMENT_3D ( 'NONE', #5219, #15231, #12451 ) ;
#4614 = EDGE_LOOP ( 'NONE', ( #881, #23097, #19769, #9967 ) ) ;
#4615 = EDGE_CURVE ( 'NONE', #28177, #11145, #22044, .T. ) ;
#4616 = CARTESIAN_POINT ( 'NONE',  ( -43.90780810587784089, -0.03953120679776400692, 62.04930799450052348 ) ) ;
#4617 = CARTESIAN_POINT ( 'NONE',  ( 21.09785597605719332, 11.92558985988973497, 47.04930799450051637 ) ) ;
#4618 = CARTESIAN_POINT ( 'NONE',  ( 46.99023568444673060, 25.82451373492759927, 49.12151524109405898 ) ) ;
#4619 = ADVANCED_FACE ( 'NONE', ( #19935 ), #27004, .F. ) ;
#4620 = AXIS2_PLACEMENT_3D ( 'NONE', #15962, #16120, #11057 ) ;
#4621 = EDGE_LOOP ( 'NONE', ( #28405, #23388, #16140, #21494 ) ) ;
#4622 = CYLINDRICAL_SURFACE ( 'NONE', #30145, 85.00000000000001421 ) ;
#4623 = CARTESIAN_POINT ( 'NONE',  ( 21.09992658989239089, 23.59164230456639544, 47.04930799450051637 ) ) ;
#4624 = CARTESIAN_POINT ( 'NONE',  ( 21.09785597605719332, 24.74924423484549507, 47.04930799450051637 ) ) ;
#4625 = EDGE_CURVE ( 'NONE', #15368, #11910, #23106, .T. ) ;
#4626 = DIRECTION ( 'NONE',  ( 0.000000000000000000, 0.000000000000000000, 1.000000000000000000 ) ) ;
#4627 = EDGE_CURVE ( 'NONE', #26804, #8205, #573, .T. ) ;
#4628 = DIRECTION ( 'NONE',  ( -0.7848668881104203798, -0.2250569586005539691, 0.5773502691896258421 ) ) ;
#4629 = CARTESIAN_POINT ( 'NONE',  ( 21.09992658989239089, 29.59143805560861296, 47.04930799450051637 ) ) ;
#4630 = DIRECTION ( 'NONE',  ( 0.000000000000000000, -1.000000000000000000, 0.000000000000000000 ) ) ;
#4631 = DIRECTION ( 'NONE',  ( 0.000000000000000000, 0.000000000000000000, 1.000000000000000000 ) ) ;
#4632 = FACE_OUTER_BOUND ( 'NONE', #31524, .T. ) ;
#4633 = CYLINDRICAL_SURFACE ( 'NONE', #27883, 12.36707279061065279 ) ;
#4634 = ORIENTED_EDGE ( 'NONE', *, *, #11776, .T. ) ;
#4635 = FACE_OUTER_BOUND ( 'NONE', #8262, .T. ) ;
#4636 = CIRCLE ( 'NONE', #2009, 0.6621856154243859205 ) ;
#4637 = AXIS2_PLACEMENT_3D ( 'NONE', #31998, #14284, #9517 ) ;
#4638 = CARTESIAN_POINT ( 'NONE',  ( 44.43390428149366755, 25.11486642951281212, 45.32110236369020839 ) ) ;
#4639 = CARTESIAN_POINT ( 'NONE',  ( 21.09992658989238734, 38.56284415653841791, 47.04930799450051637 ) ) ;
#4640 = CIRCLE ( 'NONE', #1491, 0.1000000000000008243 ) ;
#4641 = CIRCLE ( 'NONE', #20893, 12.62506659569710443 ) ;
#4642 = CARTESIAN_POINT ( 'NONE',  ( 80.85108986838918099, 5.388785998227653806, 77.62194537253992621 ) ) ;
#4643 = VERTEX_POINT ( 'NONE', #14375 ) ;
#4644 = DIRECTION ( 'NONE',  ( -1.000000000000000000, 0.000000000000000000, 0.000000000000000000 ) ) ;
#4645 = CARTESIAN_POINT ( 'NONE',  ( 21.09785597605719332, 17.16451738380053271, 34.26511779397349500 ) ) ;
#4646 = DIRECTION ( 'NONE',  ( -0.4848096202463627602, -0.8746197071393815303, 0.000000000000000000 ) ) ;
#4647 = CONICAL_SURFACE ( 'NONE', #9352, 0.9031915329475502796, 0.7853981633974456145 ) ;
#4648 = VERTEX_POINT ( 'NONE', #24372 ) ;
#4649 = VERTEX_POINT ( 'NONE', #31769 ) ;
#4650 = DIRECTION ( 'NONE',  ( 0.000000000000000000, 0.000000000000000000, -1.000000000000000000 ) ) ;
#4651 = CYLINDRICAL_SURFACE ( 'NONE', #16230, 1.500000000000001332 ) ;
#4652 = DIRECTION ( 'NONE',  ( 0.000000000000000000, 0.000000000000000000, -1.000000000000000000 ) ) ;
#4653 = TOROIDAL_SURFACE ( 'NONE', #8334, 17.50000000000000000, 1.499999999999998668 ) ;
#4654 = CARTESIAN_POINT ( 'NONE',  ( 33.72499318558949710, 26.59184655352419568, 47.04930799450051637 ) ) ;
#4655 = CARTESIAN_POINT ( 'NONE',  ( 45.86052195822112765, 29.24126980604143355, 44.96013611432259438 ) ) ;
#4656 = ORIENTED_EDGE ( 'NONE', *, *, #26627, .F. ) ;
#4657 = ORIENTED_EDGE ( 'NONE', *, *, #31935, .F. ) ;
#4658 = ADVANCED_FACE ( 'NONE', ( #14536 ), #4680, .T. ) ;
#4659 = CARTESIAN_POINT ( 'NONE',  ( -41.91739890389096956, 13.90674392281399818, 54.59993297551692848 ) ) ;
#4660 = VECTOR ( 'NONE', #4915, 1000.000000000000000 ) ;
#4661 = AXIS2_PLACEMENT_3D ( 'NONE', #16707, #4251, #5184 ) ;
#4662 = ORIENTED_EDGE ( 'NONE', *, *, #28051, .F. ) ;
#4663 = CIRCLE ( 'NONE', #465, 0.1250000000000001110 ) ;
#4664 =( BOUNDED_CURVE ( )  B_SPLINE_CURVE ( 3, ( #22093, #6681, #32124, #3894 ),
 .UNSPECIFIED., .F., .F. ) 
 B_SPLINE_CURVE_WITH_KNOTS ( ( 4, 4 ),
 ( 5.062864179022701805, 5.184122060454623870 ),
 .UNSPECIFIED. ) 
 CURVE ( )  GEOMETRIC_REPRESENTATION_ITEM ( )  RATIONAL_B_SPLINE_CURVE ( ( 1.000000000000000000, 0.9987750858034806223, 0.9987750858034806223, 1.000000000000000000 ) ) 
 REPRESENTATION_ITEM ( '' )  );
#4665 = DIRECTION ( 'NONE',  ( -1.101824276508909887E-16, 1.000000000000000000, -0.000000000000000000 ) ) ;
#4666 = FACE_OUTER_BOUND ( 'NONE', #790, .T. ) ;
#4667 = EDGE_CURVE ( 'NONE', #13719, #306, #1728, .T. ) ;
#4668 = ORIENTED_EDGE ( 'NONE', *, *, #7760, .T. ) ;
#4669 = AXIS2_PLACEMENT_3D ( 'NONE', #30855, #25761, #12820 ) ;
#4670 = LINE ( 'NONE', #2531, #6566 ) ;
#4671 = ORIENTED_EDGE ( 'NONE', *, *, #28166, .T. ) ;
#4672 = DIRECTION ( 'NONE',  ( 0.8746197071393960742, -0.4848096202463368365, -1.277302113040707570E-17 ) ) ;
#4673 = CYLINDRICAL_SURFACE ( 'NONE', #16827, 12.36707279061065101 ) ;
#4674 = LINE ( 'NONE', #24528, #4455 ) ;
#4675 = EDGE_LOOP ( 'NONE', ( #7524, #2544, #13091, #3923 ) ) ;
#4676 = DIRECTION ( 'NONE',  ( -1.101824276508909887E-16, 1.000000000000000000, -0.000000000000000000 ) ) ;
#4677 = CARTESIAN_POINT ( 'NONE',  ( 42.59785597605720397, -5.098646251524523443, 47.04930799450052348 ) ) ;
#4678 = DIRECTION ( 'NONE',  ( -1.101824276508909887E-16, 1.000000000000000000, -0.000000000000000000 ) ) ;
#4679 = FACE_OUTER_BOUND ( 'NONE', #13222, .T. ) ;
#4680 = CYLINDRICAL_SURFACE ( 'NONE', #21518, 12.62506659569710443 ) ;
#4681 = DIRECTION ( 'NONE',  ( 0.000000000000000000, 0.000000000000000000, -1.000000000000000000 ) ) ;
#4682 = VERTEX_POINT ( 'NONE', #21743 ) ;
#4683 = FACE_OUTER_BOUND ( 'NONE', #31207, .T. ) ;
#4684 = DIRECTION ( 'NONE',  ( -1.101824276508909887E-16, 1.000000000000000000, -0.000000000000000000 ) ) ;
#4685 = ORIENTED_EDGE ( 'NONE', *, *, #6793, .T. ) ;
#4686 = B_SPLINE_CURVE_WITH_KNOTS ( 'NONE', 3,
 ( #3994, #6463, #16462, #11546, #26481, #22030, #20068, #30096 ),
 .UNSPECIFIED., .F., .F.,
 ( 4, 2, 2, 4 ),
 ( 0.000000000000000000, 0.0002558676349343736952, 0.0005117352698687473904, 0.001023470539737489360 ),
 .UNSPECIFIED. ) ;
#4687 = CARTESIAN_POINT ( 'NONE',  ( -45.22799897120231094, -5.771451657996960805, 53.24836847294543674 ) ) ;
#4688 = B_SPLINE_CURVE_WITH_KNOTS ( 'NONE', 3,
 ( #26148, #28465, #3498, #1045, #11071, #11376, #21367, #21054, #32223, #24169, #22024, #2181, #6775, #2011, #9241, #27121, #12027, #26956, #16777 ),
 .UNSPECIFIED., .F., .F.,
 ( 4, 3, 3, 3, 3, 3, 4 ),
 ( -2.006352434653661683E-06, 0.000000000000000000, 4.188863878082995122E-05, 9.359854324831489748E-05, 0.0001315996560788412501, 0.0001581967873567794803, 0.0001850264499128575937 ),
 .UNSPECIFIED. ) ;
#4689 = AXIS2_PLACEMENT_3D ( 'NONE', #29465, #23720, #3861 ) ;
#4690 = CIRCLE ( 'NONE', #10465, 0.1999999999999987899 ) ;
#4691 = DIRECTION ( 'NONE',  ( -1.000000000000000000, -1.101824276508909887E-16, 0.000000000000000000 ) ) ;
#4692 = ORIENTED_EDGE ( 'NONE', *, *, #25803, .F. ) ;
#4693 = ORIENTED_EDGE ( 'NONE', *, *, #6115, .F. ) ;
#4694 = AXIS2_PLACEMENT_3D ( 'NONE', #14139, #23974, #23810 ) ;
#4695 = CIRCLE ( 'NONE', #3639, 0.1250000000000001110 ) ;
#4696 = EDGE_LOOP ( 'NONE', ( #9349, #18022, #11086, #8 ) ) ;
#4697 = VECTOR ( 'NONE', #27385, 1000.000000000000000 ) ;
#4698 = CONICAL_SURFACE ( 'NONE', #16239, 20.38082872909741994, 1.021642509542357802 ) ;
#4699 = FACE_OUTER_BOUND ( 'NONE', #20142, .T. ) ;
#4700 = AXIS2_PLACEMENT_3D ( 'NONE', #21734, #16812, #14367 ) ;
#4701 = EDGE_CURVE ( 'NONE', #6259, #6661, #5339, .T. ) ;
#4702 = ORIENTED_EDGE ( 'NONE', *, *, #17456, .F. ) ;
#4703 = ORIENTED_EDGE ( 'NONE', *, *, #31720, .T. ) ;
#4704 = DIRECTION ( 'NONE',  ( -1.000000000000000000, -1.101824276508910010E-16, 0.000000000000000000 ) ) ;
#4705 = EDGE_CURVE ( 'NONE', #29664, #27773, #15343, .T. ) ;
#4706 = EDGE_CURVE ( 'NONE', #26371, #23543, #30768, .T. ) ;
#4707 = CARTESIAN_POINT ( 'NONE',  ( -44.29239190677800053, -5.820133356959887649, 53.36605615429809291 ) ) ;
#4708 = EDGE_CURVE ( 'NONE', #2312, #665, #10886, .T. ) ;
#4709 = CARTESIAN_POINT ( 'NONE',  ( 21.09992658989239089, 25.34184655352419213, 47.04930799450051637 ) ) ;
#4710 = FACE_OUTER_BOUND ( 'NONE', #28962, .T. ) ;
#4711 = DIRECTION ( 'NONE',  ( -1.000000000000000000, 0.000000000000000000, 0.000000000000000000 ) ) ;
#4712 = ORIENTED_EDGE ( 'NONE', *, *, #3629, .T. ) ;
#4713 = CARTESIAN_POINT ( 'NONE',  ( -6.914515305352443519, 8.508769500014659926, 97.55334879272453463 ) ) ;
#4714 = ORIENTED_EDGE ( 'NONE', *, *, #21959, .T. ) ;
#4715 = CARTESIAN_POINT ( 'NONE',  ( -35.39862181984237566, -4.229295130874948683, 13.68382211909319146 ) ) ;
#4716 = CARTESIAN_POINT ( 'NONE',  ( 33.72499318558949000, 38.56284415653841791, 47.04930799450051637 ) ) ;
#4717 = ORIENTED_EDGE ( 'NONE', *, *, #18469, .T. ) ;
#4718 = CARTESIAN_POINT ( 'NONE',  ( -40.73091736380679606, 9.483895492497154578, 34.64930799450051779 ) ) ;
#4719 = DIRECTION ( 'NONE',  ( -0.4848096202463424986, -0.8746197071393928546, 2.220446049250312834E-16 ) ) ;
#4720 = CIRCLE ( 'NONE', #31460, 0.1250000000000001110 ) ;
#4721 = CARTESIAN_POINT ( 'NONE',  ( 52.20930123405432965, -5.935454061169745721, 107.5404866792554799 ) ) ;
#4722 = CARTESIAN_POINT ( 'NONE',  ( 21.09785597605719332, 15.06454579224778456, 47.04930799450051637 ) ) ;
#4723 = CARTESIAN_POINT ( 'NONE',  ( 48.14727188781975542, 19.96454579224779380, 49.10650501410607660 ) ) ;
#4724 = CARTESIAN_POINT ( 'NONE',  ( 44.70507715278255745, 26.26291119454915801, 46.92503878583765697 ) ) ;
#4725 = AXIS2_PLACEMENT_3D ( 'NONE', #74, #2698, #12728 ) ;
#4726 = DIRECTION ( 'NONE',  ( 0.2756373558169954441, -0.9612616959383198934, 1.479773560108263204E-16 ) ) ;
#4727 = DIRECTION ( 'NONE',  ( 0.000000000000000000, 1.000000000000000000, -0.000000000000000000 ) ) ;
#4728 = ORIENTED_EDGE ( 'NONE', *, *, #26650, .F. ) ;
#4729 = DIRECTION ( 'NONE',  ( -0.000000000000000000, -1.000000000000000000, -1.446921688628131436E-16 ) ) ;
#4730 = AXIS2_PLACEMENT_3D ( 'NONE', #530, #10563, #18237 ) ;
#4731 = LINE ( 'NONE', #12287, #19788 ) ;
#4732 = VERTEX_POINT ( 'NONE', #5497 ) ;
#4733 = DIRECTION ( 'NONE',  ( -1.000000000000000000, -1.101824276508909887E-16, 0.000000000000000000 ) ) ;
#4734 = DIRECTION ( 'NONE',  ( -0.000000000000000000, -1.000000000000000000, 0.000000000000000000 ) ) ;
#4735 = ORIENTED_EDGE ( 'NONE', *, *, #8766, .T. ) ;
#4736 = VERTEX_POINT ( 'NONE', #2864 ) ;
#4737 = CARTESIAN_POINT ( 'NONE',  ( 33.46699938050304013, 27.71183152705960850, 47.04930799450051637 ) ) ;
#4738 = VECTOR ( 'NONE', #4309, 1000.000000000000000 ) ;
#4739 = ORIENTED_EDGE ( 'NONE', *, *, #6896, .F. ) ;
#4740 = ADVANCED_FACE ( 'NONE', ( #12898 ), #29218, .F. ) ;
#4741 = VECTOR ( 'NONE', #27861, 1000.000000000000000 ) ;
#4742 = AXIS2_PLACEMENT_3D ( 'NONE', #4087, #24114, #1631 ) ;
#4743 = VECTOR ( 'NONE', #7223, 1000.000000000000000 ) ;
#4744 = VERTEX_POINT ( 'NONE', #563 ) ;
#4745 = CARTESIAN_POINT ( 'NONE',  ( 46.20089404322238380, 22.99884124225578574, 48.14463855678482673 ) ) ;
#4746 = CIRCLE ( 'NONE', #10525, 1.000000000000000888 ) ;
#4747 = DIRECTION ( 'NONE',  ( -0.000000000000000000, -0.000000000000000000, -1.000000000000000000 ) ) ;
#4748 = VECTOR ( 'NONE', #18074, 999.9999999999998863 ) ;
#4749 = ORIENTED_EDGE ( 'NONE', *, *, #4945, .F. ) ;
#4750 = EDGE_CURVE ( 'NONE', #24189, #5504, #25029, .T. ) ;
#4751 = EDGE_CURVE ( 'NONE', #23541, #10568, #12996, .T. ) ;
#4752 = CARTESIAN_POINT ( 'NONE',  ( 33.46699938050304013, 28.21183152705961206, 47.04930799450051637 ) ) ;
#4753 = EDGE_CURVE ( 'NONE', #3840, #27647, #3020, .T. ) ;
#4754 = CARTESIAN_POINT ( 'NONE',  ( 49.23437818303271030, 22.84434098701873594, 46.83627993336631334 ) ) ;
#4755 = EDGE_CURVE ( 'NONE', #30294, #9364, #30129, .T. ) ;
#4756 = CARTESIAN_POINT ( 'NONE',  ( 45.28286642839709231, 29.84289516297709710, 47.97516931882780966 ) ) ;
#4757 = ORIENTED_EDGE ( 'NONE', *, *, #1245, .F. ) ;
#4758 = EDGE_CURVE ( 'NONE', #22576, #22420, #2487, .T. ) ;
#4759 = ORIENTED_EDGE ( 'NONE', *, *, #16209, .F. ) ;
#4760 = TOROIDAL_SURFACE ( 'NONE', #10014, 58.86319174311611846, 0.1999999999999984290 ) ;
#4761 = EDGE_LOOP ( 'NONE', ( #18620, #18777, #13731, #18965, #20198 ) ) ;
#4762 = DIRECTION ( 'NONE',  ( -0.000000000000000000, -1.000000000000000000, 0.000000000000000000 ) ) ;
#4763 = CARTESIAN_POINT ( 'NONE',  ( -63.90214402394282445, -5.935454207752202116, 16.07118271501078510 ) ) ;
#4764 = DIRECTION ( 'NONE',  ( -1.101824276508909887E-16, 1.000000000000000000, -0.000000000000000000 ) ) ;
#4765 = DIRECTION ( 'NONE',  ( 0.000000000000000000, 0.000000000000000000, -1.000000000000000000 ) ) ;
#4766 = CARTESIAN_POINT ( 'NONE',  ( 48.83862994770795041, 25.85457786121582302, 48.17861352429476085 ) ) ;
#4767 = SHAPE_DEFINITION_REPRESENTATION ( #32111, #14743 ) ;
#4768 = VERTEX_POINT ( 'NONE', #10425 ) ;
#4769 = ORIENTED_EDGE ( 'NONE', *, *, #26658, .T. ) ;
#4770 = DIRECTION ( 'NONE',  ( 0.000000000000000000, 0.000000000000000000, -1.000000000000000000 ) ) ;
#4771 = CARTESIAN_POINT ( 'NONE',  ( -41.34584395867850048, 11.59800658573647425, 56.14611646155296398 ) ) ;
#4772 = DIRECTION ( 'NONE',  ( -1.101824276508909887E-16, 1.000000000000000000, -0.000000000000000000 ) ) ;
#4773 = ORIENTED_EDGE ( 'NONE', *, *, #8534, .T. ) ;
#4774 = DIRECTION ( 'NONE',  ( -1.000000000000000000, 0.000000000000000000, 0.000000000000000000 ) ) ;
#4775 = LINE ( 'NONE', #14624, #5236 ) ;
#4776 = ORIENTED_EDGE ( 'NONE', *, *, #24228, .F. ) ;
#4777 = DIRECTION ( 'NONE',  ( -0.000000000000000000, -1.000000000000000000, 0.000000000000000000 ) ) ;
#4778 = CIRCLE ( 'NONE', #23111, 0.5000000000000004441 ) ;
#4779 = FACE_OUTER_BOUND ( 'NONE', #20181, .T. ) ;
#4780 = VECTOR ( 'NONE', #13694, 1000.000000000000000 ) ;
#4781 = DIRECTION ( 'NONE',  ( -1.000000000000000000, 0.000000000000000000, 0.000000000000000000 ) ) ;
#4782 = EDGE_CURVE ( 'NONE', #26186, #10938, #18199, .T. ) ;
#4783 = EDGE_CURVE ( 'NONE', #1392, #31159, #8778, .T. ) ;
#4784 = VERTEX_POINT ( 'NONE', #25514 ) ;
#4785 = ORIENTED_EDGE ( 'NONE', *, *, #1993, .T. ) ;
#4786 = DIRECTION ( 'NONE',  ( -1.101824276508909887E-16, 1.000000000000000000, -0.000000000000000000 ) ) ;
#4787 = CARTESIAN_POINT ( 'NONE',  ( 48.18662509608405031, 25.88284706826093284, 49.18364984542562013 ) ) ;
#4788 = ORIENTED_EDGE ( 'NONE', *, *, #16837, .F. ) ;
#4789 = CIRCLE ( 'NONE', #31529, 27.49999999999999645 ) ;
#4790 = DIRECTION ( 'NONE',  ( -1.101824276508909887E-16, 1.000000000000000000, -0.000000000000000000 ) ) ;
#4791 = CARTESIAN_POINT ( 'NONE',  ( 48.23388202445966755, 27.52822092656774089, 49.27628909396054979 ) ) ;
#4792 = CONICAL_SURFACE ( 'NONE', #91, 0.9999999999999731326, 0.4537856055185219284 ) ;
#4793 = EDGE_CURVE ( 'NONE', #22254, #231, #2706, .T. ) ;
#4794 = CYLINDRICAL_SURFACE ( 'NONE', #22047, 16.99999999999999289 ) ;
#4795 = CIRCLE ( 'NONE', #23143, 12.36707279061065101 ) ;
#4796 = DIRECTION ( 'NONE',  ( 0.3428121700606596156, 0.6184495258776486759, 0.7071067811865566766 ) ) ;
#4797 = CARTESIAN_POINT ( 'NONE',  ( -25.19641122222149576, -13.74047052604243646, 82.56529288175448755 ) ) ;
#4798 = CARTESIAN_POINT ( 'NONE',  ( -41.50472230201275181, 5.945882615091417911, 37.04930799450052348 ) ) ;
#4799 = CARTESIAN_POINT ( 'NONE',  ( -58.11219453028166981, -16.63545420775219696, 47.04930799450023926 ) ) ;
#4800 = CARTESIAN_POINT ( 'NONE',  ( 8.732853799281732776, 31.47145308207317171, 47.04930799450051637 ) ) ;
#4801 =( NAMED_UNIT ( * ) SI_UNIT ( $, .STERADIAN. ) SOLID_ANGLE_UNIT ( ) );
#4802 = VERTEX_POINT ( 'NONE', #15026 ) ;
#4803 = EDGE_LOOP ( 'NONE', ( #31160, #20007, #3642, #29614 ) ) ;
#4804 = DIRECTION ( 'NONE',  ( -1.000000000000000000, 0.000000000000000000, 0.000000000000000000 ) ) ;
#4805 = CIRCLE ( 'NONE', #7441, 28.00000000000000000 ) ;
#4806 = CARTESIAN_POINT ( 'NONE',  ( 21.09785597605807439, -5.935454207752083988, 47.04930799450051637 ) ) ;
#4807 = DIRECTION ( 'NONE',  ( -0.4848096202463408888, -0.8746197071393936318, 0.000000000000000000 ) ) ;
#4808 = CARTESIAN_POINT ( 'NONE',  ( 8.823509210239553369, 28.59164230456639544, 47.04930799450051637 ) ) ;
#4809 = ORIENTED_EDGE ( 'NONE', *, *, #19977, .T. ) ;
#4810 = CARTESIAN_POINT ( 'NONE',  ( 9.016997203727585841, 15.24673779880127356, 47.36565641480107303 ) ) ;
#4811 = CARTESIAN_POINT ( 'NONE',  ( -41.02687597405218156, 7.220473278338834788, 60.44930799450051495 ) ) ;
#4812 = DIRECTION ( 'NONE',  ( -1.101824276508909887E-16, 1.000000000000000000, -0.000000000000000000 ) ) ;
#4813 = EDGE_CURVE ( 'NONE', #31727, #31154, #12566, .T. ) ;
#4814 = EDGE_LOOP ( 'NONE', ( #11083, #7217, #16094, #23055 ) ) ;
#4815 = ORIENTED_EDGE ( 'NONE', *, *, #5946, .T. ) ;
#4816 = CARTESIAN_POINT ( 'NONE',  ( -40.28779227465695101, 2.984619150196775816, 37.04930799450052348 ) ) ;
#4817 = CARTESIAN_POINT ( 'NONE',  ( 47.20547626766766314, 28.97451373492759430, 44.97710074790751378 ) ) ;
#4818 = DIRECTION ( 'NONE',  ( 0.4848096202463636484, 0.8746197071393810862, 0.000000000000000000 ) ) ;
#4819 = EDGE_CURVE ( 'NONE', #31739, #10736, #17798, .T. ) ;
#4820 = CARTESIAN_POINT ( 'NONE',  ( 33.71785032049129427, 32.21664230456639899, 47.04930799450051637 ) ) ;
#4821 = AXIS2_PLACEMENT_3D ( 'NONE', #19444, #24370, #21740 ) ;
#4822 = CARTESIAN_POINT ( 'NONE',  ( 71.88545709212758084, 11.18855628041951711, 22.82477309973399926 ) ) ;
#4823 = TOROIDAL_SURFACE ( 'NONE', #31551, 12.40141737965288904, 0.1249999999999998612 ) ;
#4824 = ORIENTED_EDGE ( 'NONE', *, *, #6569, .F. ) ;
#4825 = ADVANCED_FACE ( 'NONE', ( #27652 ), #23960, .T. ) ;
#4826 = EDGE_CURVE ( 'NONE', #24828, #21830, #20418, .T. ) ;
#4827 = VERTEX_POINT ( 'NONE', #27822 ) ;
#4828 = EDGE_CURVE ( 'NONE', #22606, #27738, #6162, .T. ) ;
#4829 = CARTESIAN_POINT ( 'NONE',  ( -40.80097511801616150, 8.246641009394465982, 59.44930799450051495 ) ) ;
#4830 = AXIS2_PLACEMENT_3D ( 'NONE', #9608, #24371, #19604 ) ;
#4831 = ORIENTED_EDGE ( 'NONE', *, *, #21249, .T. ) ;
#4832 = AXIS2_PLACEMENT_3D ( 'NONE', #26622, #4138, #14162 ) ;
#4833 = CARTESIAN_POINT ( 'NONE',  ( 21.09785597605720753, 13.86454579224779948, 47.04930799450052348 ) ) ;
#4834 = CYLINDRICAL_SURFACE ( 'NONE', #942, 12.62506659569710266 ) ;
#4835 = ADVANCED_FACE ( 'NONE', ( #3499 ), #6131, .F. ) ;
#4836 = VECTOR ( 'NONE', #11983, 1000.000000000000114 ) ;
#4837 = ORIENTED_EDGE ( 'NONE', *, *, #26462, .F. ) ;
#4838 = CARTESIAN_POINT ( 'NONE',  ( -40.57832940339291383, 7.446916344587776848, 60.29072935073781991 ) ) ;
#4839 = ORIENTED_EDGE ( 'NONE', *, *, #4133, .F. ) ;
#4840 = LINE ( 'NONE', #27973, #2 ) ;
#4841 = VECTOR ( 'NONE', #17031, 1000.000000000000000 ) ;
#4842 = DIRECTION ( 'NONE',  ( -0.4848096202463450521, -0.8746197071393914113, 0.000000000000000000 ) ) ;
#4843 = DIRECTION ( 'NONE',  ( -0.000000000000000000, -1.000000000000000000, 0.000000000000000000 ) ) ;
#4844 = EDGE_LOOP ( 'NONE', ( #1144, #4483, #18182, #31824 ) ) ;
#4845 = DIRECTION ( 'NONE',  ( -1.000000000000000000, 0.000000000000000000, 0.000000000000000000 ) ) ;
#4846 = DIRECTION ( 'NONE',  ( -0.000000000000000000, -1.000000000000000000, 0.000000000000000000 ) ) ;
#4847 = DIRECTION ( 'NONE',  ( -1.224646799147353207E-16, -1.349345573449484691E-32, 1.000000000000000000 ) ) ;
#4848 = PLANE ( 'NONE',  #4304 ) ;
#4849 = CARTESIAN_POINT ( 'NONE',  ( 48.14727188781975542, 22.86454579224779948, 49.10650501410607660 ) ) ;
#4850 = FACE_OUTER_BOUND ( 'NONE', #7607, .T. ) ;
#4851 = VERTEX_POINT ( 'NONE', #21535 ) ;
#4852 = CARTESIAN_POINT ( 'NONE',  ( 21.09785597605719332, 6.717634499306958773, 47.04930799450051637 ) ) ;
#4853 = FACE_OUTER_BOUND ( 'NONE', #31799, .T. ) ;
#4854 = EDGE_CURVE ( 'NONE', #17679, #5749, #7222, .T. ) ;
#4855 = VERTEX_POINT ( 'NONE', #3828 ) ;
#4856 = CARTESIAN_POINT ( 'NONE',  ( -0.9021440239427926944, -5.098646251524523443, 47.04930799450052348 ) ) ;
#4857 = ADVANCED_FACE ( 'NONE', ( #16457 ), #19772, .T. ) ;
#4858 = CARTESIAN_POINT ( 'NONE',  ( 21.09785597605720042, -16.03545420775219910, -17.45069200549948718 ) ) ;
#4859 = AXIS2_PLACEMENT_3D ( 'NONE', #21490, #1642, #11665 ) ;
#4860 = ORIENTED_EDGE ( 'NONE', *, *, #29020, .F. ) ;
#4861 = EDGE_LOOP ( 'NONE', ( #13996, #17729, #2702, #12207 ) ) ;
#4862 = AXIS2_PLACEMENT_3D ( 'NONE', #15773, #503, #23324 ) ;
#4863 = ADVANCED_FACE ( 'NONE', ( #15982 ), #1966, .T. ) ;
#4864 = AXIS2_PLACEMENT_3D ( 'NONE', #766, #23727, #1233 ) ;
#4865 = EDGE_LOOP ( 'NONE', ( #26649, #31897, #11347, #7235 ) ) ;
#4866 = ADVANCED_FACE ( 'NONE', ( #18912 ), #23462, .T. ) ;
#4867 = AXIS2_PLACEMENT_3D ( 'NONE', #16348, #26363, #13428 ) ;
#4868 =( BOUNDED_CURVE ( )  B_SPLINE_CURVE ( 3, ( #31263, #28789, #16145, #21548 ),
 .UNSPECIFIED., .F., .F. ) 
 B_SPLINE_CURVE_WITH_KNOTS ( ( 4, 4 ),
 ( 5.062864179022703581, 5.184122060454621206 ),
 .UNSPECIFIED. ) 
 CURVE ( )  GEOMETRIC_REPRESENTATION_ITEM ( )  RATIONAL_B_SPLINE_CURVE ( ( 1.000000000000000000, 0.9987750858034806223, 0.9987750858034806223, 1.000000000000000000 ) ) 
 REPRESENTATION_ITEM ( '' )  );
#4869 = DIRECTION ( 'NONE',  ( -1.101824276508909887E-16, 1.000000000000000000, -0.000000000000000000 ) ) ;
#4870 = ORIENTED_EDGE ( 'NONE', *, *, #531, .T. ) ;
#4871 = ORIENTED_EDGE ( 'NONE', *, *, #3988, .F. ) ;
#4872 = CARTESIAN_POINT ( 'NONE',  ( 81.56333945993378620, -5.935454207834600204, 15.93786612339379083 ) ) ;
#4873 = CIRCLE ( 'NONE', #31611, 0.1000000000000011297 ) ;
#4874 = CARTESIAN_POINT ( 'NONE',  ( 47.34122803410652836, 10.07216359114295479, -4.322712525059973387 ) ) ;
#4875 = CARTESIAN_POINT ( 'NONE',  ( 21.09785597605719332, 38.31023907818019580, 47.04930799450051637 ) ) ;
#4876 = DIRECTION ( 'NONE',  ( 0.000000000000000000, -1.000000000000000000, 0.000000000000000000 ) ) ;
#4877 = AXIS2_PLACEMENT_3D ( 'NONE', #15051, #5199, #22587 ) ;
#4878 = DIRECTION ( 'NONE',  ( -1.101824276508909887E-16, 1.000000000000000000, -0.000000000000000000 ) ) ;
#4879 = ORIENTED_EDGE ( 'NONE', *, *, #27843, .T. ) ;
#4880 = DIRECTION ( 'NONE',  ( -0.000000000000000000, -1.000000000000000000, -0.000000000000000000 ) ) ;
#4881 = ORIENTED_EDGE ( 'NONE', *, *, #10420, .T. ) ;
#4882 = EDGE_CURVE ( 'NONE', #31146, #14944, #16628, .T. ) ;
#4883 = DIRECTION ( 'NONE',  ( -1.000000000000000000, 0.000000000000000000, 0.000000000000000000 ) ) ;
#4884 = DIRECTION ( 'NONE',  ( 0.000000000000000000, -0.000000000000000000, -1.000000000000000000 ) ) ;
#4885 = ORIENTED_EDGE ( 'NONE', *, *, #27048, .F. ) ;
#4886 = FACE_OUTER_BOUND ( 'NONE', #8031, .T. ) ;
#4887 = CARTESIAN_POINT ( 'NONE',  ( 52.15090187871769700, -5.936918531481693684, 107.6665413424431961 ) ) ;
#4888 = DIRECTION ( 'NONE',  ( -1.000000000000000000, 0.000000000000000000, 0.000000000000000000 ) ) ;
#4889 = CARTESIAN_POINT ( 'NONE',  ( 8.474859994195282908, 38.56284415653841791, 47.04930799450051637 ) ) ;
#4890 = CARTESIAN_POINT ( 'NONE',  ( 48.94625023931840246, 28.07124452788248803, 46.10640627770150246 ) ) ;
#4891 = CIRCLE ( 'NONE', #23231, 0.1250000000000001110 ) ;
#4892 = CIRCLE ( 'NONE', #13289, 12.62506659569710266 ) ;
#4893 = CARTESIAN_POINT ( 'NONE',  ( 21.09785597605719687, 45.28940914544685370, 24.35070776595075515 ) ) ;
#4894 = CARTESIAN_POINT ( 'NONE',  ( -36.45222641229887017, 9.925589859889722533, 42.04930799450051637 ) ) ;
#4895 = ORIENTED_EDGE ( 'NONE', *, *, #27999, .T. ) ;
#4896 = CARTESIAN_POINT ( 'NONE',  ( 47.12654256966948907, 29.60334677283180582, 44.98830670686451327 ) ) ;
#4897 = LINE ( 'NONE', #2589, #26094 ) ;
#4898 = ORIENTED_EDGE ( 'NONE', *, *, #23574, .T. ) ;
#4899 = DIRECTION ( 'NONE',  ( -0.000000000000000000, -1.000000000000000000, -0.000000000000000000 ) ) ;
#4900 = ORIENTED_EDGE ( 'NONE', *, *, #11198, .T. ) ;
#4901 = VERTEX_POINT ( 'NONE', #11542 ) ;
#4902 = FACE_OUTER_BOUND ( 'NONE', #11593, .T. ) ;
#4903 = EDGE_CURVE ( 'NONE', #31649, #30197, #8599, .T. ) ;
#4904 = ORIENTED_EDGE ( 'NONE', *, *, #7124, .T. ) ;
#4905 = EDGE_CURVE ( 'NONE', #20809, #32483, #26149, .T. ) ;
#4906 = CIRCLE ( 'NONE', #32155, 20.38082872909741994 ) ;
#4907 = AXIS2_PLACEMENT_3D ( 'NONE', #25518, #10911, #567 ) ;
#4908 = VECTOR ( 'NONE', #16206, 1000.000000000000114 ) ;
#4909 = AXIS2_PLACEMENT_3D ( 'NONE', #8571, #3640, #1018 ) ;
#4910 = VECTOR ( 'NONE', #6339, 1000.000000000000000 ) ;
#4911 = EDGE_LOOP ( 'NONE', ( #8926, #30976, #16052, #8516 ) ) ;
#4912 = CARTESIAN_POINT ( 'NONE',  ( -4.902144023942810236, 25.56454579224779877, 44.54930799450078638 ) ) ;
#4913 = CARTESIAN_POINT ( 'NONE',  ( 51.67049335409638644, 5.388785998227653806, -12.70392589783158499 ) ) ;
#4914 = ORIENTED_EDGE ( 'NONE', *, *, #28935, .F. ) ;
#4915 = DIRECTION ( 'NONE',  ( -1.101824276508909887E-16, 1.000000000000000000, -0.000000000000000000 ) ) ;
#4916 = CARTESIAN_POINT ( 'NONE',  ( 0.6836613156275018754, 1.925589859889728972, -37.95069200549950494 ) ) ;
#4917 = CARTESIAN_POINT ( 'NONE',  ( 48.83059987400640978, 26.28213139976340784, 48.97189179988551899 ) ) ;
#4918 = CARTESIAN_POINT ( 'NONE',  ( 46.99218062947583974, 29.25956182964375429, 49.08406571254116102 ) ) ;
#4919 = ORIENTED_EDGE ( 'NONE', *, *, #29680, .F. ) ;
#4920 = VERTEX_POINT ( 'NONE', #26316 ) ;
#4921 = DIRECTION ( 'NONE',  ( 0.000000000000000000, -1.000000000000000000, -0.000000000000000000 ) ) ;
#4922 = VERTEX_POINT ( 'NONE', #3667 ) ;
#4923 = DIRECTION ( 'NONE',  ( -1.000000000000000000, -1.101824276508909887E-16, 0.000000000000000000 ) ) ;
#4924 = DIRECTION ( 'NONE',  ( -1.101824276508909887E-16, 1.000000000000000000, -0.000000000000000000 ) ) ;
#4925 = CARTESIAN_POINT ( 'NONE',  ( -40.68765130478461600, 6.801118111650039211, 34.74701532369150669 ) ) ;
#4926 = CIRCLE ( 'NONE', #20118, 31.50000000000000711 ) ;
#4927 = CARTESIAN_POINT ( 'NONE',  ( -40.06561427811386267, 7.496110634155836117, 58.05249952744806308 ) ) ;
#4928 = CARTESIAN_POINT ( 'NONE',  ( 45.79384627280941800, 25.67957786121582231, 49.05938063676250493 ) ) ;
#4929 = APPLICATION_PROTOCOL_DEFINITION ( 'draft international standard', 'automotive_design', 1998, #9095 ) ;
#4930 = ORIENTED_EDGE ( 'NONE', *, *, #21642, .F. ) ;
#4931 = ORIENTED_EDGE ( 'NONE', *, *, #31027, .T. ) ;
#4932 = CARTESIAN_POINT ( 'NONE',  ( -42.47434154250544225, 4.196643200812637531, 55.14930799450051779 ) ) ;
#4933 = DIRECTION ( 'NONE',  ( 0.5849755626391567320, -0.8110509177080079679, 0.000000000000000000 ) ) ;
#4934 = CIRCLE ( 'NONE', #23277, 0.8928932188134552916 ) ;
#4935 = CARTESIAN_POINT ( 'NONE',  ( 21.09992658989239089, 23.71664230456639899, 47.04930799450051637 ) ) ;
#4936 = ORIENTED_EDGE ( 'NONE', *, *, #1108, .F. ) ;
#4937 = CARTESIAN_POINT ( 'NONE',  ( 49.49063479933183629, 29.49951373492759288, 47.17357720316391578 ) ) ;
#4938 = EDGE_LOOP ( 'NONE', ( #4980, #27231, #29317, #19712 ) ) ;
#4939 = CARTESIAN_POINT ( 'NONE',  ( -42.36691375901575185, 13.72999064396537250, 59.48380644099231773 ) ) ;
#4940 = DIRECTION ( 'NONE',  ( 0.000000000000000000, 0.000000000000000000, -1.000000000000000000 ) ) ;
#4941 = DIRECTION ( 'NONE',  ( -1.000000000000000000, -1.101824276508909887E-16, 0.000000000000000000 ) ) ;
#4942 = EDGE_CURVE ( 'NONE', #5204, #25724, #7200, .T. ) ;
#4943 = ADVANCED_FACE ( 'NONE', ( #25831 ), #11377, .F. ) ;
#4944 = EDGE_CURVE ( 'NONE', #27481, #15810, #4045, .T. ) ;
#4945 = EDGE_CURVE ( 'NONE', #3387, #10137, #28068, .T. ) ;
#4946 = ORIENTED_EDGE ( 'NONE', *, *, #9416, .T. ) ;
#4947 = CIRCLE ( 'NONE', #23792, 0.1000000000000014905 ) ;
#4948 = ORIENTED_EDGE ( 'NONE', *, *, #23276, .F. ) ;
#4949 = TOROIDAL_SURFACE ( 'NONE', #3911, 56.00000000000000000, 1.000000000000000000 ) ;
#4950 = CARTESIAN_POINT ( 'NONE',  ( -43.37834615508418068, 1.121909970995876193, 34.64930799450052490 ) ) ;
#4951 = CARTESIAN_POINT ( 'NONE',  ( 72.46310410352278097, 9.702389020015065313, 73.75010705023584023 ) ) ;
#4953 = CARTESIAN_POINT ( 'NONE',  ( 47.22751897799751220, 27.94253733014356200, 44.55267275764142454 ) ) ;
#4952 = AXIS2_PLACEMENT_3D ( 'NONE', #18542, #3126, #8233 ) ;
#4954 = AXIS2_PLACEMENT_3D ( 'NONE', #23470, #18207, #23315 ) ;
#4955 = ORIENTED_EDGE ( 'NONE', *, *, #15318, .T. ) ;
#4956 = DIRECTION ( 'NONE',  ( 0.8746197071393926326, -0.4848096202463430537, -8.676864087101709653E-18 ) ) ;
#4957 = CARTESIAN_POINT ( 'NONE',  ( -42.48178708409979265, 14.60617548783703690, 55.10133939125226021 ) ) ;
#4958 = DIRECTION ( 'NONE',  ( 0.000000000000000000, -0.000000000000000000, -1.000000000000000000 ) ) ;
#4959 = DIRECTION ( 'NONE',  ( -0.9986540920324801229, -1.233316085972235080E-16, -0.05186525298099629866 ) ) ;
#4960 = DIRECTION ( 'NONE',  ( 0.000000000000000000, 0.000000000000000000, -1.000000000000000000 ) ) ;
#4961 = DIRECTION ( 'NONE',  ( 0.000000000000000000, -1.000000000000000000, 0.000000000000000000 ) ) ;
#4962 = DIRECTION ( 'NONE',  ( -0.000000000000000000, -1.000000000000000000, -0.000000000000000000 ) ) ;
#4963 = DIRECTION ( 'NONE',  ( -0.000000000000000000, -1.000000000000000000, -0.000000000000000000 ) ) ;
#4964 = DIRECTION ( 'NONE',  ( -1.188208965918165239E-16, -1.880121038077813132E-16, -1.000000000000000000 ) ) ;
#4965 = CARTESIAN_POINT ( 'NONE',  ( 8.474859994195282908, 38.56284415653841791, 47.04930799450051637 ) ) ;
#4966 = PRESENTATION_STYLE_ASSIGNMENT (( #7752 ) ) ;
#4967 = ORIENTED_EDGE ( 'NONE', *, *, #12361, .T. ) ;
#4968 = ORIENTED_EDGE ( 'NONE', *, *, #11647, .F. ) ;
#4969 = ADVANCED_FACE ( 'NONE', ( #2344 ), #11921, .F. ) ;
#4970 = FACE_OUTER_BOUND ( 'NONE', #26014, .T. ) ;
#4971 = EDGE_CURVE ( 'NONE', #26330, #17665, #8257, .T. ) ;
#4972 = CARTESIAN_POINT ( 'NONE',  ( 49.50463956150868228, 24.97506988763833036, 46.15219500445987677 ) ) ;
#4973 = CARTESIAN_POINT ( 'NONE',  ( 45.47421713364555274, 22.88065857334294861, 45.99599230681428708 ) ) ;
#4974 = CARTESIAN_POINT ( 'NONE',  ( 21.09992658989239089, 28.84143805560861296, 47.04930799450051637 ) ) ;
#4975 = AXIS2_PLACEMENT_3D ( 'NONE', #27104, #17418, #14969 ) ;
#4976 = ORIENTED_EDGE ( 'NONE', *, *, #20377, .F. ) ;
#4977 = DIRECTION ( 'NONE',  ( -0.9612616959383221138, -0.2756373558169876170, 0.000000000000000000 ) ) ;
#4978 = CARTESIAN_POINT ( 'NONE',  ( 33.72499318558949710, 27.34184655352419568, 47.04930799450051637 ) ) ;
#4979 = DIRECTION ( 'NONE',  ( -1.101824276508909887E-16, 1.000000000000000000, -0.000000000000000000 ) ) ;
#4980 = ORIENTED_EDGE ( 'NONE', *, *, #14575, .F. ) ;
#4981 = VERTEX_POINT ( 'NONE', #32058 ) ;
#4982 = CYLINDRICAL_SURFACE ( 'NONE', #534, 2.000000000000001776 ) ;
#4983 = DIRECTION ( 'NONE',  ( 1.234978253042719660E-16, -1.000000000000000000, -1.109335647967047851E-31 ) ) ;
#4984 = AXIS2_PLACEMENT_3D ( 'NONE', #3293, #15775, #347 ) ;
#4985 = CIRCLE ( 'NONE', #8624, 0.1249999999999966416 ) ;
#4986 = DIRECTION ( 'NONE',  ( -0.2756373558169954441, 0.9612616959383198934, -1.479773560108263204E-16 ) ) ;
#4987 = CARTESIAN_POINT ( 'NONE',  ( -41.40207097079809984, 10.37330416413728962, 36.63067884439899302 ) ) ;
#4988 = AXIS2_PLACEMENT_3D ( 'NONE', #11967, #13956, #23947 ) ;
#4989 = FACE_OUTER_BOUND ( 'NONE', #30709, .T. ) ;
#4990 = ORIENTED_EDGE ( 'NONE', *, *, #9116, .F. ) ;
#4991 = EDGE_CURVE ( 'NONE', #14507, #1187, #21878, .T. ) ;
#4992 = VERTEX_POINT ( 'NONE', #27290 ) ;
#4993 = CARTESIAN_POINT ( 'NONE',  ( 47.09785597605719687, 24.86454579224779593, 47.04930799450078638 ) ) ;
#4994 = ORIENTED_EDGE ( 'NONE', *, *, #3965, .T. ) ;
#4995 = VECTOR ( 'NONE', #15408, 999.9999999999998863 ) ;
#4996 = EDGE_CURVE ( 'NONE', #15058, #10568, #19570, .T. ) ;
#4997 = CARTESIAN_POINT ( 'NONE',  ( 21.09992658989238734, 38.56284415653841791, 47.04930799450051637 ) ) ;
#4998 = LINE ( 'NONE', #30113, #17691 ) ;
#4999 = CIRCLE ( 'NONE', #25373, 20.58349629884742882 ) ;
#5000 = AXIS2_PLACEMENT_3D ( 'NONE', #6651, #4186, #27155 ) ;
#5001 = AXIS2_PLACEMENT_3D ( 'NONE', #917, #13563, #1232 ) ;
#5002 = EDGE_CURVE ( 'NONE', #9845, #7831, #9894, .T. ) ;
#5003 = EDGE_LOOP ( 'NONE', ( #16613, #13069, #19012, #31542 ) ) ;
#5004 = CARTESIAN_POINT ( 'NONE',  ( -40.83597905555367902, 8.457813048054211080, 34.59301614167199546 ) ) ;
#5005 = EDGE_LOOP ( 'NONE', ( #15590, #16305, #5185, #14288 ) ) ;
#5006 = VECTOR ( 'NONE', #19923, 1000.000000000000114 ) ;
#5007 = LINE ( 'NONE', #15173, #15728 ) ;
#5008 = DIRECTION ( 'NONE',  ( 0.4848096202463636484, 0.8746197071393810862, 0.000000000000000000 ) ) ;
#5009 = CARTESIAN_POINT ( 'NONE',  ( -42.50084779003665147, 14.56798984196178637, 37.04930799450052348 ) ) ;
#5010 = CARTESIAN_POINT ( 'NONE',  ( -41.73034863705382946, 11.48775164340967514, 57.04930799450051637 ) ) ;
#5011 = ORIENTED_EDGE ( 'NONE', *, *, #2770, .T. ) ;
#5012 = ADVANCED_FACE ( 'NONE', ( #14335 ), #17267, .T. ) ;
#5013 = CARTESIAN_POINT ( 'NONE',  ( 76.14455416958249145, -3.653843372214094387, 80.65498324892040216 ) ) ;
#5014 = CARTESIAN_POINT ( 'NONE',  ( -48.24907229644473716, 10.92050229712533316, 59.54930799450050927 ) ) ;
#5015 = EDGE_CURVE ( 'NONE', #1586, #15332, #29259, .T. ) ;
#5016 = CARTESIAN_POINT ( 'NONE',  ( 21.09785597605719332, 25.76454579224776964, 47.04930799450051637 ) ) ;
#5017 = DIRECTION ( 'NONE',  ( -1.000000000000000000, 0.000000000000000000, 0.000000000000000000 ) ) ;
#5018 = CYLINDRICAL_SURFACE ( 'NONE', #27313, 25.00000000000000000 ) ;
#5019 = ORIENTED_EDGE ( 'NONE', *, *, #14270, .F. ) ;
#5020 = CARTESIAN_POINT ( 'NONE',  ( 21.09785597605720042, -13.68834655544033652, 47.04930799450051637 ) ) ;
#5021 = CARTESIAN_POINT ( 'NONE',  ( -23.40214402394279247, 13.86454579224779948, 47.04930799450052348 ) ) ;
#5022 = EDGE_LOOP ( 'NONE', ( #3418, #66, #29323, #28044 ) ) ;
#5023 = CARTESIAN_POINT ( 'NONE',  ( 21.09992658989238734, 38.56284415653841791, 47.04930799450051637 ) ) ;
#5024 = DIRECTION ( 'NONE',  ( -1.101824276508909887E-16, 1.000000000000000000, -0.000000000000000000 ) ) ;
#5025 = ORIENTED_EDGE ( 'NONE', *, *, #8427, .T. ) ;
#5026 = AXIS2_PLACEMENT_3D ( 'NONE', #8509, #13918, #28532 ) ;
#5027 = DIRECTION ( 'NONE',  ( 0.8746197071393925215, -0.4848096202463429982, -8.676864087101708112E-18 ) ) ;
#5028 = ORIENTED_EDGE ( 'NONE', *, *, #22871, .F. ) ;
#5029 = EDGE_CURVE ( 'NONE', #2485, #32314, #29740, .T. ) ;
#5030 = AXIS2_PLACEMENT_3D ( 'NONE', #1357, #19568, #31405 ) ;
#5031 = COLOUR_RGB ( '',0.7921568627450980005, 0.8196078431372548767, 0.9333333333333333481 ) ;
#5032 = AXIS2_PLACEMENT_3D ( 'NONE', #12350, #24652, #27443 ) ;
#5033 = ORIENTED_EDGE ( 'NONE', *, *, #22865, .T. ) ;
#5034 = CIRCLE ( 'NONE', #7116, 71.29999999999996874 ) ;
#5035 = EDGE_CURVE ( 'NONE', #31841, #28626, #3533, .T. ) ;
#5036 = CARTESIAN_POINT ( 'NONE',  ( -42.38687957179150345, 4.148162238788003719, 57.04930799450051637 ) ) ;
#5037 = EDGE_CURVE ( 'NONE', #29666, #18375, #30289, .T. ) ;
#5038 = EDGE_LOOP ( 'NONE', ( #16945, #11537, #670 ) ) ;
#5039 = EDGE_LOOP ( 'NONE', ( #6246, #6530, #31787, #5377 ) ) ;
#5040 = CARTESIAN_POINT ( 'NONE',  ( 33.71785032049098163, 30.71664230456641675, 47.04930799450051637 ) ) ;
#5041 = CARTESIAN_POINT ( 'NONE',  ( -44.22675629202193903, -5.639587714294394871, 52.99386105124461466 ) ) ;
#5042 = CARTESIAN_POINT ( 'NONE',  ( 21.09992658989238734, 32.54735957529758394, 47.04930799450051637 ) ) ;
#5043 = DIRECTION ( 'NONE',  ( 0.000000000000000000, 0.000000000000000000, -1.000000000000000000 ) ) ;
#5044 = CARTESIAN_POINT ( 'NONE',  ( 21.09785597605720753, 15.19538130838178169, 47.04930799450052348 ) ) ;
#5045 = VERTEX_POINT ( 'NONE', #9738 ) ;
#5046 = CARTESIAN_POINT ( 'NONE',  ( -12.65020122165379668, -2.578969365796068836, 101.3081496656164688 ) ) ;
#5047 = EDGE_LOOP ( 'NONE', ( #821, #23775, #19329, #27376 ) ) ;
#5048 = CARTESIAN_POINT ( 'NONE',  ( -35.21912017334022948, -4.034017897931858165, 13.59333530262071932 ) ) ;
#5049 = EDGE_CURVE ( 'NONE', #11329, #20520, #29756, .T. ) ;
#5050 = ORIENTED_EDGE ( 'NONE', *, *, #22218, .T. ) ;
#5051 = DIRECTION ( 'NONE',  ( -1.101824276508909887E-16, 1.000000000000000000, -0.000000000000000000 ) ) ;
#5052 = CARTESIAN_POINT ( 'NONE',  ( 45.33610888377108239, 19.86454579224779948, 45.90639628189065746 ) ) ;
#5053 = DIRECTION ( 'NONE',  ( -0.000000000000000000, -1.000000000000000000, -0.000000000000000000 ) ) ;
#5054 = EDGE_CURVE ( 'NONE', #29214, #18754, #26487, .T. ) ;
#5055 = CARTESIAN_POINT ( 'NONE',  ( 48.83862994770794330, 29.35457786121581591, 48.17861352429476796 ) ) ;
#5056 = LINE ( 'NONE', #15066, #8960 ) ;
#5057 = DIRECTION ( 'NONE',  ( 0.000000000000000000, 0.000000000000000000, 1.000000000000000000 ) ) ;
#5058 = ORIENTED_EDGE ( 'NONE', *, *, #19441, .F. ) ;
#5059 = DIRECTION ( 'NONE',  ( -1.000000000000000000, -1.101824276508909764E-16, 0.000000000000000000 ) ) ;
#5060 = CARTESIAN_POINT ( 'NONE',  ( 21.09785597605719332, 40.56454579224780588, 77.04930799450052348 ) ) ;
#5061 = ORIENTED_EDGE ( 'NONE', *, *, #17980, .F. ) ;
#5062 = CYLINDRICAL_SURFACE ( 'NONE', #6403, 78.50000000000000000 ) ;
#5063 = VERTEX_POINT ( 'NONE', #20374 ) ;
#5064 =( BOUNDED_CURVE ( )  B_SPLINE_CURVE ( 3, ( #21412, #3874, #6823, #19276 ),
 .UNSPECIFIED., .F., .F. ) 
 B_SPLINE_CURVE_WITH_KNOTS ( ( 4, 4 ),
 ( 5.930963073318635814, 6.283185307179586232 ),
 .UNSPECIFIED. ) 
 CURVE ( )  GEOMETRIC_REPRESENTATION_ITEM ( )  RATIONAL_B_SPLINE_CURVE ( ( 1.000000000000000000, 0.9896883177220884287, 0.9896883177220884287, 1.000000000000000000 ) ) 
 REPRESENTATION_ITEM ( '' )  );
#5065 = VERTEX_POINT ( 'NONE', #7442 ) ;
#5066 = DIRECTION ( 'NONE',  ( -0.9612616959383313286, -0.2756373558169555871, 0.000000000000000000 ) ) ;
#5067 = ORIENTED_EDGE ( 'NONE', *, *, #3322, .T. ) ;
#5068 = AXIS2_PLACEMENT_3D ( 'NONE', #13303, #30695, #15576 ) ;
#5069 = CARTESIAN_POINT ( 'NONE',  ( -40.51565501380215295, 9.065589196111961456, 58.05249952744806308 ) ) ;
#5070 = VERTEX_POINT ( 'NONE', #20063 ) ;
#5071 = EDGE_CURVE ( 'NONE', #21917, #22795, #5134, .T. ) ;
#5072 = CARTESIAN_POINT ( 'NONE',  ( 45.97377588299919893, 23.04411619146718238, 46.99092872297675427 ) ) ;
#5073 = AXIS2_PLACEMENT_3D ( 'NONE', #10017, #27569, #2618 ) ;
#5074 = EDGE_LOOP ( 'NONE', ( #5386, #17473, #10996, #26237 ) ) ;
#5075 = CARTESIAN_POINT ( 'NONE',  ( 21.09992658989238734, 31.34164230456639544, 47.04930799450051637 ) ) ;
#5076 = DIRECTION ( 'NONE',  ( -1.000000000000000000, -1.101824276508909887E-16, 0.000000000000000000 ) ) ;
#5077 = DIRECTION ( 'NONE',  ( -1.101824276508909887E-16, 1.000000000000000000, -0.000000000000000000 ) ) ;
#5078 = CARTESIAN_POINT ( 'NONE',  ( 46.02876340639226527, 28.96789516297709355, 44.95353858666495483 ) ) ;
#5079 = ORIENTED_EDGE ( 'NONE', *, *, #28399, .F. ) ;
#5080 = ORIENTED_EDGE ( 'NONE', *, *, #5015, .F. ) ;
#5081 = DIRECTION ( 'NONE',  ( -0.000000000000000000, 1.000000000000000000, 0.000000000000000000 ) ) ;
#5082 = ADVANCED_FACE ( 'NONE', ( #3429 ), #3037, .T. ) ;
#5083 = EDGE_LOOP ( 'NONE', ( #26210, #18236 ) ) ;
#5084 = DIRECTION ( 'NONE',  ( -1.000000000000000000, -1.101824276508909887E-16, 0.000000000000000000 ) ) ;
#5085 = DIRECTION ( 'NONE',  ( 0.000000000000000000, 1.000000000000000000, -0.000000000000000000 ) ) ;
#5086 = DIRECTION ( 'NONE',  ( 0.4441739386572013948, 0.2110602665713099679, 0.8707256032141218460 ) ) ;
#5087 = CARTESIAN_POINT ( 'NONE',  ( -39.58809650894544774, 2.596771453999702661, 48.24930799450051211 ) ) ;
#5088 = FACE_OUTER_BOUND ( 'NONE', #5022, .T. ) ;
#5089 = CONTEXT_DEPENDENT_SHAPE_REPRESENTATION ( #25865, #4590 ) ;
#5090 = ORIENTED_EDGE ( 'NONE', *, *, #27637, .F. ) ;
#5091 = ORIENTED_EDGE ( 'NONE', *, *, #30269, .T. ) ;
#5092 = FACE_OUTER_BOUND ( 'NONE', #9779, .T. ) ;
#5093 = AXIS2_PLACEMENT_3D ( 'NONE', #29846, #19985, #2099 ) ;
#5094 = CARTESIAN_POINT ( 'NONE',  ( 21.09785597605720042, -14.24176827912842391, 47.04930799450051637 ) ) ;
#5095 = DIRECTION ( 'NONE',  ( 1.000000000000000000, -0.000000000000000000, -0.000000000000000000 ) ) ;
#5096 = VERTEX_POINT ( 'NONE', #2503 ) ;
#5097 = CARTESIAN_POINT ( 'NONE',  ( 52.20591152541699387, -5.935668773294350054, 107.4618278357158374 ) ) ;
#5098 = ORIENTED_EDGE ( 'NONE', *, *, #9790, .T. ) ;
#5099 = DIRECTION ( 'NONE',  ( -1.101824276508909887E-16, 1.000000000000000000, -0.000000000000000000 ) ) ;
#5100 = DIRECTION ( 'NONE',  ( -1.000000000000000000, 0.000000000000000000, 0.000000000000000000 ) ) ;
#5101 = AXIS2_PLACEMENT_3D ( 'NONE', #29298, #16329, #19443 ) ;
#5102 = CARTESIAN_POINT ( 'NONE',  ( 21.09785597605720753, -5.098646251524523443, 47.04930799450052348 ) ) ;
#5103 = ORIENTED_EDGE ( 'NONE', *, *, #2404, .T. ) ;
#5104 = CIRCLE ( 'NONE', #29210, 12.36707279061065101 ) ;
#5105 = ORIENTED_EDGE ( 'NONE', *, *, #12586, .T. ) ;
#5106 = CARTESIAN_POINT ( 'NONE',  ( -42.82457667231739151, 15.69696662191612901, 37.04930799450052348 ) ) ;
#5107 = CIRCLE ( 'NONE', #15592, 0.1999999999999987899 ) ;
#5108 = CARTESIAN_POINT ( 'NONE',  ( 49.65101332465108186, 24.93501648625822398, 46.52608845888364186 ) ) ;
#5109 = CARTESIAN_POINT ( 'NONE',  ( 48.94625023931840957, 26.75784706826093284, 46.10640627770150246 ) ) ;
#5110 = VERTEX_POINT ( 'NONE', #13459 ) ;
#5111 = CARTESIAN_POINT ( 'NONE',  ( -38.65545646816406133, -3.086612947480494196, 80.82450247980625591 ) ) ;
#5112 = AXIS2_PLACEMENT_3D ( 'NONE', #8913, #21055, #6459 ) ;
#5113 = DIRECTION ( 'NONE',  ( -1.101824276508909887E-16, 1.000000000000000000, -0.000000000000000000 ) ) ;
#5114 = CARTESIAN_POINT ( 'NONE',  ( 46.96819297411687444, 27.46988759933318747, 49.54594323136014822 ) ) ;
#5115 = DIRECTION ( 'NONE',  ( -0.1949050434465281478, 0.6797146636928673713, 0.7071067811865469066 ) ) ;
#5116 = EDGE_CURVE ( 'NONE', #6679, #19678, #6189, .T. ) ;
#5117 = DIRECTION ( 'NONE',  ( 0.000000000000000000, -1.000000000000000000, 0.000000000000000000 ) ) ;
#5118 = AXIS2_PLACEMENT_3D ( 'NONE', #5677, #23715, #18461 ) ;
#5119 = CARTESIAN_POINT ( 'NONE',  ( 33.71785032049135111, 27.71664230456639899, 47.04930799450051637 ) ) ;
#5120 = FACE_OUTER_BOUND ( 'NONE', #15545, .T. ) ;
#5121 = EDGE_CURVE ( 'NONE', #2124, #20651, #22515, .T. ) ;
#5122 = DIRECTION ( 'NONE',  ( 0.000000000000000000, 1.000000000000000000, -0.000000000000000000 ) ) ;
#5124 = EDGE_CURVE ( 'NONE', #13889, #26169, #22408, .T. ) ;
#5123 = FACE_OUTER_BOUND ( 'NONE', #6689, .T. ) ;
#5125 = B_SPLINE_SURFACE_WITH_KNOTS ( 'NONE', 3, 3, ( 
 ( #10634, #20625, #278, #30651, #2902, #10304 ),
 ( #28019, #8316, #20290, #12931, #28345, #30322 ),
 ( #7836, #27860, #15382, #25388, #22919, #436 ),
 ( #10464, #11112, #31608, #4027, #21408, #16499 ),
 ( #1559, #26351, #18476, #1401, #21095, #13890 ),
 ( #14048, #8954, #18786, #6169, #19110, #16175 ) ),
 .UNSPECIFIED., .F., .F., .F.,
 ( 4, 2, 4 ),
 ( 4, 2, 4 ),
 ( 0.000000000000000000, 0.5000000000000000000, 1.000000000000000000 ),
 ( 0.000000000000000000, 0.5000000000000000000, 1.000000000000000000 ),
 .UNSPECIFIED. ) ;
#5126 = EDGE_CURVE ( 'NONE', #3409, #6259, #206, .T. ) ;
#5127 = EDGE_CURVE ( 'NONE', #21917, #2124, #941, .T. ) ;
#5128 = CARTESIAN_POINT ( 'NONE',  ( 21.09992658989238734, 32.34184655352418503, 47.04930799450051637 ) ) ;
#5129 = CYLINDRICAL_SURFACE ( 'NONE', #1598, 16.99999999999999289 ) ;
#5130 = EDGE_LOOP ( 'NONE', ( #15036, #27392, #19586, #25265 ) ) ;
#5131 = ORIENTED_EDGE ( 'NONE', *, *, #9830, .F. ) ;
#5132 = DIRECTION ( 'NONE',  ( -1.000000000000000000, 0.000000000000000000, 0.000000000000000000 ) ) ;
#5133 = FACE_OUTER_BOUND ( 'NONE', #1821, .T. ) ;
#5134 = LINE ( 'NONE', #5462, #18720 ) ;
#5135 = CARTESIAN_POINT ( 'NONE',  ( 80.85108986838918099, -5.935454207752202116, 77.87546120947918382 ) ) ;
#5136 = VERTEX_POINT ( 'NONE', #4973 ) ;
#5137 = DIRECTION ( 'NONE',  ( 0.000000000000000000, 0.000000000000000000, -1.000000000000000000 ) ) ;
#5138 = LINE ( 'NONE', #29598, #12054 ) ;
#5139 = VERTEX_POINT ( 'NONE', #16062 ) ;
#5140 = ORIENTED_EDGE ( 'NONE', *, *, #17571, .T. ) ;
#5141 = CARTESIAN_POINT ( 'NONE',  ( 5.570303151842745493, 15.19538130838178169, 47.04930799450052348 ) ) ;
#5142 = CARTESIAN_POINT ( 'NONE',  ( 48.94625023931840957, 27.45784706826093213, 46.10640627770150246 ) ) ;
#5143 = AXIS2_PLACEMENT_3D ( 'NONE', #30789, #8303, #28168 ) ;
#5144 = CARTESIAN_POINT ( 'NONE',  ( 21.09785597605720042, -16.03545420775220265, -22.54971151909227700 ) ) ;
#5145 = AXIS2_PLACEMENT_3D ( 'NONE', #10290, #17324, #17159 ) ;
#5146 = DIRECTION ( 'NONE',  ( -1.000000000000000000, 0.000000000000000000, 0.000000000000000000 ) ) ;
#5147 = CARTESIAN_POINT ( 'NONE',  ( 45.99596926870651004, 19.86454579224779948, 44.88925112391522987 ) ) ;
#5148 = CIRCLE ( 'NONE', #21375, 0.1250000000000001110 ) ;
#5149 = AXIS2_PLACEMENT_3D ( 'NONE', #11396, #1383, #6316 ) ;
#5150 = ORIENTED_EDGE ( 'NONE', *, *, #20964, .F. ) ;
#5151 = LINE ( 'NONE', #12876, #20346 ) ;
#5152 = EDGE_CURVE ( 'NONE', #25906, #12709, #19265, .T. ) ;
#5153 = ORIENTED_EDGE ( 'NONE', *, *, #16441, .T. ) ;
#5154 = DIRECTION ( 'NONE',  ( -0.8907924397839087627, -1.100109291107994187E-16, 0.4544104193609907472 ) ) ;
#5155 = CARTESIAN_POINT ( 'NONE',  ( 8.732853799281734553, 38.56284415653841791, 47.04930799450051637 ) ) ;
#5156 = AXIS2_PLACEMENT_3D ( 'NONE', #10734, #26130, #3321 ) ;
#5157 = AXIS2_PLACEMENT_3D ( 'NONE', #6154, #14363, #24357 ) ;
#5158 = VECTOR ( 'NONE', #11161, 1000.000000000000000 ) ;
#5159 = ORIENTED_EDGE ( 'NONE', *, *, #28137, .F. ) ;
#5160 = DIRECTION ( 'NONE',  ( -1.101824276508909887E-16, 1.000000000000000000, -0.000000000000000000 ) ) ;
#5161 = ORIENTED_EDGE ( 'NONE', *, *, #671, .F. ) ;
#5162 = AXIS2_PLACEMENT_3D ( 'NONE', #14009, #24004, #13846 ) ;
#5163 = EDGE_CURVE ( 'NONE', #802, #11200, #23983, .T. ) ;
#5164 = LINE ( 'NONE', #10582, #27783 ) ;
#5165 = CARTESIAN_POINT ( 'NONE',  ( 8.732853799281732776, 25.22145308207319303, 47.04930799450051637 ) ) ;
#5166 = EDGE_CURVE ( 'NONE', #3444, #15199, #20847, .T. ) ;
#5167 = AXIS2_PLACEMENT_3D ( 'NONE', #22561, #14381, #20107 ) ;
#5168 = DIRECTION ( 'NONE',  ( -0.3428121700606640565, -0.6184495258776567805, -0.7071067811865474617 ) ) ;
#5169 = EDGE_CURVE ( 'NONE', #31904, #9250, #10912, .T. ) ;
#5170 = DIRECTION ( 'NONE',  ( 0.000000000000000000, 0.000000000000000000, -1.000000000000000000 ) ) ;
#5171 = ORIENTED_EDGE ( 'NONE', *, *, #22634, .F. ) ;
#5172 = CARTESIAN_POINT ( 'NONE',  ( 78.71125094149621759, -5.832427868686499650, 78.63111537559601061 ) ) ;
#5173 = CARTESIAN_POINT ( 'NONE',  ( -9.880269303432735128, -5.935454207752202116, -13.51052302966392205 ) ) ;
#5174 = DIRECTION ( 'NONE',  ( 1.188208965918164993E-16, 1.880121038077812639E-16, 1.000000000000000000 ) ) ;
#5175 = AXIS2_PLACEMENT_3D ( 'NONE', #26946, #23831, #1504 ) ;
#5176 = CARTESIAN_POINT ( 'NONE',  ( 75.45786391719093444, -1.094061166257011664, 80.59074881016049119 ) ) ;
#5177 = ORIENTED_EDGE ( 'NONE', *, *, #5822, .F. ) ;
#5178 = CARTESIAN_POINT ( 'NONE',  ( 21.09785597605719332, 43.75535478762431296, 47.04930799450051637 ) ) ;
#5179 = ORIENTED_EDGE ( 'NONE', *, *, #3852, .T. ) ;
#5180 = CARTESIAN_POINT ( 'NONE',  ( -41.07644103349282005, 9.237697617431789965, 39.54930799450052348 ) ) ;
#5181 = DIRECTION ( 'NONE',  ( -0.000000000000000000, 1.000000000000000000, -0.000000000000000000 ) ) ;
#5182 = CARTESIAN_POINT ( 'NONE',  ( 33.37634396954518223, 32.59164230456639899, 47.04930799450051637 ) ) ;
#5183 = ORIENTED_EDGE ( 'NONE', *, *, #11051, .F. ) ;
#5184 = DIRECTION ( 'NONE',  ( 0.000000000000000000, 0.000000000000000000, -1.000000000000000000 ) ) ;
#5185 = ORIENTED_EDGE ( 'NONE', *, *, #2834, .T. ) ;
#5186 = CIRCLE ( 'NONE', #31397, 1.500000000000001332 ) ;
#5187 = EDGE_CURVE ( 'NONE', #180, #25211, #19161, .T. ) ;
#5188 = ORIENTED_EDGE ( 'NONE', *, *, #4996, .T. ) ;
#5189 = AXIS2_PLACEMENT_3D ( 'NONE', #19362, #26761, #21828 ) ;
#5190 = EDGE_CURVE ( 'NONE', #4111, #3549, #32396, .T. ) ;
#5191 = ADVANCED_FACE ( 'NONE', ( #9323 ), #9331, .T. ) ;
#5192 = AXIS2_PLACEMENT_3D ( 'NONE', #27291, #29593, #24834 ) ;
#5193 = CARTESIAN_POINT ( 'NONE',  ( 21.09785597605719332, 25.56454579224779167, 60.24930799450052632 ) ) ;
#5194 = CARTESIAN_POINT ( 'NONE',  ( 45.52675994804781112, 26.01155426599985532, 49.47108226228597516 ) ) ;
#5195 = VERTEX_POINT ( 'NONE', #21791 ) ;
#5196 = VERTEX_POINT ( 'NONE', #1776 ) ;
#5197 = CARTESIAN_POINT ( 'NONE',  ( -44.30341829581058022, -5.862881430098965119, 53.49729029702648830 ) ) ;
#5198 = DIRECTION ( 'NONE',  ( -0.3428121700606640565, -0.6184495258776567805, 0.7071067811865474617 ) ) ;
#5199 = DIRECTION ( 'NONE',  ( -0.000000000000000000, -1.000000000000000000, 0.000000000000000000 ) ) ;
#5200 = DIRECTION ( 'NONE',  ( -1.000000000000000000, 0.000000000000000000, 0.000000000000000000 ) ) ;
#5201 = EDGE_CURVE ( 'NONE', #1586, #8660, #5657, .T. ) ;
#5202 = ORIENTED_EDGE ( 'NONE', *, *, #31623, .T. ) ;
#5203 = CARTESIAN_POINT ( 'NONE',  ( -12.32273293319885532, -0.6526263882323729559, 100.2535347340254219 ) ) ;
#5204 = VERTEX_POINT ( 'NONE', #13938 ) ;
#5205 = CARTESIAN_POINT ( 'NONE',  ( 46.27991722120741258, 29.86454579224779948, 45.44588160288975587 ) ) ;
#5206 = CARTESIAN_POINT ( 'NONE',  ( -40.74365851677129768, 8.439942589813739460, 34.54930799450052348 ) ) ;
#5207 = CIRCLE ( 'NONE', #16196, 0.1250000000000001110 ) ;
#5208 = VERTEX_POINT ( 'NONE', #19324 ) ;
#5209 = FACE_OUTER_BOUND ( 'NONE', #14516, .T. ) ;
#5210 = FACE_OUTER_BOUND ( 'NONE', #30047, .T. ) ;
#5211 = AXIS2_PLACEMENT_3D ( 'NONE', #571, #13061, #10763 ) ;
#5212 = DIRECTION ( 'NONE',  ( -0.000000000000000000, -1.000000000000000000, -0.000000000000000000 ) ) ;
#5213 = LINE ( 'NONE', #27862, #32044 ) ;
#5214 = CARTESIAN_POINT ( 'NONE',  ( -42.94875805865124363, 16.13003858227299858, 37.04930799450052348 ) ) ;
#5215 = CARTESIAN_POINT ( 'NONE',  ( 48.18662509608405031, 27.89624452788248377, 49.18364984542562013 ) ) ;
#5216 = FACE_BOUND ( 'NONE', #30469, .T. ) ;
#5217 = DIRECTION ( 'NONE',  ( -1.000000000000000000, 0.000000000000000000, 0.000000000000000000 ) ) ;
#5218 = ORIENTED_EDGE ( 'NONE', *, *, #2554, .F. ) ;
#5219 = CARTESIAN_POINT ( 'NONE',  ( 21.09785597605720753, 14.86454579224779948, 47.04930799450052348 ) ) ;
#5220 = ORIENTED_EDGE ( 'NONE', *, *, #18289, .F. ) ;
#5221 = AXIS2_PLACEMENT_3D ( 'NONE', #31500, #28702, #9008 ) ;
#5222 = DIRECTION ( 'NONE',  ( 0.000000000000000000, 0.000000000000000000, -1.000000000000000000 ) ) ;
#5223 = VERTEX_POINT ( 'NONE', #8837 ) ;
#5224 = AXIS2_PLACEMENT_3D ( 'NONE', #3924, #817, #13946 ) ;
#5225 = EDGE_CURVE ( 'NONE', #10602, #27059, #26611, .T. ) ;
#5226 = ORIENTED_EDGE ( 'NONE', *, *, #21782, .T. ) ;
#5227 = EDGE_CURVE ( 'NONE', #2178, #7469, #28725, .T. ) ;
#5228 = VERTEX_POINT ( 'NONE', #29029 ) ;
#5229 = EDGE_CURVE ( 'NONE', #18133, #31159, #5148, .T. ) ;
#5230 = CIRCLE ( 'NONE', #27215, 12.36707279061065101 ) ;
#5231 = ADVANCED_FACE ( 'NONE', ( #26402 ), #26887, .T. ) ;
#5232 = TOROIDAL_SURFACE ( 'NONE', #1025, 41.50000000000000000, 1.999999999999998224 ) ;
#5233 = ADVANCED_FACE ( 'NONE', ( #18833 ), #13777, .F. ) ;
#5234 = ORIENTED_EDGE ( 'NONE', *, *, #8234, .F. ) ;
#5235 = CARTESIAN_POINT ( 'NONE',  ( 46.53577443378190281, 23.10527845304106620, 47.02011620365084354 ) ) ;
#5236 = VECTOR ( 'NONE', #12165, 1000.000000000000000 ) ;
#5237 = AXIS2_PLACEMENT_3D ( 'NONE', #6788, #16469, #4159 ) ;
#5238 = EDGE_LOOP ( 'NONE', ( #20326, #14785, #17444, #17400 ) ) ;
#5239 = DIRECTION ( 'NONE',  ( -1.101824276508909887E-16, 1.000000000000000000, -0.000000000000000000 ) ) ;
#5240 = AXIS2_PLACEMENT_3D ( 'NONE', #13042, #2534, #15334 ) ;
#5241 = CARTESIAN_POINT ( 'NONE',  ( 49.32738855505253639, 29.28333847617543739, 46.19910593250668285 ) ) ;
#5242 = CARTESIAN_POINT ( 'NONE',  ( 48.23388202445966044, 26.25087065737812253, 49.27628909396054979 ) ) ;
#5243 = CARTESIAN_POINT ( 'NONE',  ( 45.24946171279598417, 25.62124452788248874, 47.99220971130007030 ) ) ;
#5244 = TOROIDAL_SURFACE ( 'NONE', #23588, 12.40141737965284108, 0.1249999999999997918 ) ;
#5245 = ORIENTED_EDGE ( 'NONE', *, *, #4398, .T. ) ;
#5246 = VERTEX_POINT ( 'NONE', #14098 ) ;
#5247 = LINE ( 'NONE', #22310, #2208 ) ;
#5248 = EDGE_LOOP ( 'NONE', ( #4570, #8141, #13699, #32453 ) ) ;
#5249 = LINE ( 'NONE', #15258, #5266 ) ;
#5250 = DIRECTION ( 'NONE',  ( -1.000000000000000000, 0.000000000000000000, 0.000000000000000000 ) ) ;
#5251 = CARTESIAN_POINT ( 'NONE',  ( -40.69332644341264427, 6.790879890547277142, 34.68541711214640344 ) ) ;
#5252 = CARTESIAN_POINT ( 'NONE',  ( 21.09785597605720753, 13.86454579224779948, 47.04930799450052348 ) ) ;
#5253 = CARTESIAN_POINT ( 'NONE',  ( 48.40186567930497574, 25.32957786121582444, 45.03923535223908203 ) ) ;
#5254 = ORIENTED_EDGE ( 'NONE', *, *, #8808, .T. ) ;
#5255 = EDGE_LOOP ( 'NONE', ( #26407, #23963, #30773, #28159 ) ) ;
#5256 = CARTESIAN_POINT ( 'NONE',  ( 48.77917452769285944, 20.36454579224779948, 50.34524002170125101 ) ) ;
#5257 = CIRCLE ( 'NONE', #31448, 0.1000000000000016709 ) ;
#5258 = CARTESIAN_POINT ( 'NONE',  ( 21.09785597605720753, -5.098646251524523443, 47.04930799450052348 ) ) ;
#5259 = DIRECTION ( 'NONE',  ( -0.000000000000000000, 1.000000000000000000, -0.000000000000000000 ) ) ;
#5260 = ORIENTED_EDGE ( 'NONE', *, *, #18116, .F. ) ;
#5261 = CARTESIAN_POINT ( 'NONE',  ( 46.99023568444673060, 27.92451373492759714, 49.12151524109405898 ) ) ;
#5262 = ADVANCED_FACE ( 'NONE', ( #14420, #11309, #24419, #6381 ), #11153, .F. ) ;
#5263 = ORIENTED_EDGE ( 'NONE', *, *, #11852, .F. ) ;
#5264 = LINE ( 'NONE', #25288, #21429 ) ;
#5265 = DIRECTION ( 'NONE',  ( -1.000000000000000000, 0.000000000000000000, 0.000000000000000000 ) ) ;
#5266 = VECTOR ( 'NONE', #25269, 1000.000000000000000 ) ;
#5267 = AXIS2_PLACEMENT_3D ( 'NONE', #6888, #4261, #14281 ) ;
#5268 = ADVANCED_FACE ( 'NONE', ( #3914, #23770 ), #31813, .T. ) ;
#5269 = DIRECTION ( 'NONE',  ( 0.5319835227803600963, -0.2110602665713099124, -0.8200287161831869565 ) ) ;
#5270 = AXIS2_PLACEMENT_3D ( 'NONE', #25346, #17787, #19925 ) ;
#5271 = AXIS2_PLACEMENT_3D ( 'NONE', #24536, #14376, #24373 ) ;
#5272 = CIRCLE ( 'NONE', #28838, 2.500000000000002220 ) ;
#5273 = PRESENTATION_LAYER_ASSIGNMENT (  '', '', ( #1066 ) ) ;
#5274 = EDGE_CURVE ( 'NONE', #5196, #17364, #30826, .T. ) ;
#5275 = ORIENTED_EDGE ( 'NONE', *, *, #31211, .F. ) ;
#5276 = ADVANCED_FACE ( 'NONE', ( #23932 ), #420, .T. ) ;
#5277 = ORIENTED_EDGE ( 'NONE', *, *, #31470, .T. ) ;
#5278 = CARTESIAN_POINT ( 'NONE',  ( 21.09785597605718976, 7.264443105416139801, 66.26382401993569715 ) ) ;
#5279 = DIRECTION ( 'NONE',  ( -1.101824276508909887E-16, 1.000000000000000000, -0.000000000000000000 ) ) ;
#5280 = CARTESIAN_POINT ( 'NONE',  ( 45.24946171279598417, 26.40784706826093498, 47.99220971130007030 ) ) ;
#5281 = AXIS2_PLACEMENT_3D ( 'NONE', #32373, #22184, #12355 ) ;
#5282 = EDGE_LOOP ( 'NONE', ( #7158, #28115, #17849, #4143 ) ) ;
#5283 = FACE_OUTER_BOUND ( 'NONE', #4444, .T. ) ;
#5284 = CARTESIAN_POINT ( 'NONE',  ( 81.47077242904269667, -5.936694392936851195, 15.97589416290124831 ) ) ;
#5285 = CYLINDRICAL_SURFACE ( 'NONE', #32424, 1.500000000000001332 ) ;
#5286 = CARTESIAN_POINT ( 'NONE',  ( 21.09785597605719332, 13.06454579224779877, 47.04930799450051637 ) ) ;
#5287 = VECTOR ( 'NONE', #10305, 999.9999999999998863 ) ;
#5288 = DIRECTION ( 'NONE',  ( -1.101824276508909887E-16, 1.000000000000000000, -0.000000000000000000 ) ) ;
#5289 = FACE_BOUND ( 'NONE', #2744, .T. ) ;
#5290 = CARTESIAN_POINT ( 'NONE',  ( 21.09992658989239089, 29.09143805560861296, 47.04930799450051637 ) ) ;
#5291 = CARTESIAN_POINT ( 'NONE',  ( 45.39590889550878927, 22.93328494799376571, 47.28470721838063184 ) ) ;
#5292 = FACE_OUTER_BOUND ( 'NONE', #4582, .T. ) ;
#5293 = CIRCLE ( 'NONE', #24657, 43.00000000000000000 ) ;
#5294 = CARTESIAN_POINT ( 'NONE',  ( 33.72499318558949710, 31.59143805560860585, 47.04930799450051637 ) ) ;
#5295 = DIRECTION ( 'NONE',  ( -0.000000000000000000, 1.000000000000000000, -0.000000000000000000 ) ) ;
#5296 = CIRCLE ( 'NONE', #6853, 12.62506659569710266 ) ;
#5297 = ORIENTED_EDGE ( 'NONE', *, *, #22376, .F. ) ;
#5298 = ORIENTED_EDGE ( 'NONE', *, *, #31466, .T. ) ;
#5299 = CARTESIAN_POINT ( 'NONE',  ( 21.09785597605720753, 14.86454579224779948, 47.04930799450052348 ) ) ;
#5300 = AXIS2_PLACEMENT_3D ( 'NONE', #13848, #11224, #6460 ) ;
#5301 = DIRECTION ( 'NONE',  ( -1.101824276508909887E-16, 1.000000000000000000, -0.000000000000000000 ) ) ;
#5302 = DIRECTION ( 'NONE',  ( 1.000000000000000000, 0.000000000000000000, 0.000000000000000000 ) ) ;
#5303 = PLANE ( 'NONE',  #10426 ) ;
#5304 = ORIENTED_EDGE ( 'NONE', *, *, #13286, .T. ) ;
#5305 = CARTESIAN_POINT ( 'NONE',  ( -42.73182147790732444, -0.8057266458565844891, 32.04930799450052348 ) ) ;
#5306 = DIRECTION ( 'NONE',  ( -1.224646799147353207E-16, -1.349345573449484691E-32, 1.000000000000000000 ) ) ;
#5307 = CARTESIAN_POINT ( 'NONE',  ( 21.09785597605719332, 11.92558985988973497, 47.04930799450051637 ) ) ;
#5308 = ORIENTED_EDGE ( 'NONE', *, *, #2524, .T. ) ;
#5309 = EDGE_LOOP ( 'NONE', ( #1423, #20680, #29015, #543 ) ) ;
#5310 = DIRECTION ( 'NONE',  ( -1.224646799147353207E-16, -1.349345573449484691E-32, 1.000000000000000000 ) ) ;
#5311 = CARTESIAN_POINT ( 'NONE',  ( 45.79384627280941089, 27.16618040159427139, 49.05938063676249072 ) ) ;
#5312 = B_SPLINE_CURVE_WITH_KNOTS ( 'NONE', 3,
 ( #19104, #26508, #6489, #8779, #8947, #9109, #26834, #16326, #11258, #6649 ),
 .UNSPECIFIED., .F., .F.,
 ( 4, 2, 2, 2, 4 ),
 ( 0.0006731324393515002820, 0.002417216000136425402, 0.004161299560921350414, 0.005905383121706275426, 0.007649466682491198703 ),
 .UNSPECIFIED. ) ;
#5313 = AXIS2_PLACEMENT_3D ( 'NONE', #22269, #27531, #2578 ) ;
#5314 = DIRECTION ( 'NONE',  ( -1.101824276508909887E-16, 1.000000000000000000, -0.000000000000000000 ) ) ;
#5315 = CARTESIAN_POINT ( 'NONE',  ( 21.09992658989238734, 38.56284415653841791, 47.04930799450051637 ) ) ;
#5316 = CARTESIAN_POINT ( 'NONE',  ( -40.28779227465695101, 2.984619150196775372, 38.54930799450052348 ) ) ;
#5317 = EDGE_CURVE ( 'NONE', #6385, #8606, #21628, .T. ) ;
#5318 = VERTEX_POINT ( 'NONE', #5060 ) ;
#5319 = ADVANCED_FACE ( 'NONE', ( #32309 ), #17192, .T. ) ;
#5320 = EDGE_CURVE ( 'NONE', #31117, #7831, #32147, .T. ) ;
#5321 = VECTOR ( 'NONE', #20466, 1000.000000000000114 ) ;
#5322 = CONICAL_SURFACE ( 'NONE', #12136, 58.70143199044622406, 1.269872874662816509 ) ;
#5323 = FACE_OUTER_BOUND ( 'NONE', #30250, .T. ) ;
#5324 = AXIS2_PLACEMENT_3D ( 'NONE', #16861, #15063, #4888 ) ;
#5325 = EDGE_LOOP ( 'NONE', ( #29985, #18356, #28595, #24555 ) ) ;
#5326 = CARTESIAN_POINT ( 'NONE',  ( 45.82550680184641578, 25.16454579224780019, 44.55508916310584056 ) ) ;
#5327 = CYLINDRICAL_SURFACE ( 'NONE', #8287, 0.1000000000000018235 ) ;
#5328 = AXIS2_PLACEMENT_3D ( 'NONE', #14164, #21694, #1510 ) ;
#5329 = VERTEX_POINT ( 'NONE', #133 ) ;
#5330 = CARTESIAN_POINT ( 'NONE',  ( 67.03037309312014713, 14.61319044934410627, 47.04930799450051637 ) ) ;
#5331 = ORIENTED_EDGE ( 'NONE', *, *, #18801, .F. ) ;
#5332 = CARTESIAN_POINT ( 'NONE',  ( -10.74933306299440083, -5.721341737285946749, 105.3592130793008721 ) ) ;
#5333 = CARTESIAN_POINT ( 'NONE',  ( -40.60333149162104860, 7.557375771971046596, 60.54930799450051637 ) ) ;
#5334 = FACE_BOUND ( 'NONE', #28285, .T. ) ;
#5335 = DIRECTION ( 'NONE',  ( 0.000000000000000000, 0.000000000000000000, -1.000000000000000000 ) ) ;
#5336 = ORIENTED_EDGE ( 'NONE', *, *, #6185, .T. ) ;
#5337 = CARTESIAN_POINT ( 'NONE',  ( 45.96182992765471909, 26.60087065737812040, 44.82232689504102296 ) ) ;
#5338 = DIRECTION ( 'NONE',  ( 0.000000000000000000, -1.000000000000000000, 0.000000000000000000 ) ) ;
#5339 = B_SPLINE_CURVE_WITH_KNOTS ( 'NONE', 3,
 ( #17959, #25672, #27980, #22727 ),
 .UNSPECIFIED., .F., .F.,
 ( 4, 4 ),
 ( 0.07166325488466616933, 0.08752405979088770382 ),
 .UNSPECIFIED. ) ;
#5340 = FACE_OUTER_BOUND ( 'NONE', #26145, .T. ) ;
#5341 = CARTESIAN_POINT ( 'NONE',  ( 21.09992658989239089, 27.84184655352419568, 47.04930799450051637 ) ) ;
#5342 = AXIS2_PLACEMENT_3D ( 'NONE', #20623, #25870, #918 ) ;
#5343 = DIRECTION ( 'NONE',  ( -0.000000000000000000, -1.000000000000000000, 0.000000000000000000 ) ) ;
#5344 = EDGE_LOOP ( 'NONE', ( #5711, #22841, #12288, #10331 ) ) ;
#5345 = CIRCLE ( 'NONE', #16839, 0.1250000000000001110 ) ;
#5346 = DIRECTION ( 'NONE',  ( 0.8746197071393926326, -0.4848096202463430537, -8.676864087101709653E-18 ) ) ;
#5347 = CARTESIAN_POINT ( 'NONE',  ( -42.47434154250544225, 4.196643200812637531, 55.74930799450051211 ) ) ;
#5348 = ORIENTED_EDGE ( 'NONE', *, *, #2194, .F. ) ;
#5349 = VECTOR ( 'NONE', #14655, 1000.000000000000114 ) ;
#5350 = DIRECTION ( 'NONE',  ( 0.000000000000000000, 0.000000000000000000, -1.000000000000000000 ) ) ;
#5351 = CARTESIAN_POINT ( 'NONE',  ( -39.64148344771002286, 7.657122216028890982, 32.14930799450051779 ) ) ;
#5352 = CARTESIAN_POINT ( 'NONE',  ( -38.57628410747783221, -5.906256089375805374, 15.45647446568822225 ) ) ;
#5353 = DIRECTION ( 'NONE',  ( 0.000000000000000000, 0.000000000000000000, 1.000000000000000000 ) ) ;
#5354 = ORIENTED_EDGE ( 'NONE', *, *, #14424, .F. ) ;
#5355 = CYLINDRICAL_SURFACE ( 'NONE', #9917, 0.1000000000000004774 ) ;
#5356 = ORIENTED_EDGE ( 'NONE', *, *, #11202, .F. ) ;
#5357 = CIRCLE ( 'NONE', #13236, 65.96844849472888939 ) ;
#5358 = ORIENTED_EDGE ( 'NONE', *, *, #15588, .T. ) ;
#5359 = EDGE_CURVE ( 'NONE', #10117, #6715, #29772, .T. ) ;
#5360 = EDGE_CURVE ( 'NONE', #16253, #9695, #22115, .T. ) ;
#5361 = EDGE_CURVE ( 'NONE', #29666, #27949, #9849, .T. ) ;
#5362 = EDGE_CURVE ( 'NONE', #19781, #17800, #15598, .T. ) ;
#5363 = AXIS2_PLACEMENT_3D ( 'NONE', #7604, #14667, #19900 ) ;
#5364 = CARTESIAN_POINT ( 'NONE',  ( -42.35386648718987601, 15.27751306094253891, 38.53464782781823317 ) ) ;
#5365 = CARTESIAN_POINT ( 'NONE',  ( -39.58809650894544774, 2.596771453999702661, 45.74930799450051211 ) ) ;
#5366 = B_SPLINE_CURVE_WITH_KNOTS ( 'NONE', 3,
 ( #30805, #18000, #12933, #30168, #5870, #3225 ),
 .UNSPECIFIED., .F., .F.,
 ( 4, 2, 4 ),
 ( 0.000000000000000000, 0.5000000000000000000, 1.000000000000000000 ),
 .UNSPECIFIED. ) ;
#5367 = ORIENTED_EDGE ( 'NONE', *, *, #4492, .F. ) ;
#5368 = EDGE_LOOP ( 'NONE', ( #22289, #21422 ) ) ;
#5369 = DIRECTION ( 'NONE',  ( 1.000000000000000000, 0.000000000000000000, 0.000000000000000000 ) ) ;
#5370 = CARTESIAN_POINT ( 'NONE',  ( 21.09992658989238734, 31.21183152705961206, 47.04930799450051637 ) ) ;
#5371 = CARTESIAN_POINT ( 'NONE',  ( -30.26451050232878615, 9.135310954698587338, 74.43234153126013553 ) ) ;
#5372 = CARTESIAN_POINT ( 'NONE',  ( -40.48129536610376533, 8.613360132207176889, 39.44930799450052206 ) ) ;
#5373 = ORIENTED_EDGE ( 'NONE', *, *, #3322, .F. ) ;
#5374 = CARTESIAN_POINT ( 'NONE',  ( -9.278155635207900431, 5.370505999354209692, 98.20157670830246843 ) ) ;
#5375 = VERTEX_POINT ( 'NONE', #32470 ) ;
#5376 = DIRECTION ( 'NONE',  ( -0.000000000000000000, -1.000000000000000000, -0.000000000000000000 ) ) ;
#5377 = ORIENTED_EDGE ( 'NONE', *, *, #25128, .F. ) ;
#5378 = CARTESIAN_POINT ( 'NONE',  ( 9.016997203727585841, 15.24673779880127356, 47.36565641480107303 ) ) ;
#5379 = CARTESIAN_POINT ( 'NONE',  ( -40.10456357475989364, 7.631942973856654433, 53.94930799450051495 ) ) ;
#5380 = LINE ( 'NONE', #3056, #2170 ) ;
#5381 = DIRECTION ( 'NONE',  ( -1.000000000000000000, 0.000000000000000000, 0.000000000000000000 ) ) ;
#5382 = AXIS2_PLACEMENT_3D ( 'NONE', #27898, #7221, #27410 ) ;
#5383 = CARTESIAN_POINT ( 'NONE',  ( 45.35708200440645044, 28.30457786121581876, 45.92000246470679770 ) ) ;
#5384 = LINE ( 'NONE', #2907, #25737 ) ;
#5385 = DIRECTION ( 'NONE',  ( -2.779292025043186357E-18, 1.288349127009862211E-17, -1.000000000000000000 ) ) ;
#5386 = ORIENTED_EDGE ( 'NONE', *, *, #25817, .F. ) ;
#5387 = ADVANCED_FACE ( 'NONE', ( #11951 ), #1451, .T. ) ;
#5388 = ORIENTED_EDGE ( 'NONE', *, *, #11257, .F. ) ;
#5389 = EDGE_CURVE ( 'NONE', #26389, #27795, #17710, .T. ) ;
#5390 = AXIS2_PLACEMENT_3D ( 'NONE', #18817, #25749, #26226 ) ;
#5391 = ORIENTED_EDGE ( 'NONE', *, *, #7539, .T. ) ;
#5392 = CIRCLE ( 'NONE', #25295, 22.00000000000000000 ) ;
#5393 = ORIENTED_EDGE ( 'NONE', *, *, #437, .F. ) ;
#5394 = CYLINDRICAL_SURFACE ( 'NONE', #26718, 12.62506659569710266 ) ;
#5395 = ORIENTED_EDGE ( 'NONE', *, *, #21571, .F. ) ;
#5396 = EDGE_CURVE ( 'NONE', #3842, #29156, #30011, .T. ) ;
#5397 = TOROIDAL_SURFACE ( 'NONE', #11694, 3.700000000000000178, 0.5000000000000002220 ) ;
#5398 = VERTEX_POINT ( 'NONE', #17185 ) ;
#5399 = AXIS2_PLACEMENT_3D ( 'NONE', #5725, #30999, #18345 ) ;
#5400 = CARTESIAN_POINT ( 'NONE',  ( 45.57717830316858709, 22.95310733321322161, 47.66397322663508618 ) ) ;
#5401 = EDGE_LOOP ( 'NONE', ( #10083, #925, #24751, #21289 ) ) ;
#5402 = CARTESIAN_POINT ( 'NONE',  ( -40.02540636251514172, 2.839176264122877047, 57.04930799450051637 ) ) ;
#5403 = CIRCLE ( 'NONE', #1714, 12.27641737965283575 ) ;
#5404 = CYLINDRICAL_SURFACE ( 'NONE', #22816, 12.36707279061065101 ) ;
#5405 = CARTESIAN_POINT ( 'NONE',  ( -40.50720532202722524, 7.584939507552746818, 54.64930799450051779 ) ) ;
#5406 = EDGE_CURVE ( 'NONE', #21437, #14294, #29157, .T. ) ;
#5407 = CARTESIAN_POINT ( 'NONE',  ( 44.70507715278255745, 26.96291119454915375, 46.92503878583765697 ) ) ;
#5408 = ORIENTED_EDGE ( 'NONE', *, *, #14575, .T. ) ;
#5409 = ORIENTED_EDGE ( 'NONE', *, *, #30326, .T. ) ;
#5410 = CYLINDRICAL_SURFACE ( 'NONE', #27380, 2.499999999999997335 ) ;
#5411 = VERTEX_POINT ( 'NONE', #7362 ) ;
#5412 = EDGE_CURVE ( 'NONE', #3113, #11837, #4731, .T. ) ;
#5413 = CARTESIAN_POINT ( 'NONE',  ( 21.09785597605719332, 25.56454579224779167, 21.04930799450051282 ) ) ;
#5414 = DIRECTION ( 'NONE',  ( 0.000000000000000000, -0.000000000000000000, -1.000000000000000000 ) ) ;
#5415 = CARTESIAN_POINT ( 'NONE',  ( 48.01680169312755453, 22.93807716476589675, 45.63279442905645311 ) ) ;
#5416 = DIRECTION ( 'NONE',  ( -1.101824276508909887E-16, 1.000000000000000000, -0.000000000000000000 ) ) ;
#5417 = APPLICATION_PROTOCOL_DEFINITION ( 'draft international standard', 'automotive_design', 1998, #1945 ) ;
#5418 = ORIENTED_EDGE ( 'NONE', *, *, #22376, .T. ) ;
#5419 = DIRECTION ( 'NONE',  ( 0.000000000000000000, 0.000000000000000000, 1.000000000000000000 ) ) ;
#5420 = ADVANCED_FACE ( 'NONE', ( #7687 ), #7774, .F. ) ;
#5421 = CARTESIAN_POINT ( 'NONE',  ( -40.73091736380679606, 9.483895492497154578, 38.64930799450052490 ) ) ;
#5422 = EDGE_CURVE ( 'NONE', #13542, #19007, #25076, .T. ) ;
#5423 = EDGE_CURVE ( 'NONE', #28525, #2384, #4897, .T. ) ;
#5424 = DIRECTION ( 'NONE',  ( 1.000000000000000000, 0.000000000000000000, 0.000000000000000000 ) ) ;
#5425 = AXIS2_PLACEMENT_3D ( 'NONE', #30653, #15385, #5536 ) ;
#5426 = CARTESIAN_POINT ( 'NONE',  ( 49.49063479933183629, 27.39951373492759856, 47.17357720316391578 ) ) ;
#5427 = AXIS2_PLACEMENT_3D ( 'NONE', #19961, #4876, #5043 ) ;
#5428 = ORIENTED_EDGE ( 'NONE', *, *, #23971, .F. ) ;
#5429 = DIRECTION ( 'NONE',  ( -1.101824276508909887E-16, 1.000000000000000000, -0.000000000000000000 ) ) ;
#5430 = DIRECTION ( 'NONE',  ( 1.234978253042719660E-16, -1.000000000000000000, -1.109335647967047851E-31 ) ) ;
#5431 = CARTESIAN_POINT ( 'NONE',  ( -24.94027200377598064, 13.95840365082257151, 47.04930799450052348 ) ) ;
#5432 = AXIS2_PLACEMENT_3D ( 'NONE', #24844, #7772, #29608 ) ;
#5433 = AXIS2_PLACEMENT_3D ( 'NONE', #3426, #23294, #808 ) ;
#5434 = EDGE_CURVE ( 'NONE', #5749, #31925, #14039, .T. ) ;
#5435 = ORIENTED_EDGE ( 'NONE', *, *, #12257, .F. ) ;
#5436 = ORIENTED_EDGE ( 'NONE', *, *, #29023, .T. ) ;
#5437 = CARTESIAN_POINT ( 'NONE',  ( -38.03217016322641086, -5.870668399053029951, 15.62619681354832046 ) ) ;
#5438 = CARTESIAN_POINT ( 'NONE',  ( -45.06166779280743384, -5.721341737285086992, 53.14897153969102561 ) ) ;
#5439 = DIRECTION ( 'NONE',  ( -1.101824276508909887E-16, 1.000000000000000000, -0.000000000000000000 ) ) ;
#5440 = EDGE_LOOP ( 'NONE', ( #8085, #2849, #20025, #15254 ) ) ;
#5441 = CIRCLE ( 'NONE', #8071, 0.1249999999999983763 ) ;
#5442 = CARTESIAN_POINT ( 'NONE',  ( -38.65545646816406133, 5.786704587343633577, 77.24891569812123748 ) ) ;
#5443 = DIRECTION ( 'NONE',  ( 0.000000000000000000, 0.000000000000000000, 1.000000000000000000 ) ) ;
#5444 = CYLINDRICAL_SURFACE ( 'NONE', #16363, 12.62506659569710266 ) ;
#5445 = EDGE_CURVE ( 'NONE', #26196, #10005, #17680, .T. ) ;
#5446 = FACE_BOUND ( 'NONE', #10809, .T. ) ;
#5447 = ADVANCED_FACE ( 'NONE', ( #7027 ), #23263, .T. ) ;
#5448 = LINE ( 'NONE', #15933, #25930 ) ;
#5449 = DIRECTION ( 'NONE',  ( 0.000000000000000000, 0.000000000000000000, -1.000000000000000000 ) ) ;
#5451 = CIRCLE ( 'NONE', #30080, 37.00000000000000711 ) ;
#5450 = CARTESIAN_POINT ( 'NONE',  ( -38.05567176388106532, 15.54312433976834740, 59.44930799450051495 ) ) ;
#5452 = DIRECTION ( 'NONE',  ( 0.8746197071393925215, -0.4848096202463429982, -8.676864087101708112E-18 ) ) ;
#5453 = LINE ( 'NONE', #18223, #1611 ) ;
#5454 = CIRCLE ( 'NONE', #21672, 71.99999999999998579 ) ;
#5455 = DIRECTION ( 'NONE',  ( 0.4848096202463906268, 0.8746197071393660982, 0.000000000000000000 ) ) ;
#5456 = CARTESIAN_POINT ( 'NONE',  ( 44.09250526802607340, 28.75621246473837189, 46.89322480343881949 ) ) ;
#5457 = VERTEX_POINT ( 'NONE', #929 ) ;
#5458 = ORIENTED_EDGE ( 'NONE', *, *, #31861, .F. ) ;
#5459 = CARTESIAN_POINT ( 'NONE',  ( 21.09785597605719332, 12.74140866975414887, -8.821853672795185730 ) ) ;
#5460 = CARTESIAN_POINT ( 'NONE',  ( 58.59785597605721108, 14.86454579224779948, 47.04930799450051637 ) ) ;
#5461 = EDGE_CURVE ( 'NONE', #17919, #29185, #455, .T. ) ;
#5462 = CARTESIAN_POINT ( 'NONE',  ( 33.72499318558949000, 38.56284415653841791, 47.04930799450051637 ) ) ;
#5463 = EDGE_CURVE ( 'NONE', #17607, #29601, #8013, .T. ) ;
#5464 = FACE_OUTER_BOUND ( 'NONE', #18096, .T. ) ;
#5465 = EDGE_LOOP ( 'NONE', ( #22318, #25044, #2615, #5028 ) ) ;
#5466 = CARTESIAN_POINT ( 'NONE',  ( -39.45773241730296377, -5.935454212835550969, 77.98461610899785512 ) ) ;
#5467 = CARTESIAN_POINT ( 'NONE',  ( 33.37634396954522487, 29.09164230456639899, 47.04930799450051637 ) ) ;
#5468 = CARTESIAN_POINT ( 'NONE',  ( -40.02661603751083419, 7.039661056838938613, 39.27950010995386521 ) ) ;
#5469 = ORIENTED_EDGE ( 'NONE', *, *, #16209, .T. ) ;
#5470 = ORIENTED_EDGE ( 'NONE', *, *, #31627, .F. ) ;
#5471 = DIRECTION ( 'NONE',  ( 0.6797146636928687036, 0.1949050434465272041, 0.7071067811865459074 ) ) ;
#5472 = CARTESIAN_POINT ( 'NONE',  ( 48.94625023931840246, 28.85784706826092716, 46.10640627770150246 ) ) ;
#5473 = CARTESIAN_POINT ( 'NONE',  ( 46.00908685603034343, 28.24624452788248163, 44.91496614357594552 ) ) ;
#5474 = CARTESIAN_POINT ( 'NONE',  ( 47.79865503179234310, 9.702389020015065313, -37.95069200549950494 ) ) ;
#5475 = CIRCLE ( 'NONE', #7045, 0.2000000000000004274 ) ;
#5476 = CARTESIAN_POINT ( 'NONE',  ( 21.09992658989239089, 26.34164230456639899, 47.04930799450051637 ) ) ;
#5477 = ORIENTED_EDGE ( 'NONE', *, *, #22080, .F. ) ;
#5478 = FACE_OUTER_BOUND ( 'NONE', #29296, .T. ) ;
#5479 = CYLINDRICAL_SURFACE ( 'NONE', #22820, 39.49999999999999289 ) ;
#5480 = EDGE_LOOP ( 'NONE', ( #3957, #16898, #30299, #11350 ) ) ;
#5481 = CARTESIAN_POINT ( 'NONE',  ( 21.09785597605719332, -19.93545420775220123, 47.04930799450051637 ) ) ;
#5482 = EDGE_LOOP ( 'NONE', ( #21216, #20006, #13745, #6086 ) ) ;
#5483 = DIRECTION ( 'NONE',  ( 0.000000000000000000, -1.000000000000000000, 0.000000000000000000 ) ) ;
#5484 = LINE ( 'NONE', #232, #24109 ) ;
#5485 = DIRECTION ( 'NONE',  ( 0.000000000000000000, 0.000000000000000000, -1.000000000000000000 ) ) ;
#5486 = CIRCLE ( 'NONE', #4975, 1.000000000001013856 ) ;
#5487 = VECTOR ( 'NONE', #8387, 1000.000000000000114 ) ;
#5488 = DIRECTION ( 'NONE',  ( -1.101824276508909887E-16, 1.000000000000000000, -0.000000000000000000 ) ) ;
#5489 = VECTOR ( 'NONE', #32288, 1000.000000000000114 ) ;
#5490 = DIRECTION ( 'NONE',  ( -1.101824276508909887E-16, 1.000000000000000000, -0.000000000000000000 ) ) ;
#5491 = ORIENTED_EDGE ( 'NONE', *, *, #26667, .T. ) ;
#5492 = CARTESIAN_POINT ( 'NONE',  ( 74.30208271558197453, -0.6526263882323326548, 80.46989690375676219 ) ) ;
#5493 = AXIS2_PLACEMENT_3D ( 'NONE', #21090, #21403, #23249 ) ;
#5494 = AXIS2_PLACEMENT_3D ( 'NONE', #5530, #15534, #28178 ) ;
#5495 = CARTESIAN_POINT ( 'NONE',  ( -41.56459318755936749, 7.281738416154046156, 53.54930799450051637 ) ) ;
#5496 = EDGE_CURVE ( 'NONE', #10005, #12804, #26126, .T. ) ;
#5497 = CARTESIAN_POINT ( 'NONE',  ( -42.24141723705587737, 13.63285518870473290, 54.54930799450051637 ) ) ;
#5498 = CIRCLE ( 'NONE', #21189, 1.042135311067126979 ) ;
#5499 = EDGE_CURVE ( 'NONE', #3287, #13675, #11977, .T. ) ;
#5500 = CARTESIAN_POINT ( 'NONE',  ( -40.64160980462626327, 6.824069488939680461, 39.41866629635870822 ) ) ;
#5501 = ORIENTED_EDGE ( 'NONE', *, *, #31177, .T. ) ;
#5502 = CARTESIAN_POINT ( 'NONE',  ( 21.09992658989239089, 23.59164230456639544, 47.04930799450051637 ) ) ;
#5503 = CARTESIAN_POINT ( 'NONE',  ( -41.08785830660042393, 9.277514380576530328, 35.49072935073782986 ) ) ;
#5504 = VERTEX_POINT ( 'NONE', #25400 ) ;
#5506 = CIRCLE ( 'NONE', #28840, 12.27641737965283930 ) ;
#5505 = CARTESIAN_POINT ( 'NONE',  ( 21.09785597605719332, 25.56454579224780232, -32.16074251183835031 ) ) ;
#5507 = CYLINDRICAL_SURFACE ( 'NONE', #20941, 71.99999999999998579 ) ;
#5508 = CARTESIAN_POINT ( 'NONE',  ( 48.23388202445966044, 28.92822092656773947, 49.27628909396054979 ) ) ;
#5509 = CARTESIAN_POINT ( 'NONE',  ( 54.63043436083805915, -3.866180060838560806, -9.113925348800353987 ) ) ;
#5510 = VERTEX_POINT ( 'NONE', #23421 ) ;
#5511 = CARTESIAN_POINT ( 'NONE',  ( 59.59785597605720397, 13.86454579224779948, 47.04930799450051637 ) ) ;
#5512 = VERTEX_POINT ( 'NONE', #27870 ) ;
#5513 = ORIENTED_EDGE ( 'NONE', *, *, #19632, .T. ) ;
#5514 = AXIS2_PLACEMENT_3D ( 'NONE', #4916, #29868, #12638 ) ;
#5515 = AXIS2_PLACEMENT_3D ( 'NONE', #28903, #26586, #19354 ) ;
#5516 = CIRCLE ( 'NONE', #29623, 55.85791022362053582 ) ;
#5517 = CIRCLE ( 'NONE', #25933, 72.21005050633880273 ) ;
#5518 = DIRECTION ( 'NONE',  ( -1.101824276508909887E-16, 1.000000000000000000, -0.000000000000000000 ) ) ;
#5519 = DIRECTION ( 'NONE',  ( -0.000000000000000000, -1.000000000000000000, 0.000000000000000000 ) ) ;
#5520 = DIRECTION ( 'NONE',  ( 3.629881133195132442E-17, 0.9550631830612811290, -0.2964022880492887535 ) ) ;
#5521 = ORIENTED_EDGE ( 'NONE', *, *, #329, .T. ) ;
#5522 = ORIENTED_EDGE ( 'NONE', *, *, #16961, .F. ) ;
#5523 = CARTESIAN_POINT ( 'NONE',  ( 45.69268131687783807, 22.99884124225578574, 46.97633003370108185 ) ) ;
#5524 = CARTESIAN_POINT ( 'NONE',  ( 21.09785597605719332, 13.74476430820393347, 47.04930799450051637 ) ) ;
#5525 = CARTESIAN_POINT ( 'NONE',  ( -30.33962712718416910, 8.338190197707957552, 75.22269307782707415 ) ) ;
#5526 = DIRECTION ( 'NONE',  ( -1.101824276508909887E-16, 1.000000000000000000, -0.000000000000000000 ) ) ;
#5527 = VERTEX_POINT ( 'NONE', #10957 ) ;
#5528 = FACE_OUTER_BOUND ( 'NONE', #11715, .T. ) ;
#5529 = ORIENTED_EDGE ( 'NONE', *, *, #6400, .T. ) ;
#5530 = CARTESIAN_POINT ( 'NONE',  ( 106.0978559760575735, 11.92558985988973497, 26.63511333407112858 ) ) ;
#5531 = DIRECTION ( 'NONE',  ( 0.000000000000000000, 3.761114140369702165E-15, -1.000000000000000000 ) ) ;
#5532 = ORIENTED_EDGE ( 'NONE', *, *, #13948, .F. ) ;
#5533 = EDGE_CURVE ( 'NONE', #15187, #28369, #30338, .T. ) ;
#5534 = CARTESIAN_POINT ( 'NONE',  ( 21.09992658989239089, 30.46664230456641675, 47.04930799450051637 ) ) ;
#5535 = DIRECTION ( 'NONE',  ( -1.000000000000000000, -1.101824276508909887E-16, 0.000000000000000000 ) ) ;
#5536 = DIRECTION ( 'NONE',  ( -1.000000000000000000, 0.000000000000000000, 0.000000000000000000 ) ) ;
#5537 = EDGE_CURVE ( 'NONE', #1639, #1830, #12940, .T. ) ;
#5538 = EDGE_CURVE ( 'NONE', #22139, #19299, #11457, .T. ) ;
#5539 = DIRECTION ( 'NONE',  ( 1.234978253042719660E-16, -1.000000000000000000, -1.109335647967047851E-31 ) ) ;
#5540 = AXIS2_PLACEMENT_3D ( 'NONE', #10007, #29374, #24939 ) ;
#5541 = ADVANCED_FACE ( 'NONE', ( #13102 ), #4647, .F. ) ;
#5542 =( BOUNDED_CURVE ( )  B_SPLINE_CURVE ( 2, ( #983, #28406, #28564, #18689, #1301, #11007, #11325, #30711, #28716 ),
 .UNSPECIFIED., .F., .F. ) 
 B_SPLINE_CURVE_WITH_KNOTS ( ( 3, 2, 2, 2, 3 ),
 ( 0.7500000011612726336, 0.7619047619047618625, 0.7857142857142856984, 0.8095238095238095344, 0.8214285725898440305 ),
 .UNSPECIFIED. ) 
 CURVE ( )  GEOMETRIC_REPRESENTATION_ITEM ( )  RATIONAL_B_SPLINE_CURVE ( ( 0.9330127018922200755, 0.9330127084266227611, 1.000000000000000000, 0.8660254037844388186, 1.000000000000000000, 0.8660254037844388186, 1.000000000000000000, 0.9330126953578163906, 0.9330127018922200755 ) ) 
 REPRESENTATION_ITEM ( '' )  );
#5543 = DIRECTION ( 'NONE',  ( -1.101824276508909887E-16, 1.000000000000000000, -0.000000000000000000 ) ) ;
#5544 = DIRECTION ( 'NONE',  ( -1.000000000000000000, 0.000000000000000000, 0.000000000000000000 ) ) ;
#5545 = ADVANCED_FACE ( 'NONE', ( #10312 ), #8832, .T. ) ;
#5546 = AXIS2_PLACEMENT_3D ( 'NONE', #20501, #5414, #30361 ) ;
#5547 = ADVANCED_FACE ( 'NONE', ( #15546 ), #2755, .F. ) ;
#5548 = ORIENTED_EDGE ( 'NONE', *, *, #2347, .T. ) ;
#5549 = DIRECTION ( 'NONE',  ( -1.101824276508909887E-16, 1.000000000000000000, -0.000000000000000000 ) ) ;
#5550 = TOROIDAL_SURFACE ( 'NONE', #32277, 38.50000000000000000, 1.499999999999997780 ) ;
#5551 = AXIS2_PLACEMENT_3D ( 'NONE', #15171, #25183, #18424 ) ;
#5552 = CARTESIAN_POINT ( 'NONE',  ( 48.23388202445966044, 28.35087065737811685, 49.27628909396054979 ) ) ;
#5553 = ORIENTED_EDGE ( 'NONE', *, *, #11012, .T. ) ;
#5554 = VERTEX_POINT ( 'NONE', #10802 ) ;
#5555 = DIRECTION ( 'NONE',  ( -1.000000000000000000, 0.000000000000000000, 0.000000000000000000 ) ) ;
#5556 = CIRCLE ( 'NONE', #13940, 12.36707279061065279 ) ;
#5557 = ORIENTED_EDGE ( 'NONE', *, *, #22197, .F. ) ;
#5558 = EDGE_LOOP ( 'NONE', ( #31240, #31024, #30960, #3341 ) ) ;
#5559 = DIRECTION ( 'NONE',  ( -1.101824276508909887E-16, 1.000000000000000000, -0.000000000000000000 ) ) ;
#5560 = ADVANCED_FACE ( 'NONE', ( #22769 ), #27175, .T. ) ;
#5561 = AXIS2_PLACEMENT_3D ( 'NONE', #22646, #19690, #25279 ) ;
#5562 = EDGE_LOOP ( 'NONE', ( #8864, #8703, #24882 ) ) ;
#5563 = CARTESIAN_POINT ( 'NONE',  ( 48.76626135000090301, 22.93328494799376216, 47.45974698848920781 ) ) ;
#5564 = CYLINDRICAL_SURFACE ( 'NONE', #12753, 12.62506659569710266 ) ;
#5565 = CARTESIAN_POINT ( 'NONE',  ( 48.80717017713595141, 27.27622849631043067, 48.15820438821415195 ) ) ;
#5566 = EDGE_LOOP ( 'NONE', ( #896, #10859, #27346, #8860 ) ) ;
#5567 = EDGE_LOOP ( 'NONE', ( #8351, #15622, #32252, #22472 ) ) ;
#5568 = LINE ( 'NONE', #22797, #11656 ) ;
#5569 = VERTEX_POINT ( 'NONE', #8170 ) ;
#5570 = AXIS2_PLACEMENT_3D ( 'NONE', #32407, #7466, #7131 ) ;
#5571 = DIRECTION ( 'NONE',  ( 0.000000000000000000, -0.000000000000000000, -1.000000000000000000 ) ) ;
#5572 = DIRECTION ( 'NONE',  ( -0.000000000000000000, -1.000000000000000000, 0.000000000000000000 ) ) ;
#5573 = CARTESIAN_POINT ( 'NONE',  ( -40.59581018552366061, 9.375516295340284856, 39.44930799450052206 ) ) ;
#5574 = EDGE_CURVE ( 'NONE', #23509, #116, #4092, .T. ) ;
#5575 = CARTESIAN_POINT ( 'NONE',  ( 47.74496780842034127, 22.93328494799376571, 45.45767897490919296 ) ) ;
#5576 = CARTESIAN_POINT ( 'NONE',  ( 48.94625023931840246, 25.27124452788249442, 46.10640627770148825 ) ) ;
#5577 = EDGE_CURVE ( 'NONE', #11769, #22362, #3067, .T. ) ;
#5578 = ORIENTED_EDGE ( 'NONE', *, *, #3518, .T. ) ;
#5579 = CARTESIAN_POINT ( 'NONE',  ( -41.06741244844305783, 5.703477804968248854, 47.04930799450051637 ) ) ;
#5580 = FACE_OUTER_BOUND ( 'NONE', #22644, .T. ) ;
#5581 = CARTESIAN_POINT ( 'NONE',  ( -9.794785901691708929, -5.936920032134867853, 107.5052597691543070 ) ) ;
#5582 = CARTESIAN_POINT ( 'NONE',  ( 45.35708200440645044, 26.29118040159426428, 45.92000246470680480 ) ) ;
#5583 = ORIENTED_EDGE ( 'NONE', *, *, #11807, .T. ) ;
#5584 = CARTESIAN_POINT ( 'NONE',  ( 21.09992658989239089, 26.71183152705960495, 47.04930799450051637 ) ) ;
#5585 = FACE_OUTER_BOUND ( 'NONE', #25051, .T. ) ;
#5586 = AXIS2_PLACEMENT_3D ( 'NONE', #24257, #4243, #14260 ) ;
#5587 = LINE ( 'NONE', #12982, #14425 ) ;
#5588 = EDGE_LOOP ( 'NONE', ( #13571, #3053, #16681, #28901 ) ) ;
#5589 = EDGE_CURVE ( 'NONE', #20520, #8606, #10416, .T. ) ;
#5590 = VECTOR ( 'NONE', #7085, 1000.000000000000000 ) ;
#5591 = ORIENTED_EDGE ( 'NONE', *, *, #18031, .F. ) ;
#5592 = ORIENTED_EDGE ( 'NONE', *, *, #28913, .F. ) ;
#5593 = PLANE ( 'NONE',  #12869 ) ;
#5594 = EDGE_CURVE ( 'NONE', #21972, #30111, #6211, .T. ) ;
#5595 = CARTESIAN_POINT ( 'NONE',  ( 8.823509210239555145, 28.84164230456639544, 47.04930799450051637 ) ) ;
#5596 = DIRECTION ( 'NONE',  ( -1.000000000000000000, 0.000000000000000000, 0.000000000000000000 ) ) ;
#5597 = EDGE_CURVE ( 'NONE', #29666, #5958, #15880, .T. ) ;
#5598 = ORIENTED_EDGE ( 'NONE', *, *, #14122, .F. ) ;
#5599 = CARTESIAN_POINT ( 'NONE',  ( -29.27613032885505007, 11.23353054871637013, 71.85461326257689052 ) ) ;
#5600 = LINE ( 'NONE', #21814, #25417 ) ;
#5601 = CARTESIAN_POINT ( 'NONE',  ( 8.474859994195282908, 38.56284415653841791, 47.04930799450051637 ) ) ;
#5602 = CIRCLE ( 'NONE', #25536, 34.00000000000000000 ) ;
#5603 = DIRECTION ( 'NONE',  ( 0.000000000000000000, 0.000000000000000000, 1.000000000000000000 ) ) ;
#5604 = CARTESIAN_POINT ( 'NONE',  ( 45.00053793792376666, 27.35920399681022630, 45.68869892245983522 ) ) ;
#5605 = CARTESIAN_POINT ( 'NONE',  ( 44.79156314060809763, 22.86454579224779948, 46.92953032342012420 ) ) ;
#5606 = CARTESIAN_POINT ( 'NONE',  ( 21.09785597605719332, 25.56454579224779877, 47.04930799450051637 ) ) ;
#5607 = CARTESIAN_POINT ( 'NONE',  ( -42.12525683681430877, 14.70933063813549424, 38.19144330556764544 ) ) ;
#5608 = FACE_OUTER_BOUND ( 'NONE', #24785, .T. ) ;
#5609 = CARTESIAN_POINT ( 'NONE',  ( 21.09992658989239089, 30.09164230456639544, 47.04930799450051637 ) ) ;
#5610 = CARTESIAN_POINT ( 'NONE',  ( 46.96268396749378127, 28.93121246473836905, 49.65201805493727960 ) ) ;
#5611 = EDGE_CURVE ( 'NONE', #30781, #6259, #3344, .T. ) ;
#5612 = EDGE_LOOP ( 'NONE', ( #12655, #6042 ) ) ;
#5613 = ORIENTED_EDGE ( 'NONE', *, *, #5116, .T. ) ;
#5614 = CARTESIAN_POINT ( 'NONE',  ( 33.50134396954521776, 29.59164230456639899, 47.04930799450051637 ) ) ;
#5615 = CARTESIAN_POINT ( 'NONE',  ( 49.03322279537384532, 25.03300763406332408, 45.41163724378073852 ) ) ;
#5616 = DIRECTION ( 'NONE',  ( 0.8746197071393925215, -0.4848096202463429982, -8.676864087101709653E-18 ) ) ;
#5617 = ORIENTED_EDGE ( 'NONE', *, *, #23857, .T. ) ;
#5618 = CARTESIAN_POINT ( 'NONE',  ( -5.602943079677954685, 9.702389020015065313, -3.412202488244239884 ) ) ;
#5619 = CARTESIAN_POINT ( 'NONE',  ( -40.01477201457414878, 7.207664580857849224, 39.00001346453329631 ) ) ;
#5620 = ORIENTED_EDGE ( 'NONE', *, *, #5187, .F. ) ;
#5621 = ORIENTED_EDGE ( 'NONE', *, *, #3518, .F. ) ;
#5622 = LINE ( 'NONE', #15471, #1065 ) ;
#5623 = CARTESIAN_POINT ( 'NONE',  ( 49.49063479933183629, 28.79951373492759359, 47.17357720316391578 ) ) ;
#5624 = B_SPLINE_CURVE_WITH_KNOTS ( 'NONE', 3,
 ( #20355, #30384, #668, #12992, #27922, #28245 ),
 .UNSPECIFIED., .F., .F.,
 ( 4, 2, 4 ),
 ( 0.000000000000000000, 0.5000000000000000000, 1.000000000000000000 ),
 .UNSPECIFIED. ) ;
#5625 = CARTESIAN_POINT ( 'NONE',  ( 46.99023568444673060, 28.53791119454914949, 49.12151524109405898 ) ) ;
#5626 = CARTESIAN_POINT ( 'NONE',  ( 46.04844006429464542, 22.86454579224779948, 44.99211097489548905 ) ) ;
#5627 = ADVANCED_FACE ( 'NONE', ( #3879 ), #26362, .T. ) ;
#5628 = AXIS2_PLACEMENT_3D ( 'NONE', #31372, #6909, #11677 ) ;
#5629 = ADVANCED_FACE ( 'NONE', ( #26197 ), #26683, .T. ) ;
#5630 = VERTEX_POINT ( 'NONE', #14224 ) ;
#5631 = AXIS2_PLACEMENT_3D ( 'NONE', #31091, #5823, #28619 ) ;
#5632 = CARTESIAN_POINT ( 'NONE',  ( 33.46699938050304013, 27.21183152705960495, 47.04930799450051637 ) ) ;
#5633 = DIRECTION ( 'NONE',  ( -1.000000000000000000, 0.000000000000000000, 0.000000000000000000 ) ) ;
#5634 = EDGE_CURVE ( 'NONE', #25363, #26371, #23899, .T. ) ;
#5635 = ORIENTED_EDGE ( 'NONE', *, *, #27109, .F. ) ;
#5636 = ADVANCED_FACE ( 'NONE', ( #19282 ), #12508, .T. ) ;
#5637 = CARTESIAN_POINT ( 'NONE',  ( 79.18332612743283505, -5.935454207752198563, 77.87546120947918382 ) ) ;
#5638 = DIRECTION ( 'NONE',  ( -0.8746197071393805311, 0.4848096202463645921, 1.277302113040265530E-17 ) ) ;
#5639 = CARTESIAN_POINT ( 'NONE',  ( 76.48178494842512976, -4.032327822094600833, 13.59507165472702894 ) ) ;
#5640 = ORIENTED_EDGE ( 'NONE', *, *, #1706, .T. ) ;
#5641 = DIRECTION ( 'NONE',  ( 0.8746197071393925215, -0.4848096202463429982, -8.676864087101708112E-18 ) ) ;
#5642 = DIRECTION ( 'NONE',  ( -1.224646799147353207E-16, -1.349345573449484691E-32, 1.000000000000000000 ) ) ;
#5643 = CARTESIAN_POINT ( 'NONE',  ( -40.11286833322907341, 2.887657226147507306, 37.04930799450052348 ) ) ;
#5644 = LINE ( 'NONE', #17954, #17598 ) ;
#5645 = ORIENTED_EDGE ( 'NONE', *, *, #26692, .F. ) ;
#5646 = FACE_OUTER_BOUND ( 'NONE', #24588, .T. ) ;
#5648 = FACE_OUTER_BOUND ( 'NONE', #11106, .T. ) ;
#5647 = AXIS2_PLACEMENT_3D ( 'NONE', #5785, #23339, #15793 ) ;
#5649 = AXIS2_PLACEMENT_3D ( 'NONE', #8838, #8361, #18358 ) ;
#5650 = FACE_OUTER_BOUND ( 'NONE', #14035, .T. ) ;
#5651 = DIRECTION ( 'NONE',  ( -0.000000000000000000, -1.000000000000000000, 0.000000000000000000 ) ) ;
#5652 = CARTESIAN_POINT ( 'NONE',  ( -40.64500813507293486, 6.819128862114092193, 39.51928662074344345 ) ) ;
#5653 = VERTEX_POINT ( 'NONE', #16029 ) ;
#5654 = DIRECTION ( 'NONE',  ( -0.000000000000000000, -1.000000000000000000, -0.000000000000000000 ) ) ;
#5655 = CARTESIAN_POINT ( 'NONE',  ( 49.73127130660545703, 24.88724468661089873, 46.52306240693558692 ) ) ;
#5656 = DIRECTION ( 'NONE',  ( 1.234978253042719660E-16, -1.000000000000000000, -1.109335647967047851E-31 ) ) ;
#5657 = CIRCLE ( 'NONE', #16641, 0.1000000000000028644 ) ;
#5658 = VERTEX_POINT ( 'NONE', #8796 ) ;
#5659 = CARTESIAN_POINT ( 'NONE',  ( 21.09992658989239089, 27.84143805560860940, 47.04930799450051637 ) ) ;
#5660 = CARTESIAN_POINT ( 'NONE',  ( 21.09785597605719332, 11.78014697381582643, 47.04930799450051637 ) ) ;
#5661 = FACE_OUTER_BOUND ( 'NONE', #23654, .T. ) ;
#5662 = AXIS2_PLACEMENT_3D ( 'NONE', #3001, #29780, #19920 ) ;
#5663 = DIRECTION ( 'NONE',  ( -1.101824276508909887E-16, 1.000000000000000000, -0.000000000000000000 ) ) ;
#5664 = VERTEX_POINT ( 'NONE', #11121 ) ;
#5665 = B_SPLINE_SURFACE_WITH_KNOTS ( 'NONE', 3, 1, ( 
 ( #23593, #13114 ),
 ( #6043, #8337 ),
 ( #20960, #13590 ),
 ( #11134, #3407 ),
 ( #25573, #6192 ),
 ( #8029, #10488 ) ),
 .UNSPECIFIED., .F., .F., .F.,
 ( 4, 1, 1, 4 ),
 ( 2, 2 ),
 ( 0.1800733115436725096, 0.4989925988945991819, 0.7849997004460342875, 1.000000000000000000 ),
 ( 0.000000000000000000, 1.000000000000000000 ),
 .UNSPECIFIED. ) ;
#5666 = DIRECTION ( 'NONE',  ( -1.101824276508909887E-16, 1.000000000000000000, -0.000000000000000000 ) ) ;
#5667 = VERTEX_POINT ( 'NONE', #26035 ) ;
#5668 = EDGE_CURVE ( 'NONE', #10579, #10718, #28829, .T. ) ;
#5669 = EDGE_CURVE ( 'NONE', #4920, #5411, #1411, .T. ) ;
#5670 = EDGE_LOOP ( 'NONE', ( #9048, #26323, #27618, #15172 ) ) ;
#5671 = AXIS2_PLACEMENT_3D ( 'NONE', #13463, #20830, #5910 ) ;
#5672 = AXIS2_PLACEMENT_3D ( 'NONE', #9629, #22745, #29655 ) ;
#5673 = EDGE_CURVE ( 'NONE', #25118, #9995, #16669, .T. ) ;
#5674 = AXIS2_PLACEMENT_3D ( 'NONE', #2977, #15615, #22688 ) ;
#5675 = AXIS2_PLACEMENT_3D ( 'NONE', #31459, #16183, #11424 ) ;
#5676 = FACE_OUTER_BOUND ( 'NONE', #7663, .T. ) ;
#5677 = CARTESIAN_POINT ( 'NONE',  ( 21.09785597605719332, 38.31023907818019580, 47.04930799450051637 ) ) ;
#5678 = DIRECTION ( 'NONE',  ( 0.000000000000000000, 0.000000000000000000, -1.000000000000000000 ) ) ;
#5679 = EDGE_LOOP ( 'NONE', ( #15652, #29644, #14384, #17961 ) ) ;
#5680 = AXIS2_PLACEMENT_3D ( 'NONE', #19550, #24157, #27105 ) ;
#5681 = DIRECTION ( 'NONE',  ( 0.9612616959383202264, 0.2756373558169946114, -1.699334552409296294E-15 ) ) ;
#5682 = ORIENTED_EDGE ( 'NONE', *, *, #18204, .T. ) ;
#5683 = DIRECTION ( 'NONE',  ( -1.101824276508909887E-16, 1.000000000000000000, -0.000000000000000000 ) ) ;
#5684 = CYLINDRICAL_SURFACE ( 'NONE', #7050, 2.749999999999998224 ) ;
#5685 = DIRECTION ( 'NONE',  ( -1.000000000000000000, 0.000000000000000000, 0.000000000000000000 ) ) ;
#5686 = DIRECTION ( 'NONE',  ( -1.000000000000000000, 0.000000000000000000, 0.000000000000000000 ) ) ;
#5687 = VERTEX_POINT ( 'NONE', #8651 ) ;
#5688 = DIRECTION ( 'NONE',  ( 0.000000000000000000, -1.000000000000000000, 0.000000000000000000 ) ) ;
#5689 = ORIENTED_EDGE ( 'NONE', *, *, #22934, .F. ) ;
#5690 = CARTESIAN_POINT ( 'NONE',  ( -40.47970302497625994, 7.463434137431151250, 53.64930799450051779 ) ) ;
#5691 = CARTESIAN_POINT ( 'NONE',  ( 21.09785597605720042, -16.03545420775220265, 47.04930799450051637 ) ) ;
#5692 = VERTEX_POINT ( 'NONE', #11274 ) ;
#5693 = DIRECTION ( 'NONE',  ( -0.9862637841664568805, -0.1651779284337366038, 0.000000000000000000 ) ) ;
#5694 = DIRECTION ( 'NONE',  ( -1.101824276508909887E-16, 1.000000000000000000, -0.000000000000000000 ) ) ;
#5695 = DIRECTION ( 'NONE',  ( -0.8746197071393925215, 0.4848096202463429982, 8.676864087101708112E-18 ) ) ;
#5696 = CARTESIAN_POINT ( 'NONE',  ( 73.09176707068564838, 11.92558985988973497, 67.46350265493038023 ) ) ;
#5697 = PRESENTATION_STYLE_ASSIGNMENT (( #28185 ) ) ;
#5698 = LINE ( 'NONE', #11118, #2710 ) ;
#5699 = CARTESIAN_POINT ( 'NONE',  ( -40.11286833322908052, 2.887657226147509970, 58.24930799450051921 ) ) ;
#5700 = ORIENTED_EDGE ( 'NONE', *, *, #24671, .F. ) ;
#5701 = CARTESIAN_POINT ( 'NONE',  ( 21.09785597605719332, 7.881678200673685630, 47.04930799450051637 ) ) ;
#5702 = TOROIDAL_SURFACE ( 'NONE', #9892, 12.61792373059898686, 0.1249999999999964195 ) ;
#5703 = AXIS2_PLACEMENT_3D ( 'NONE', #8366, #18363, #15916 ) ;
#5704 = CARTESIAN_POINT ( 'NONE',  ( -9.880269303432738681, -5.935454207752202116, -13.57859485750651629 ) ) ;
#5705 = AXIS2_PLACEMENT_3D ( 'NONE', #26437, #21495, #29720 ) ;
#5706 = ORIENTED_EDGE ( 'NONE', *, *, #22038, .F. ) ;
#5707 = AXIS2_PLACEMENT_3D ( 'NONE', #12412, #22398, #1898 ) ;
#5708 = ORIENTED_EDGE ( 'NONE', *, *, #15601, .F. ) ;
#5709 = DIRECTION ( 'NONE',  ( -1.000000000000000000, 0.000000000000000000, 0.000000000000000000 ) ) ;
#5710 = CIRCLE ( 'NONE', #14100, 0.1000000000000027811 ) ;
#5711 = ORIENTED_EDGE ( 'NONE', *, *, #8662, .F. ) ;
#5712 = EDGE_CURVE ( 'NONE', #607, #1905, #18957, .T. ) ;
#5713 = ADVANCED_FACE ( 'NONE', ( #1568 ), #7281, .T. ) ;
#5714 = EDGE_CURVE ( 'NONE', #20563, #6650, #8966, .T. ) ;
#5715 = ADVANCED_FACE ( 'NONE', ( #19119 ), #28222, .T. ) ;
#5716 = ORIENTED_EDGE ( 'NONE', *, *, #22671, .F. ) ;
#5717 = CARTESIAN_POINT ( 'NONE',  ( 8.823509210239507183, 24.09164230456639544, 47.04930799450051637 ) ) ;
#5718 = ADVANCED_FACE ( 'NONE', ( #6666 ), #25037, .T. ) ;
#5719 =( GEOMETRIC_REPRESENTATION_CONTEXT ( 3 ) GLOBAL_UNCERTAINTY_ASSIGNED_CONTEXT ( ( #13746 ) ) GLOBAL_UNIT_ASSIGNED_CONTEXT ( ( #18023, #22455, #7867 ) ) REPRESENTATION_CONTEXT ( 'NONE', 'WORKASPACE' ) );
#5720 = VECTOR ( 'NONE', #9092, 1000.000000000000000 ) ;
#5721 = ORIENTED_EDGE ( 'NONE', *, *, #10847, .T. ) ;
#5722 = CARTESIAN_POINT ( 'NONE',  ( 48.49492103495406070, 22.99884124225578574, 47.27843453342132563 ) ) ;
#5723 = SHAPE_REPRESENTATION ( 'Screw M5', ( #8172 ), #22330 ) ;
#5724 = CARTESIAN_POINT ( 'NONE',  ( 48.23388214087538728, 15.77906836436399374, 49.27628903457465270 ) ) ;
#5725 = CARTESIAN_POINT ( 'NONE',  ( 21.09785597605719332, 25.56454579224779877, 47.04930799450051637 ) ) ;
#5726 = CARTESIAN_POINT ( 'NONE',  ( 46.02876340639226527, 25.46789516297710065, 44.95353858666495483 ) ) ;
#5727 = ORIENTED_EDGE ( 'NONE', *, *, #27675, .F. ) ;
#5728 = ORIENTED_EDGE ( 'NONE', *, *, #18773, .F. ) ;
#5729 = PRESENTATION_STYLE_ASSIGNMENT (( #13295 ) ) ;
#5730 = ORIENTED_EDGE ( 'NONE', *, *, #15663, .F. ) ;
#5731 = CIRCLE ( 'NONE', #474, 12.36707279061065101 ) ;
#5732 = CARTESIAN_POINT ( 'NONE',  ( 47.79865503179234310, 9.702389020015065313, 98.41455612196619995 ) ) ;
#5733 = CARTESIAN_POINT ( 'NONE',  ( 54.76993271253332551, -1.761407059904337880, 101.7633224016298925 ) ) ;
#5734 = LINE ( 'NONE', #13299, #4359 ) ;
#5735 = AXIS2_PLACEMENT_3D ( 'NONE', #13465, #1453, #15915 ) ;
#5736 = CARTESIAN_POINT ( 'NONE',  ( 21.09785597605719332, 44.99492099041257376, 47.04930799450051637 ) ) ;
#5737 = DIRECTION ( 'NONE',  ( -0.000000000000000000, -1.000000000000000000, 0.000000000000000000 ) ) ;
#5738 = CONTEXT_DEPENDENT_SHAPE_REPRESENTATION ( #16417, #12213 ) ;
#5739 = EDGE_LOOP ( 'NONE', ( #12672, #1802, #27125, #14542, #7934, #7788, #29464, #23905 ) ) ;
#5740 = DIRECTION ( 'NONE',  ( 2.779292025043186357E-18, -1.288349127009862211E-17, 1.000000000000000000 ) ) ;
#5741 = CARTESIAN_POINT ( 'NONE',  ( 21.09785597605719332, 43.75535478762431296, 47.04930799450051637 ) ) ;
#5742 = CARTESIAN_POINT ( 'NONE',  ( 21.09992658989238734, 32.59164230456639899, 47.04930799450051637 ) ) ;
#5743 = DIRECTION ( 'NONE',  ( 0.2756373558169954441, -0.9612616959383198934, 5.348665517716782531E-31 ) ) ;
#5744 = ORIENTED_EDGE ( 'NONE', *, *, #20077, .F. ) ;
#5745 = CARTESIAN_POINT ( 'NONE',  ( -42.26497471389478733, 14.66834543456875117, 59.01654570186344984 ) ) ;
#5746 = EDGE_CURVE ( 'NONE', #13269, #11793, #2548, .T. ) ;
#5747 = CIRCLE ( 'NONE', #488, 0.1250000000000001110 ) ;
#5748 = VECTOR ( 'NONE', #3998, 1000.000000000000000 ) ;
#5749 = VERTEX_POINT ( 'NONE', #29642 ) ;
#5750 = AXIS2_PLACEMENT_3D ( 'NONE', #18917, #26639, #14181 ) ;
#5751 = VECTOR ( 'NONE', #14510, 1000.000000000000000 ) ;
#5752 = ORIENTED_EDGE ( 'NONE', *, *, #1626, .T. ) ;
#5753 = EDGE_CURVE ( 'NONE', #7619, #6508, #4365, .T. ) ;
#5754 = EDGE_CURVE ( 'NONE', #10875, #12313, #12083, .T. ) ;
#5755 = EDGE_CURVE ( 'NONE', #25242, #27840, #6723, .T. ) ;
#5756 = AXIS2_PLACEMENT_3D ( 'NONE', #24590, #2276, #22124 ) ;
#5757 = ORIENTED_EDGE ( 'NONE', *, *, #12585, .T. ) ;
#5758 = ADVANCED_FACE ( 'NONE', ( #14872 ), #24879, .F. ) ;
#5759 = DIRECTION ( 'NONE',  ( 0.7141240004913198547, -0.3958453973320100738, -0.5773502691896283956 ) ) ;
#5760 = CIRCLE ( 'NONE', #17816, 16.00569570871410008 ) ;
#5761 = EDGE_CURVE ( 'NONE', #22214, #3389, #31894, .T. ) ;
#5762 = CARTESIAN_POINT ( 'NONE',  ( 21.09785597605720042, 14.56957104541719694, 101.5543332476699305 ) ) ;
#5763 = ORIENTED_EDGE ( 'NONE', *, *, #28355, .T. ) ;
#5764 = CYLINDRICAL_SURFACE ( 'NONE', #448, 2.500000000000002220 ) ;
#5765 = CARTESIAN_POINT ( 'NONE',  ( 81.56333945993378620, -5.935454207834600204, 15.93786612339379083 ) ) ;
#5766 = CARTESIAN_POINT ( 'NONE',  ( 21.09785597605719332, 11.92558985988973497, 47.04930799450051637 ) ) ;
#5767 = CARTESIAN_POINT ( 'NONE',  ( 21.09992658989239089, 28.84164230456639544, 47.04930799450051637 ) ) ;
#5768 = AXIS2_PLACEMENT_3D ( 'NONE', #26507, #11577, #24364 ) ;
#5769 = CIRCLE ( 'NONE', #9956, 12.51969897791880015 ) ;
#5770 = CARTESIAN_POINT ( 'NONE',  ( -41.95414548415062228, 13.78332541096821373, 59.54930799450050927 ) ) ;
#5771 = CARTESIAN_POINT ( 'NONE',  ( 21.09785597605719332, -13.49020584019834601, -11.04286022428629188 ) ) ;
#5772 = CARTESIAN_POINT ( 'NONE',  ( -39.58809650894544774, 2.596771453999702661, 47.04930799450051637 ) ) ;
#5773 = DIRECTION ( 'NONE',  ( -1.101824276508909887E-16, 1.000000000000000000, -0.000000000000000000 ) ) ;
#5774 = CARTESIAN_POINT ( 'NONE',  ( -40.69224796978070202, 6.791021494070471398, 34.63467695428018800 ) ) ;
#5775 = DIRECTION ( 'NONE',  ( 0.000000000000000000, 0.000000000000000000, -1.000000000000000000 ) ) ;
#5776 =( LENGTH_UNIT ( ) NAMED_UNIT ( * ) SI_UNIT ( .MILLI., .METRE. ) );
#5777 = ORIENTED_EDGE ( 'NONE', *, *, #20000, .T. ) ;
#5778 = ORIENTED_EDGE ( 'NONE', *, *, #33, .T. ) ;
#5779 = CARTESIAN_POINT ( 'NONE',  ( 63.14652337230385371, -13.30632128221581389, 83.93193429851626775 ) ) ;
#5780 = LINE ( 'NONE', #8562, #22454 ) ;
#5781 = CIRCLE ( 'NONE', #25691, 0.1250000000000001110 ) ;
#5782 = AXIS2_PLACEMENT_3D ( 'NONE', #31194, #13632, #21809 ) ;
#5783 = DIRECTION ( 'NONE',  ( -1.000000000000000000, -1.101824276508909887E-16, 0.000000000000000000 ) ) ;
#5784 = ORIENTED_EDGE ( 'NONE', *, *, #19854, .T. ) ;
#5785 = CARTESIAN_POINT ( 'NONE',  ( 21.09992658989238734, 38.56284415653841791, 47.04930799450051637 ) ) ;
#5786 = CIRCLE ( 'NONE', #4208, 19.50000000000000000 ) ;
#5787 = CARTESIAN_POINT ( 'NONE',  ( -40.23847960489091236, 6.935107575317840833, 39.54930799450052348 ) ) ;
#5788 = ORIENTED_EDGE ( 'NONE', *, *, #11673, .F. ) ;
#5789 = CARTESIAN_POINT ( 'NONE',  ( 21.09785597605719687, 30.56454579224779522, 14.54930799450051460 ) ) ;
#5790 = AXIS2_PLACEMENT_3D ( 'NONE', #9450, #31931, #4518 ) ;
#5791 = CARTESIAN_POINT ( 'NONE',  ( 44.70507715278255745, 28.44951373492759217, 46.92503878583765697 ) ) ;
#5792 = TOROIDAL_SURFACE ( 'NONE', #30436, 1.899999999999999467, 0.1000000000000000056 ) ;
#5793 = EDGE_CURVE ( 'NONE', #28202, #6910, #19295, .T. ) ;
#5794 = ADVANCED_FACE ( 'NONE', ( #24379 ), #17731, .T. ) ;
#5795 = CARTESIAN_POINT ( 'NONE',  ( 48.40186567930498285, 28.12957786121581805, 45.03923535223908203 ) ) ;
#5796 = CARTESIAN_POINT ( 'NONE',  ( -39.39899823193098172, -5.936009779471990377, 77.95343643848875104 ) ) ;
#5797 = AXIS2_PLACEMENT_3D ( 'NONE', #22347, #17260, #7434 ) ;
#5798 = ORIENTED_EDGE ( 'NONE', *, *, #10542, .T. ) ;
#5799 = EDGE_CURVE ( 'NONE', #4386, #30985, #22529, .T. ) ;
#5800 = FACE_OUTER_BOUND ( 'NONE', #25926, .T. ) ;
#5801 = CARTESIAN_POINT ( 'NONE',  ( -15.90214402394279958, -5.098646251524523443, 47.04930799450052348 ) ) ;
#5802 = CIRCLE ( 'NONE', #28343, 0.2551199516247883436 ) ;
#5803 = AXIS2_PLACEMENT_3D ( 'NONE', #26352, #21580, #31451 ) ;
#5804 = ORIENTED_EDGE ( 'NONE', *, *, #26569, .T. ) ;
#5805 = CIRCLE ( 'NONE', #27803, 0.1250000000000001110 ) ;
#5806 = DIRECTION ( 'NONE',  ( 0.000000000000000000, 0.000000000000000000, -1.000000000000000000 ) ) ;
#5807 = CARTESIAN_POINT ( 'NONE',  ( -43.64073206722599707, 1.267352857069779848, 39.44930799450052916 ) ) ;
#5808 = TOROIDAL_SURFACE ( 'NONE', #7376, 12.40141737965288726, 0.1250000000000003331 ) ;
#5809 = AXIS2_PLACEMENT_3D ( 'NONE', #18526, #1134, #26078 ) ;
#5810 = DIRECTION ( 'NONE',  ( -0.8746197071393895239, 0.4848096202463481053, 0.000000000000000000 ) ) ;
#5811 = AXIS2_PLACEMENT_3D ( 'NONE', #21100, #11116, #13265 ) ;
#5812 = EDGE_LOOP ( 'NONE', ( #26107, #18547, #641, #2117 ) ) ;
#5813 = CARTESIAN_POINT ( 'NONE',  ( -40.62282199596570109, 7.625347238340325795, 53.94439779120587986 ) ) ;
#5814 = DIRECTION ( 'NONE',  ( -0.000000000000000000, -1.000000000000000000, -0.000000000000000000 ) ) ;
#5815 = EDGE_CURVE ( 'NONE', #3106, #12291, #19835, .T. ) ;
#5816 = CARTESIAN_POINT ( 'NONE',  ( 8.732853799281738105, 28.96183152705961206, 47.04930799450051637 ) ) ;
#5817 = ORIENTED_EDGE ( 'NONE', *, *, #6229, .F. ) ;
#5818 = CARTESIAN_POINT ( 'NONE',  ( 46.45846941443645761, 22.99884124225578930, 45.79590206249746132 ) ) ;
#5819 = DIRECTION ( 'NONE',  ( -1.224646799147353207E-16, -1.349345573449484691E-32, 1.000000000000000000 ) ) ;
#5820 = CIRCLE ( 'NONE', #2681, 4.200000000000000178 ) ;
#5821 = CARTESIAN_POINT ( 'NONE',  ( 45.23477325667712989, 24.76454579224779806, 43.39705899138675704 ) ) ;
#5822 = EDGE_CURVE ( 'NONE', #12300, #2537, #32443, .T. ) ;
#5823 = DIRECTION ( 'NONE',  ( -1.101824276508909887E-16, 1.000000000000000000, -0.000000000000000000 ) ) ;
#5824 = CARTESIAN_POINT ( 'NONE',  ( 21.09785597605720753, 15.70210863493540288, 47.04930799450052348 ) ) ;
#5825 = ORIENTED_EDGE ( 'NONE', *, *, #20564, .F. ) ;
#5826 = CARTESIAN_POINT ( 'NONE',  ( 47.76133520913771235, 29.61346213614034895, 45.10342086390699734 ) ) ;
#5827 = CARTESIAN_POINT ( 'NONE',  ( 49.73059755354898215, 24.88073588970408423, 46.43791210414119064 ) ) ;
#5828 = CARTESIAN_POINT ( 'NONE',  ( -39.85048242108726413, 2.742214340073605428, 45.54930799450051637 ) ) ;
#5829 = B_SPLINE_CURVE_WITH_KNOTS ( 'NONE', 3,
 ( #8076, #15603, #23326, #837, #10862, #27361, #22263, #21611, #31645, #24403 ),
 .UNSPECIFIED., .F., .F.,
 ( 4, 2, 2, 2, 4 ),
 ( 0.000000000000000000, 0.0008791187685415481319, 0.001318678152812310976, 0.001538457844947706656, 0.001758237537083101685 ),
 .UNSPECIFIED. ) ;
#5830 = ORIENTED_EDGE ( 'NONE', *, *, #17573, .T. ) ;
#5831 = CARTESIAN_POINT ( 'NONE',  ( -10.11676764852370880, -5.928581419070745540, -12.41916627326984290 ) ) ;
#5832 = DIRECTION ( 'NONE',  ( -1.000000000000000000, 0.000000000000000000, -1.224646799147353207E-16 ) ) ;
#5833 = EDGE_CURVE ( 'NONE', #9196, #8819, #14093, .T. ) ;
#5834 = ADVANCED_FACE ( 'NONE', ( #32271 ), #19941, .F. ) ;
#5835 = CARTESIAN_POINT ( 'NONE',  ( 21.09785597605720042, -13.64309448858209528, -11.84046438077000118 ) ) ;
#5836 = CARTESIAN_POINT ( 'NONE',  ( 54.83359747464948697, -2.706209967029943986, -8.239931912618725818 ) ) ;
#5837 = EDGE_CURVE ( 'NONE', #23957, #16025, #28241, .T. ) ;
#5838 = EDGE_LOOP ( 'NONE', ( #12861, #28090, #20021, #25579 ) ) ;
#5839 = CARTESIAN_POINT ( 'NONE',  ( -40.59783212598355107, 7.538197204814858665, 60.10545411752895006 ) ) ;
#5840 = AXIS2_PLACEMENT_3D ( 'NONE', #23735, #8648, #13421 ) ;
#5841 = VERTEX_POINT ( 'NONE', #19456 ) ;
#5842 = CIRCLE ( 'NONE', #4227, 0.1000000000000024064 ) ;
#5843 = B_SPLINE_CURVE_WITH_KNOTS ( 'NONE', 3,
 ( #28896, #1147, #21160, #31522, #8862, #9192, #19183, #23794, #18695, #31199, #1309, #16563 ),
 .UNSPECIFIED., .F., .F.,
 ( 4, 2, 2, 2, 2, 4 ),
 ( 0.0002262581842376736074, 0.001077027684495157536, 0.001927797184752641328, 0.002778566685010125121, 0.003203951435138863331, 0.003629336185267601107 ),
 .UNSPECIFIED. ) ;
#5844 = TOROIDAL_SURFACE ( 'NONE', #6343, 32.50000000000000000, 1.499999999999999556 ) ;
#5845 = EDGE_LOOP ( 'NONE', ( #18482, #7052, #16904, #12038 ) ) ;
#5846 = EDGE_CURVE ( 'NONE', #30037, #14004, #22456, .T. ) ;
#5847 = AXIS2_PLACEMENT_3D ( 'NONE', #22050, #16957, #24689 ) ;
#5848 = CARTESIAN_POINT ( 'NONE',  ( -35.78489663495318496, -5.401021002517912173, 79.44869760013504845 ) ) ;
#5849 = CARTESIAN_POINT ( 'NONE',  ( 49.32483701613094240, 27.00322093266652601, 45.91328182968236860 ) ) ;
#5850 = ORIENTED_EDGE ( 'NONE', *, *, #3104, .T. ) ;
#5851 = CARTESIAN_POINT ( 'NONE',  ( 21.09785597605720042, -13.59284023713420630, 47.04930799450051637 ) ) ;
#5852 = VERTEX_POINT ( 'NONE', #5351 ) ;
#5853 = AXIS2_PLACEMENT_3D ( 'NONE', #26513, #16647, #4025 ) ;
#5854 = CARTESIAN_POINT ( 'NONE',  ( -41.63422246745999189, 11.51531537899137447, 56.14611646155296398 ) ) ;
#5855 = AXIS2_PLACEMENT_3D ( 'NONE', #23260, #10799, #15876 ) ;
#5856 = CARTESIAN_POINT ( 'NONE',  ( -40.47970302497626705, 7.463434137431151250, 53.80788663826320573 ) ) ;
#5857 = CARTESIAN_POINT ( 'NONE',  ( -30.49287641343807209, 11.01517781903025650, 71.67080780280015517 ) ) ;
#5858 = ADVANCED_FACE ( 'NONE', ( #737 ), #9941, .T. ) ;
#5859 = CARTESIAN_POINT ( 'NONE',  ( -40.65487266620045403, 9.475231293617264683, 35.46144002885649371 ) ) ;
#5860 = VECTOR ( 'NONE', #22384, 1000.000000000000000 ) ;
#5861 = ORIENTED_EDGE ( 'NONE', *, *, #25008, .F. ) ;
#5862 = DIRECTION ( 'NONE',  ( -0.05186525298099804726, -2.168404344971009854E-16, 0.9986540920324800119 ) ) ;
#5863 = ORIENTED_EDGE ( 'NONE', *, *, #26204, .T. ) ;
#5864 = DIRECTION ( 'NONE',  ( -0.4544104193609905806, -5.611869858668446909E-17, -0.8907924397839086517 ) ) ;
#5865 = CARTESIAN_POINT ( 'NONE',  ( -42.36153388572594736, 13.68895619636815653, 54.64930799450051779 ) ) ;
#5866 = ORIENTED_EDGE ( 'NONE', *, *, #14122, .T. ) ;
#5867 = CARTESIAN_POINT ( 'NONE',  ( -41.24971778908466291, 11.62557032131817181, 56.04611646155296256 ) ) ;
#5868 = ADVANCED_FACE ( 'NONE', ( #30620 ), #20593, .F. ) ;
#5869 = CARTESIAN_POINT ( 'NONE',  ( -36.45222641229887017, 9.925589859889724309, 52.04930799450051637 ) ) ;
#5870 = CARTESIAN_POINT ( 'NONE',  ( 45.50623141997586174, 22.89977464660286444, 48.01957109218837871 ) ) ;
#5871 = CARTESIAN_POINT ( 'NONE',  ( 21.09992658989238734, 32.34164230456639899, 47.04930799450051637 ) ) ;
#5872 = ORIENTED_EDGE ( 'NONE', *, *, #11025, .T. ) ;
#5873 = CARTESIAN_POINT ( 'NONE',  ( -41.94956971822180947, 3.905757428664830222, 45.84930799450051353 ) ) ;
#5874 = DIRECTION ( 'NONE',  ( -0.000000000000000000, -1.000000000000000000, -0.000000000000000000 ) ) ;
#5875 = ORIENTED_EDGE ( 'NONE', *, *, #17045, .T. ) ;
#5876 = DIRECTION ( 'NONE',  ( 1.000000000000000000, 0.000000000000000000, 0.000000000000000000 ) ) ;
#5877 = VECTOR ( 'NONE', #17011, 1000.000000000000114 ) ;
#5878 = ADVANCED_FACE ( 'NONE', ( #12746 ), #18280, .T. ) ;
#5879 = CARTESIAN_POINT ( 'NONE',  ( -44.28695544631908376, -5.935454207752205669, 40.04930799450050216 ) ) ;
#5880 = ORIENTED_EDGE ( 'NONE', *, *, #4176, .F. ) ;
#5881 = ORIENTED_EDGE ( 'NONE', *, *, #15437, .F. ) ;
#5882 = CARTESIAN_POINT ( 'NONE',  ( -12.44358483960257189, -1.094061166256872442, 101.4093159356342682 ) ) ;
#5883 = EDGE_LOOP ( 'NONE', ( #31295, #1572 ) ) ;
#5884 = TOROIDAL_SURFACE ( 'NONE', #17390, 12.40141737965283397, 0.1249999999999992922 ) ;
#5885 = AXIS2_PLACEMENT_3D ( 'NONE', #11872, #18916, #14339 ) ;
#5886 = ORIENTED_EDGE ( 'NONE', *, *, #25435, .T. ) ;
#5887 = TOROIDAL_SURFACE ( 'NONE', #10086, 12.61792373059897265, 0.1249999999999971551 ) ;
#5888 = ORIENTED_EDGE ( 'NONE', *, *, #15318, .F. ) ;
#5889 = AXIS2_PLACEMENT_3D ( 'NONE', #17336, #27358, #20931 ) ;
#5890 = CARTESIAN_POINT ( 'NONE',  ( -40.52669582637187773, 7.652910973922034010, 53.94439779120588696 ) ) ;
#5891 = FACE_OUTER_BOUND ( 'NONE', #10062, .T. ) ;
#5892 = DIRECTION ( 'NONE',  ( -1.101824276508909887E-16, 1.000000000000000000, -0.000000000000000000 ) ) ;
#5893 = CARTESIAN_POINT ( 'NONE',  ( 46.99218062947583974, 27.85956182964376282, 49.08406571254116102 ) ) ;
#5894 = ORIENTED_EDGE ( 'NONE', *, *, #22486, .T. ) ;
#5895 = VERTEX_POINT ( 'NONE', #20426 ) ;
#5896 = DIRECTION ( 'NONE',  ( 0.000000000000000000, -0.2964022880492265255, -0.9550631830613005580 ) ) ;
#5897 = EDGE_LOOP ( 'NONE', ( #27475, #8813, #31328, #23417 ) ) ;
#5898 = AXIS2_PLACEMENT_3D ( 'NONE', #30684, #16367, #23122 ) ;
#5899 = CARTESIAN_POINT ( 'NONE',  ( 21.09785597605720753, 13.68462854903246573, 47.04930799450052348 ) ) ;
#5900 = CARTESIAN_POINT ( 'NONE',  ( 54.62670865243408258, -1.035104995753989954, 101.3786800976585738 ) ) ;
#5901 = FACE_OUTER_BOUND ( 'NONE', #32292, .T. ) ;
#5902 = VECTOR ( 'NONE', #14264, 1000.000000000000000 ) ;
#5903 = CARTESIAN_POINT ( 'NONE',  ( 8.732853799281732776, 38.56284415653841791, 47.04930799450051637 ) ) ;
#5904 = DIRECTION ( 'NONE',  ( -1.000000000000000000, 0.000000000000000000, -1.224646799147353207E-16 ) ) ;
#5905 = VERTEX_POINT ( 'NONE', #17966 ) ;
#5906 = DIRECTION ( 'NONE',  ( -1.000000000000000000, 0.000000000000000000, 0.000000000000000000 ) ) ;
#5907 = DIRECTION ( 'NONE',  ( 0.000000000000000000, 0.000000000000000000, -1.000000000000000000 ) ) ;
#5908 = EDGE_CURVE ( 'NONE', #29601, #20020, #14648, .T. ) ;
#5909 = FACE_OUTER_BOUND ( 'NONE', #8842, .T. ) ;
#5910 = DIRECTION ( 'NONE',  ( -1.000000000000000000, 0.000000000000000000, 0.000000000000000000 ) ) ;
#5911 = ORIENTED_EDGE ( 'NONE', *, *, #26650, .T. ) ;
#5912 = DIRECTION ( 'NONE',  ( -1.000000000000000000, 0.000000000000000000, 0.000000000000000000 ) ) ;
#5913 = CARTESIAN_POINT ( 'NONE',  ( -40.59307405792753798, 7.534955460439823227, 53.80788663826319862 ) ) ;
#5914 = ORIENTED_EDGE ( 'NONE', *, *, #1709, .F. ) ;
#5915 = AXIS2_PLACEMENT_3D ( 'NONE', #16724, #19522, #11988 ) ;
#5916 = CIRCLE ( 'NONE', #30546, 0.1250000000000001110 ) ;
#5917 = ORIENTED_EDGE ( 'NONE', *, *, #31720, .F. ) ;
#5918 = AXIS2_PLACEMENT_3D ( 'NONE', #4858, #25204, #94 ) ;
#5919 =( BOUNDED_CURVE ( )  B_SPLINE_CURVE ( 2, ( #5552, #17527, #20302, #25402, #25558, #17683, #22439, #7364, #3064 ),
 .UNSPECIFIED., .F., .F. ) 
 B_SPLINE_CURVE_WITH_KNOTS ( ( 3, 2, 2, 2, 3 ),
 ( 0.2500000011612727446, 0.2619047619047619180, 0.2857142857142856984, 0.3095238095238095344, 0.3214285725898440860 ),
 .UNSPECIFIED. ) 
 CURVE ( )  GEOMETRIC_REPRESENTATION_ITEM ( )  RATIONAL_B_SPLINE_CURVE ( ( 0.9330127018922200755, 0.9330127084266233162, 1.000000000000000000, 0.8660254037844388186, 1.000000000000000000, 0.8660254037844388186, 1.000000000000000000, 0.9330126953578159466, 0.9330127018922200755 ) ) 
 REPRESENTATION_ITEM ( '' )  );
#5920 = ORIENTED_EDGE ( 'NONE', *, *, #1851, .T. ) ;
#5921 = CARTESIAN_POINT ( 'NONE',  ( -41.04685960816998147, 9.497330455345890599, 38.54930799450052348 ) ) ;
#5922 = CARTESIAN_POINT ( 'NONE',  ( -44.35282064072296748, -4.283462843672324105, 52.07173525871509412 ) ) ;
#5923 = CARTESIAN_POINT ( 'NONE',  ( 21.09785597605720753, -5.098646251524523443, 47.04930799450052348 ) ) ;
#5924 = ORIENTED_EDGE ( 'NONE', *, *, #31820, .T. ) ;
#5925 = DIRECTION ( 'NONE',  ( 0.000000000000000000, -0.000000000000000000, -1.000000000000000000 ) ) ;
#5926 = DIRECTION ( 'NONE',  ( 0.8746197071393926326, -0.4848096202463430537, -8.676864087101709653E-18 ) ) ;
#5927 = CARTESIAN_POINT ( 'NONE',  ( 47.28715512441527125, 22.91889071986277671, 48.84357536195264515 ) ) ;
#5928 = EDGE_LOOP ( 'NONE', ( #7459, #14271, #25219, #19380 ) ) ;
#5929 = DIRECTION ( 'NONE',  ( -1.188208965918165239E-16, -1.880121038077812639E-16, -1.000000000000000000 ) ) ;
#5930 = ORIENTED_EDGE ( 'NONE', *, *, #1708, .T. ) ;
#5931 = DIRECTION ( 'NONE',  ( -1.000000000000000000, 0.000000000000000000, 0.000000000000000000 ) ) ;
#5932 = DIRECTION ( 'NONE',  ( -1.000000000000000000, -1.101824276508909887E-16, 0.000000000000000000 ) ) ;
#5933 = DIRECTION ( 'NONE',  ( -1.000000000000000000, -1.101824276508910010E-16, 0.000000000000000000 ) ) ;
#5934 = CARTESIAN_POINT ( 'NONE',  ( 21.09785597605719332, -19.93545420775220123, 47.04930799450051637 ) ) ;
#5935 = CONICAL_SURFACE ( 'NONE', #32123, 12.00000000000000355, 0.7853981633974466137 ) ;
#5936 = LINE ( 'NONE', #8869, #16264 ) ;
#5937 = CIRCLE ( 'NONE', #171, 0.9031915329475500576 ) ;
#5938 = SURFACE_STYLE_USAGE ( .BOTH. , #28735 ) ;
#5939 = ORIENTED_EDGE ( 'NONE', *, *, #5054, .T. ) ;
#5940 = ORIENTED_EDGE ( 'NONE', *, *, #25803, .T. ) ;
#5941 = CARTESIAN_POINT ( 'NONE',  ( 57.98048228007294114, -13.30632128221581212, 89.09797539074718031 ) ) ;
#5942 = CARTESIAN_POINT ( 'NONE',  ( 8.823509210239521394, 25.84164230456639899, 47.04930799450051637 ) ) ;
#5943 = EDGE_CURVE ( 'NONE', #24037, #17607, #2602, .T. ) ;
#5944 = CARTESIAN_POINT ( 'NONE',  ( 51.44386815995735418, 5.417291301124356195, 98.18922675647870335 ) ) ;
#5945 = EDGE_CURVE ( 'NONE', #15557, #27550, #23544, .T. ) ;
#5946 = EDGE_CURVE ( 'NONE', #321, #12078, #27748, .T. ) ;
#5947 = ORIENTED_EDGE ( 'NONE', *, *, #8224, .F. ) ;
#5948 = CIRCLE ( 'NONE', #4368, 12.36707279061065101 ) ;
#5949 = CARTESIAN_POINT ( 'NONE',  ( 8.474859994195286461, 24.09184655352419213, 47.04930799450051637 ) ) ;
#5950 = CARTESIAN_POINT ( 'NONE',  ( -40.02327307428360115, 7.071123406435155800, 39.20438120789051339 ) ) ;
#5951 = AXIS2_PLACEMENT_3D ( 'NONE', #965, #10987, #20982 ) ;
#5952 = ADVANCED_FACE ( 'NONE', ( #13385 ), #28155, .F. ) ;
#5953 = EDGE_LOOP ( 'NONE', ( #24646, #2867, #26798, #22358 ) ) ;
#5954 = DIRECTION ( 'NONE',  ( -1.101824276508909887E-16, 1.000000000000000000, -0.000000000000000000 ) ) ;
#5955 = ADVANCED_FACE ( 'NONE', ( #30458 ), #22735, .T. ) ;
#5956 = CARTESIAN_POINT ( 'NONE',  ( 48.46535932150934656, 28.98954579807170617, 49.73005965046827015 ) ) ;
#5957 = CARTESIAN_POINT ( 'NONE',  ( -39.39870901941788617, -5.936041284844024268, 77.94996054681324438 ) ) ;
#5958 = VERTEX_POINT ( 'NONE', #30137 ) ;
#5959 = VECTOR ( 'NONE', #8644, 1000.000000000000000 ) ;
#5960 = CARTESIAN_POINT ( 'NONE',  ( 51.92840300912122586, -5.935709855254033940, -13.61832391111114937 ) ) ;
#5961 = CARTESIAN_POINT ( 'NONE',  ( 36.37380348623724302, 15.23758267881771111, 47.04930799450052348 ) ) ;
#5962 = VERTEX_POINT ( 'NONE', #22893 ) ;
#5963 = AXIS2_PLACEMENT_3D ( 'NONE', #3504, #27985, #13698 ) ;
#5964 = CIRCLE ( 'NONE', #8582, 0.1250000000000001110 ) ;
#5965 = CIRCLE ( 'NONE', #11729, 37.50000000000000711 ) ;
#5966 = CARTESIAN_POINT ( 'NONE',  ( 33.72499318558949710, 29.09143805560861296, 47.04930799450051637 ) ) ;
#5967 = DIRECTION ( 'NONE',  ( 0.000000000000000000, 0.000000000000000000, -1.000000000000000000 ) ) ;
#5968 = ADVANCED_FACE ( 'NONE', ( #27660 ), #5507, .T. ) ;
#5969 = DIRECTION ( 'NONE',  ( -1.000000000000000000, 0.000000000000000000, 0.000000000000000000 ) ) ;
#5970 = EDGE_CURVE ( 'NONE', #10137, #29664, #12018, .T. ) ;
#5971 = VERTEX_POINT ( 'NONE', #2872 ) ;
#5972 = FACE_OUTER_BOUND ( 'NONE', #21824, .T. ) ;
#5973 = CARTESIAN_POINT ( 'NONE',  ( -40.60922101150777053, 7.585765375989693915, 53.90260032368192356 ) ) ;
#5974 = DIRECTION ( 'NONE',  ( 1.000000000000000000, 0.000000000000000000, 0.000000000000000000 ) ) ;
#5975 = AXIS2_PLACEMENT_3D ( 'NONE', #11580, #21575, #21251 ) ;
#5976 = DIRECTION ( 'NONE',  ( 2.779292025043186357E-18, -1.288349127009862211E-17, 1.000000000000000000 ) ) ;
#5977 = DIRECTION ( 'NONE',  ( 1.000000000000000000, 0.000000000000000000, 0.000000000000000000 ) ) ;
#5978 = ORIENTED_EDGE ( 'NONE', *, *, #32402, .F. ) ;
#5979 = DIRECTION ( 'NONE',  ( 0.000000000000000000, 0.000000000000000000, -1.000000000000000000 ) ) ;
#5980 = DIRECTION ( 'NONE',  ( 0.000000000000000000, 0.000000000000000000, 1.000000000000000000 ) ) ;
#5981 = CARTESIAN_POINT ( 'NONE',  ( 76.05035340485899553, -2.181906231263063933, 80.77867826514622607 ) ) ;
#5982 = EDGE_LOOP ( 'NONE', ( #28899, #745, #6137, #18708 ) ) ;
#5983 = CARTESIAN_POINT ( 'NONE',  ( 21.09785597605720753, 14.86454579224779948, 47.04930799450052348 ) ) ;
#5984 = DIRECTION ( 'NONE',  ( -1.101824276508909887E-16, 1.000000000000000000, -0.000000000000000000 ) ) ;
#5985 = DIRECTION ( 'NONE',  ( -0.000000000000000000, -1.000000000000000000, 0.000000000000000000 ) ) ;
#5986 = EDGE_LOOP ( 'NONE', ( #20602, #9686, #13312, #23710 ) ) ;
#5987 = CARTESIAN_POINT ( 'NONE',  ( -40.14354458344919863, 7.767885906595227929, 53.80788663826320573 ) ) ;
#5988 = EDGE_CURVE ( 'NONE', #20933, #3444, #2062, .T. ) ;
#5989 = CARTESIAN_POINT ( 'NONE',  ( 21.09785597605719332, 24.86454579224779948, 23.54930799450051637 ) ) ;
#5990 = CARTESIAN_POINT ( 'NONE',  ( 52.94504501510867556, -5.721341737285968065, -11.26059709029990330 ) ) ;
#5991 = ORIENTED_EDGE ( 'NONE', *, *, #20389, .F. ) ;
#5992 = CARTESIAN_POINT ( 'NONE',  ( 8.732853799281738105, 27.71183152705960850, 47.04930799450051637 ) ) ;
#5993 = ORIENTED_EDGE ( 'NONE', *, *, #1293, .T. ) ;
#5994 = ORIENTED_EDGE ( 'NONE', *, *, #19785, .F. ) ;
#5995 = EDGE_CURVE ( 'NONE', #20242, #18754, #18128, .T. ) ;
#5996 = ADVANCED_FACE ( 'NONE', ( #23221 ), #17778, .T. ) ;
#5997 = AXIS2_PLACEMENT_3D ( 'NONE', #21521, #8734, #18731 ) ;
#5998 = CARTESIAN_POINT ( 'NONE',  ( 21.09785597605720753, 14.86454579224779948, 47.04930799450052348 ) ) ;
#5999 = CYLINDRICAL_SURFACE ( 'NONE', #11416, 12.62506659569710266 ) ;
#6000 = AXIS2_PLACEMENT_3D ( 'NONE', #4875, #427, #269 ) ;
#6001 = DIRECTION ( 'NONE',  ( 1.234978253042719660E-16, -1.000000000000000000, -1.109335647967047851E-31 ) ) ;
#6002 = EDGE_CURVE ( 'NONE', #9593, #22169, #24594, .T. ) ;
#6003 = AXIS2_PLACEMENT_3D ( 'NONE', #1840, #6927, #23834 ) ;
#6004 = EDGE_CURVE ( 'NONE', #14867, #27708, #4690, .T. ) ;
#6005 = ORIENTED_EDGE ( 'NONE', *, *, #16642, .T. ) ;
#6006 = CARTESIAN_POINT ( 'NONE',  ( 21.09992658989239089, 27.34143805560860940, 47.04930799450051637 ) ) ;
#6007 = ORIENTED_EDGE ( 'NONE', *, *, #28795, .T. ) ;
#6008 = AXIS2_PLACEMENT_3D ( 'NONE', #23985, #32198, #19212 ) ;
#6009 = CARTESIAN_POINT ( 'NONE',  ( -9.728297238921257417, -5.935454207752202116, 97.43646483284780402 ) ) ;
#6010 = DIRECTION ( 'NONE',  ( -0.000000000000000000, -1.000000000000000000, -0.000000000000000000 ) ) ;
#6011 = DIRECTION ( 'NONE',  ( -1.000000000000000000, 0.000000000000000000, 0.000000000000000000 ) ) ;
#6012 = CARTESIAN_POINT ( 'NONE',  ( 21.09785597605720753, 14.86454579224779948, 47.04930799450052348 ) ) ;
#6013 = EDGE_LOOP ( 'NONE', ( #31914, #11162, #31952, #2106 ) ) ;
#6014 = DIRECTION ( 'NONE',  ( -0.1540342867254181347, 0.6907746437949939811, -0.7064728091037127955 ) ) ;
#6015 = CARTESIAN_POINT ( 'NONE',  ( 21.09992658989239089, 29.84164230456639899, 47.04930799450051637 ) ) ;
#6016 = DIRECTION ( 'NONE',  ( 1.000000000000000000, 0.000000000000000000, 0.000000000000000000 ) ) ;
#6017 = DIRECTION ( 'NONE',  ( 0.000000000000000000, -0.000000000000000000, 1.000000000000000000 ) ) ;
#6018 = ORIENTED_EDGE ( 'NONE', *, *, #25247, .F. ) ;
#6019 = DIRECTION ( 'NONE',  ( 0.000000000000000000, -0.000000000000000000, -1.000000000000000000 ) ) ;
#6020 = FACE_OUTER_BOUND ( 'NONE', #2896, .T. ) ;
#6021 = DIRECTION ( 'NONE',  ( 1.000000000000000000, 0.000000000000000000, 0.000000000000000000 ) ) ;
#6022 = CARTESIAN_POINT ( 'NONE',  ( -39.55402147699608406, 7.608641254004257171, 62.04930799450052348 ) ) ;
#6023 = CARTESIAN_POINT ( 'NONE',  ( 48.18662509608405031, 25.09624452788249371, 49.18364984542562013 ) ) ;
#6024 = ORIENTED_EDGE ( 'NONE', *, *, #2486, .F. ) ;
#6025 = FACE_OUTER_BOUND ( 'NONE', #9430, .T. ) ;
#6026 = CARTESIAN_POINT ( 'NONE',  ( -40.54123211584830244, 7.002658380788985504, 35.02021009580667510 ) ) ;
#6027 = ORIENTED_EDGE ( 'NONE', *, *, #6410, .T. ) ;
#6028 = EDGE_CURVE ( 'NONE', #29052, #14004, #29860, .T. ) ;
#6029 = DIRECTION ( 'NONE',  ( 0.000000000000000000, -0.6995351541602693457, 0.7145981864614324719 ) ) ;
#6030 = CARTESIAN_POINT ( 'NONE',  ( 21.09785597605720753, 13.86454579224779948, 47.04930799450052348 ) ) ;
#6031 = ORIENTED_EDGE ( 'NONE', *, *, #747, .T. ) ;
#6032 = CIRCLE ( 'NONE', #3393, 2.950930354263400890 ) ;
#6033 = ORIENTED_EDGE ( 'NONE', *, *, #30807, .F. ) ;
#6034 = CARTESIAN_POINT ( 'NONE',  ( 21.09785597605719332, 25.56454579224779167, 33.84930799450050642 ) ) ;
#6035 = AXIS2_PLACEMENT_3D ( 'NONE', #20212, #27275, #9725 ) ;
#6036 = VECTOR ( 'NONE', #13484, 1000.000000000000227 ) ;
#6037 = CIRCLE ( 'NONE', #242, 43.50000000000000000 ) ;
#6038 = CIRCLE ( 'NONE', #7081, 1.500000000000001332 ) ;
#6039 = VERTEX_POINT ( 'NONE', #24178 ) ;
#6040 = EDGE_CURVE ( 'NONE', #655, #3764, #20910, .T. ) ;
#6041 = ADVANCED_FACE ( 'NONE', ( #8450 ), #20398, .T. ) ;
#6042 = ORIENTED_EDGE ( 'NONE', *, *, #14998, .T. ) ;
#6043 = CARTESIAN_POINT ( 'NONE',  ( 80.77181806311266143, 8.310461108307681144, 18.62663443640236238 ) ) ;
#6044 = EDGE_CURVE ( 'NONE', #1224, #3218, #26325, .T. ) ;
#6045 = EDGE_LOOP ( 'NONE', ( #2651, #32227, #8094 ) ) ;
#6046 = ADVANCED_FACE ( 'NONE', ( #23856 ), #5232, .T. ) ;
#6047 = AXIS2_PLACEMENT_3D ( 'NONE', #27066, #12471, #27401 ) ;
#6048 = CARTESIAN_POINT ( 'NONE',  ( 48.04379483844901699, 22.98879437201065912, 48.17263172485531442 ) ) ;
#6049 = CYLINDRICAL_SURFACE ( 'NONE', #12764, 0.1000000000000020595 ) ;
#6050 = CARTESIAN_POINT ( 'NONE',  ( 45.28286642839709231, 27.74289516297709568, 47.97516931882780966 ) ) ;
#6051 = ORIENTED_EDGE ( 'NONE', *, *, #1036, .F. ) ;
#6052 = VERTEX_POINT ( 'NONE', #26158 ) ;
#6054 =( NAMED_UNIT ( * ) PLANE_ANGLE_UNIT ( ) SI_UNIT ( $, .RADIAN. ) );
#6053 = AXIS2_PLACEMENT_3D ( 'NONE', #11741, #14698, #9605 ) ;
#6055 = ORIENTED_EDGE ( 'NONE', *, *, #24268, .F. ) ;
#6056 = LINE ( 'NONE', #28862, #25174 ) ;
#6057 = VECTOR ( 'NONE', #25979, 1000.000000000000114 ) ;
#6058 = CARTESIAN_POINT ( 'NONE',  ( 50.60998280159589058, 6.668192824305383404, 98.79818430532178297 ) ) ;
#6059 = DIRECTION ( 'NONE',  ( -0.3597811455230787714, 0.7883456110718085608, -0.4990678559373643575 ) ) ;
#6060 = CARTESIAN_POINT ( 'NONE',  ( 21.09785597605720042, -5.986312001188950127, 114.4134811058425640 ) ) ;
#6061 = CARTESIAN_POINT ( 'NONE',  ( 8.732853799281731000, 28.22145308207318237, 47.04930799450051637 ) ) ;
#6062 = ORIENTED_EDGE ( 'NONE', *, *, #8060, .F. ) ;
#6063 = FACE_BOUND ( 'NONE', #12293, .T. ) ;
#6064 = CARTESIAN_POINT ( 'NONE',  ( -34.53047946185701988, -4.295946708764400768, 13.71755887862822476 ) ) ;
#6065 = CARTESIAN_POINT ( 'NONE',  ( -40.60333149162104860, 7.557375771971046596, 60.54930799450051637 ) ) ;
#6066 = CARTESIAN_POINT ( 'NONE',  ( 21.09992658989239089, 25.96664230456639899, 47.04930799450051637 ) ) ;
#6067 = DIRECTION ( 'NONE',  ( -1.000000000000000000, 0.000000000000000000, 0.000000000000000000 ) ) ;
#6068 = CARTESIAN_POINT ( 'NONE',  ( -39.64148344771002286, 7.657122216028890982, 32.04930799450052348 ) ) ;
#6069 = EDGE_LOOP ( 'NONE', ( #21799, #20289 ) ) ;
#6070 = CARTESIAN_POINT ( 'NONE',  ( 21.09992658989239089, 27.09184655352419568, 47.04930799450051637 ) ) ;
#6071 = LINE ( 'NONE', #818, #29815 ) ;
#6072 = ORIENTED_EDGE ( 'NONE', *, *, #30135, .T. ) ;
#6073 = ADVANCED_FACE ( 'NONE', ( #14018 ), #18808, .T. ) ;
#6074 = AXIS2_PLACEMENT_3D ( 'NONE', #15977, #28615, #726 ) ;
#6075 = STYLED_ITEM ( 'NONE', ( #27283 ), #8502 ) ;
#6076 = EDGE_LOOP ( 'NONE', ( #16530, #10990, #31310, #11925 ) ) ;
#6077 = CARTESIAN_POINT ( 'NONE',  ( -41.10316901461906980, 9.481183992871798694, 38.54930799450053058 ) ) ;
#6078 = DIRECTION ( 'NONE',  ( 0.9612616959383200044, 0.2756373558169954996, -1.660411357259285896E-16 ) ) ;
#6079 = DIRECTION ( 'NONE',  ( 0.000000000000000000, 0.000000000000000000, -1.000000000000000000 ) ) ;
#6080 = ADVANCED_FACE ( 'NONE', ( #18920 ), #25654, .T. ) ;
#6081 = CIRCLE ( 'NONE', #32282, 12.27641737965286772 ) ;
#6082 = EDGE_LOOP ( 'NONE', ( #7343, #22582, #11643, #27869 ) ) ;
#6083 = CARTESIAN_POINT ( 'NONE',  ( 33.46699938050304013, 25.47145308207319303, 47.04930799450050927 ) ) ;
#6084 = FACE_OUTER_BOUND ( 'NONE', #26768, .T. ) ;
#6085 = CARTESIAN_POINT ( 'NONE',  ( 21.09785597605719332, 24.56454579224780232, 47.04930799450051637 ) ) ;
#6086 = ORIENTED_EDGE ( 'NONE', *, *, #21961, .F. ) ;
#6087 = CARTESIAN_POINT ( 'NONE',  ( 48.72149481846882679, 22.88065857334295217, 48.10262368218729279 ) ) ;
#6088 = ORIENTED_EDGE ( 'NONE', *, *, #2990, .F. ) ;
#6089 = LINE ( 'NONE', #28576, #11765 ) ;
#6090 = CARTESIAN_POINT ( 'NONE',  ( 21.09785597605720753, 14.36454579224779948, 47.04930799450052348 ) ) ;
#6091 = DIRECTION ( 'NONE',  ( 0.000000000000000000, 0.000000000000000000, -1.000000000000000000 ) ) ;
#6092 = EDGE_LOOP ( 'NONE', ( #31691, #5583, #25751 ) ) ;
#6093 = ORIENTED_EDGE ( 'NONE', *, *, #22791, .T. ) ;
#6094 = DIRECTION ( 'NONE',  ( 1.000000000000000000, 0.000000000000000000, 0.000000000000000000 ) ) ;
#6095 = AXIS2_PLACEMENT_3D ( 'NONE', #19361, #1321, #24295 ) ;
#6096 = DIRECTION ( 'NONE',  ( 1.313185983435984691E-29, -1.000000000000000000, -3.761114140369702165E-15 ) ) ;
#6097 = FACE_BOUND ( 'NONE', #18381, .T. ) ;
#6098 = ORIENTED_EDGE ( 'NONE', *, *, #24228, .T. ) ;
#6099 = DIRECTION ( 'NONE',  ( -1.101824276508909887E-16, 1.000000000000000000, -0.000000000000000000 ) ) ;
#6100 = LINE ( 'NONE', #13659, #14661 ) ;
#6101 = ORIENTED_EDGE ( 'NONE', *, *, #24054, .T. ) ;
#6102 = FACE_OUTER_BOUND ( 'NONE', #30618, .T. ) ;
#6103 = CARTESIAN_POINT ( 'NONE',  ( 45.46000861347822308, 29.57287913140503832, 49.57397645940629616 ) ) ;
#6104 = AXIS2_PLACEMENT_3D ( 'NONE', #7624, #4665, #12881 ) ;
#6105 = CARTESIAN_POINT ( 'NONE',  ( 21.09785597605720753, 14.66454579224779842, 47.04930799450052348 ) ) ;
#6106 = VERTEX_POINT ( 'NONE', #26643 ) ;
#6107 = CARTESIAN_POINT ( 'NONE',  ( 21.09992658989238734, 31.47145308207317171, 47.04930799450051637 ) ) ;
#6108 = CIRCLE ( 'NONE', #16575, 12.62506659569710266 ) ;
#6109 = CARTESIAN_POINT ( 'NONE',  ( -40.02540636251514172, 2.839176264122877047, 57.04930799450051637 ) ) ;
#6110 = CARTESIAN_POINT ( 'NONE',  ( 8.474859994195286461, 26.09143805560860940, 47.04930799450051637 ) ) ;
#6111 = DIRECTION ( 'NONE',  ( -0.000000000000000000, -1.000000000000000000, 0.000000000000000000 ) ) ;
#6112 = EDGE_CURVE ( 'NONE', #19482, #20710, #16307, .T. ) ;
#6113 = ORIENTED_EDGE ( 'NONE', *, *, #12775, .T. ) ;
#6114 = ADVANCED_FACE ( 'NONE', ( #24017 ), #11233, .T. ) ;
#6115 = EDGE_CURVE ( 'NONE', #24091, #24927, #6139, .T. ) ;
#6116 = EDGE_CURVE ( 'NONE', #15784, #13775, #23567, .T. ) ;
#6117 = ADVANCED_FACE ( 'NONE', ( #3836 ), #28284, .T. ) ;
#6118 = CARTESIAN_POINT ( 'NONE',  ( -42.38687957179149635, 4.148162238787999279, 37.04930799450052348 ) ) ;
#6119 = CARTESIAN_POINT ( 'NONE',  ( 46.94469835654546586, 23.12036939723557083, 47.28539358874152043 ) ) ;
#6120 = CARTESIAN_POINT ( 'NONE',  ( 33.50134396954518223, 32.59164230456639899, 47.04930799450051637 ) ) ;
#6121 = CIRCLE ( 'NONE', #2450, 1.499999999999997780 ) ;
#6122 = ORIENTED_EDGE ( 'NONE', *, *, #23975, .T. ) ;
#6123 = CARTESIAN_POINT ( 'NONE',  ( -41.94323192092818431, 13.80701548633532560, 54.55385885333559060 ) ) ;
#6124 = FACE_OUTER_BOUND ( 'NONE', #470, .T. ) ;
#6125 = DIRECTION ( 'NONE',  ( -0.000000000000000000, -1.000000000000000000, 0.000000000000000000 ) ) ;
#6126 = SURFACE_STYLE_USAGE ( .BOTH. , #28613 ) ;
#6127 = ORIENTED_EDGE ( 'NONE', *, *, #11222, .T. ) ;
#6128 = FACE_OUTER_BOUND ( 'NONE', #19991, .T. ) ;
#6129 = DIRECTION ( 'NONE',  ( 0.000000000000000000, -0.000000000000000000, -1.000000000000000000 ) ) ;
#6130 = DIRECTION ( 'NONE',  ( -0.000000000000000000, -1.000000000000000000, -0.000000000000000000 ) ) ;
#6131 = CYLINDRICAL_SURFACE ( 'NONE', #21343, 0.9999999999999998890 ) ;
#6132 = DIRECTION ( 'NONE',  ( 1.234978253042719660E-16, -1.000000000000000000, -1.109335647967047851E-31 ) ) ;
#6133 = ORIENTED_EDGE ( 'NONE', *, *, #4782, .F. ) ;
#6134 = CARTESIAN_POINT ( 'NONE',  ( 48.59475124299144966, 29.58954579224780090, 45.61232171765963272 ) ) ;
#6135 = CYLINDRICAL_SURFACE ( 'NONE', #15322, 12.36707279061065101 ) ;
#6136 = LINE ( 'NONE', #31096, #17490 ) ;
#6137 = ORIENTED_EDGE ( 'NONE', *, *, #8490, .T. ) ;
#6138 = CARTESIAN_POINT ( 'NONE',  ( 21.09992658989238734, 30.71183152705961916, 47.04930799450051637 ) ) ;
#6139 = LINE ( 'NONE', #25996, #4165 ) ;
#6140 = CIRCLE ( 'NONE', #375, 0.1250000000000001110 ) ;
#6141 = DIRECTION ( 'NONE',  ( 0.9612616959383207815, 0.2756373558169926685, 8.795445018804291370E-19 ) ) ;
#6142 = CARTESIAN_POINT ( 'NONE',  ( 51.94105711998279418, 4.618558202237299071, -5.241157233405584925 ) ) ;
#6143 = ORIENTED_EDGE ( 'NONE', *, *, #28320, .T. ) ;
#6144 = CARTESIAN_POINT ( 'NONE',  ( 21.09785597605720753, -5.098646251524523443, 47.04930799450052348 ) ) ;
#6145 = EDGE_LOOP ( 'NONE', ( #24417, #30662, #26066, #7969 ) ) ;
#6146 = EDGE_CURVE ( 'NONE', #7677, #29646, #16732, .T. ) ;
#6147 = ORIENTED_EDGE ( 'NONE', *, *, #23092, .F. ) ;
#6148 = AXIS2_PLACEMENT_3D ( 'NONE', #28900, #23797, #26427 ) ;
#6149 = EDGE_CURVE ( 'NONE', #15078, #12341, #7837, .T. ) ;
#6150 = EDGE_CURVE ( 'NONE', #12910, #163, #18313, .T. ) ;
#6151 = CIRCLE ( 'NONE', #20822, 0.1000000000000018235 ) ;
#6152 = DIRECTION ( 'NONE',  ( 1.188208965918165239E-16, 1.880121038077813132E-16, 1.000000000000000000 ) ) ;
#6153 = CARTESIAN_POINT ( 'NONE',  ( 100.3079064823960493, -16.63545420775219696, 49.54930799450134771 ) ) ;
#6154 = CARTESIAN_POINT ( 'NONE',  ( 21.09992658989238734, 32.59164230456639899, 47.04930799450051637 ) ) ;
#6155 = EDGE_CURVE ( 'NONE', #26286, #4992, #13093, .T. ) ;
#6156 = TOROIDAL_SURFACE ( 'NONE', #17156, 12.40141737965281088, 0.1249999999999987788 ) ;
#6157 = ORIENTED_EDGE ( 'NONE', *, *, #24724, .T. ) ;
#6158 = DIRECTION ( 'NONE',  ( -1.000000000000000000, 0.000000000000000000, 0.000000000000000000 ) ) ;
#6159 = ORIENTED_EDGE ( 'NONE', *, *, #29491, .T. ) ;
#6160 = CARTESIAN_POINT ( 'NONE',  ( 45.41164638504195494, 22.93807716476589675, 46.96173444154113241 ) ) ;
#6161 = CARTESIAN_POINT ( 'NONE',  ( 21.09785597605720753, 14.86454579224779948, 47.04930799450052348 ) ) ;
#6162 = CIRCLE ( 'NONE', #22396, 12.62506659569710266 ) ;
#6163 = CARTESIAN_POINT ( 'NONE',  ( -43.37834615508418068, 1.121909970995877304, 39.44930799450052916 ) ) ;
#6164 = EDGE_LOOP ( 'NONE', ( #459, #13899 ) ) ;
#6165 = CYLINDRICAL_SURFACE ( 'NONE', #16000, 71.29999999999996874 ) ;
#6166 = DIRECTION ( 'NONE',  ( -1.101824276508909887E-16, 1.000000000000000000, -0.000000000000000000 ) ) ;
#6167 = DIRECTION ( 'NONE',  ( -1.101824276508909887E-16, 1.000000000000000000, -0.000000000000000000 ) ) ;
#6168 = ORIENTED_EDGE ( 'NONE', *, *, #20528, .T. ) ;
#6169 = CARTESIAN_POINT ( 'NONE',  ( 46.90849534498374140, 22.91413368675619111, 45.25622507561872965 ) ) ;
#6170 = CARTESIAN_POINT ( 'NONE',  ( 8.474859994195281132, 31.09143805560860585, 47.04930799450051637 ) ) ;
#6171 = TOROIDAL_SURFACE ( 'NONE', #14555, 1.524998423334081643, 0.1000000000000000056 ) ;
#6172 = CARTESIAN_POINT ( 'NONE',  ( 21.09785597605719332, -5.935454207752205669, 47.04930799450050927 ) ) ;
#6173 = CARTESIAN_POINT ( 'NONE',  ( -42.38687957179149635, 4.148162238787999279, 37.04930799450052348 ) ) ;
#6174 = CARTESIAN_POINT ( 'NONE',  ( 21.09992658989239089, 26.09164230456639899, 47.04930799450051637 ) ) ;
#6175 = ORIENTED_EDGE ( 'NONE', *, *, #27198, .T. ) ;
#6176 = CARTESIAN_POINT ( 'NONE',  ( 47.65993751833249092, 23.10527845304106620, 47.07849978535075053 ) ) ;
#6177 = CYLINDRICAL_SURFACE ( 'NONE', #30623, 12.36707279061065101 ) ;
#6178 = ORIENTED_EDGE ( 'NONE', *, *, #13247, .F. ) ;
#6179 = CARTESIAN_POINT ( 'NONE',  ( -43.97745734477487645, -5.102102110272670465, 41.67880536011271175 ) ) ;
#6180 = CARTESIAN_POINT ( 'NONE',  ( 8.474859994195281132, 31.34184655352422766, 47.04930799450051637 ) ) ;
#6181 = ORIENTED_EDGE ( 'NONE', *, *, #14388, .F. ) ;
#6182 = EDGE_LOOP ( 'NONE', ( #29548, #31097, #8929, #26099 ) ) ;
#6183 = EDGE_CURVE ( 'NONE', #32001, #25278, #8876, .T. ) ;
#6184 = AXIS2_PLACEMENT_3D ( 'NONE', #26175, #23553, #11252 ) ;
#6185 = EDGE_CURVE ( 'NONE', #17767, #25543, #2023, .T. ) ;
#6186 = VECTOR ( 'NONE', #5520, 1000.000000000000114 ) ;
#6187 = ORIENTED_EDGE ( 'NONE', *, *, #890, .F. ) ;
#6188 = AXIS2_PLACEMENT_3D ( 'NONE', #20417, #3176, #80 ) ;
#6189 = CIRCLE ( 'NONE', #11406, 12.27641737965285706 ) ;
#6190 = VECTOR ( 'NONE', #344, 1000.000000000000000 ) ;
#6191 = ORIENTED_EDGE ( 'NONE', *, *, #26529, .T. ) ;
#6192 = CARTESIAN_POINT ( 'NONE',  ( 71.49893360114316465, -5.983766253076982622, 14.98546771274981637 ) ) ;
#6193 = ADVANCED_FACE ( 'NONE', ( #11717 ), #32067, .F. ) ;
#6194 = ORIENTED_EDGE ( 'NONE', *, *, #13094, .F. ) ;
#6195 = CARTESIAN_POINT ( 'NONE',  ( 47.71481260072994246, 23.09557481883486929, 47.44955100077470433 ) ) ;
#6196 = CARTESIAN_POINT ( 'NONE',  ( 21.09785597605720753, 16.03967147762301693, 47.04930799450052348 ) ) ;
#6197 = DIRECTION ( 'NONE',  ( -1.000000000000000000, 0.000000000000000000, 0.000000000000000000 ) ) ;
#6198 = CARTESIAN_POINT ( 'NONE',  ( 48.37829923888483563, 27.45122849631043138, 45.07556196625585443 ) ) ;
#6199 = ORIENTED_EDGE ( 'NONE', *, *, #28797, .T. ) ;
#6200 = AXIS2_PLACEMENT_3D ( 'NONE', #15482, #64, #10085 ) ;
#6201 = EDGE_LOOP ( 'NONE', ( #26954, #137, #7730, #16190 ) ) ;
#6202 = DIRECTION ( 'NONE',  ( -0.000000000000000000, -1.000000000000000000, -0.000000000000000000 ) ) ;
#6203 = AXIS2_PLACEMENT_3D ( 'NONE', #9434, #27760, #342 ) ;
#6204 = ORIENTED_EDGE ( 'NONE', *, *, #22218, .F. ) ;
#6205 = DIRECTION ( 'NONE',  ( 0.000000000000000000, -0.000000000000000000, -1.000000000000000000 ) ) ;
#6206 = CIRCLE ( 'NONE', #10410, 12.36707279061065101 ) ;
#6207 = DIRECTION ( 'NONE',  ( -1.000000000000000000, 0.000000000000000000, 0.000000000000000000 ) ) ;
#6208 = FACE_OUTER_BOUND ( 'NONE', #28664, .T. ) ;
#6209 = FACE_OUTER_BOUND ( 'NONE', #17779, .T. ) ;
#6210 = TOROIDAL_SURFACE ( 'NONE', #23521, 12.40141737965288371, 0.1249999999999996253 ) ;
#6211 = CIRCLE ( 'NONE', #20876, 0.1250000000000001110 ) ;
#6212 = DIRECTION ( 'NONE',  ( -0.000000000000000000, -1.000000000000000000, 0.000000000000000000 ) ) ;
#6213 = DIRECTION ( 'NONE',  ( 0.000000000000000000, 0.000000000000000000, 1.000000000000000000 ) ) ;
#6214 = EDGE_CURVE ( 'NONE', #4827, #8205, #8368, .T. ) ;
#6215 = VERTEX_POINT ( 'NONE', #24675 ) ;
#6216 = CARTESIAN_POINT ( 'NONE',  ( 21.09785597605720042, 11.92558985988973497, -8.808602229120017668 ) ) ;
#6217 = CARTESIAN_POINT ( 'NONE',  ( 21.09785597605720753, 13.86454579224779948, 47.04930799450052348 ) ) ;
#6218 = CARTESIAN_POINT ( 'NONE',  ( -40.05987053574653345, 7.506472619680472746, 38.19144330556764544 ) ) ;
#6219 = ADVANCED_FACE ( 'NONE', ( #31742 ), #2496, .F. ) ;
#6220 = AXIS2_PLACEMENT_3D ( 'NONE', #14136, #11501, #8563 ) ;
#6221 = LINE ( 'NONE', #16223, #20558 ) ;
#6222 = CARTESIAN_POINT ( 'NONE',  ( 33.46699938050303302, 38.56284415653841791, 47.04930799450051637 ) ) ;
#6223 = ORIENTED_EDGE ( 'NONE', *, *, #5463, .T. ) ;
#6224 = CARTESIAN_POINT ( 'NONE',  ( 46.00908685603033632, 26.93284706826093000, 44.91496614357595263 ) ) ;
#6225 = VERTEX_POINT ( 'NONE', #14999 ) ;
#6226 = CARTESIAN_POINT ( 'NONE',  ( -41.92347351173194170, 13.84990507184044084, 59.52701028453313370 ) ) ;
#6227 = CARTESIAN_POINT ( 'NONE',  ( -40.67837904183828357, 9.488261090400158082, 35.45356819842893259 ) ) ;
#6228 = EDGE_CURVE ( 'NONE', #4161, #4920, #9748, .T. ) ;
#6229 = EDGE_CURVE ( 'NONE', #15830, #17244, #19880, .T. ) ;
#6230 = ADVANCED_FACE ( 'NONE', ( #19242 ), #4651, .T. ) ;
#6231 = EDGE_LOOP ( 'NONE', ( #5621, #1242, #30904, #5150 ) ) ;
#6232 = COLOUR_RGB ( '',0.7921568627450980005, 0.8196078431372548767, 0.9333333333333333481 ) ;
#6233 = CIRCLE ( 'NONE', #7812, 1.500000000000001332 ) ;
#6234 = ORIENTED_EDGE ( 'NONE', *, *, #31859, .F. ) ;
#6235 = FACE_OUTER_BOUND ( 'NONE', #32152, .T. ) ;
#6236 = EDGE_CURVE ( 'NONE', #16953, #7900, #30391, .T. ) ;
#6237 = DIRECTION ( 'NONE',  ( -1.000000000000000000, -1.101824276508909887E-16, 0.000000000000000000 ) ) ;
#6238 = DIRECTION ( 'NONE',  ( -1.101824276508909887E-16, 1.000000000000000000, -0.000000000000000000 ) ) ;
#6239 = AXIS2_PLACEMENT_3D ( 'NONE', #9501, #24587, #29526 ) ;
#6240 = ORIENTED_EDGE ( 'NONE', *, *, #24482, .F. ) ;
#6241 = DIRECTION ( 'NONE',  ( -1.000000000000000000, 0.000000000000000000, 0.000000000000000000 ) ) ;
#6242 = DIRECTION ( 'NONE',  ( -0.8746197071393805311, 0.4848096202463645921, 1.277302113040265530E-17 ) ) ;
#6243 = CARTESIAN_POINT ( 'NONE',  ( 73.18730857026689307, 5.323792735596109438, 16.63543975439153400 ) ) ;
#6244 = ORIENTED_EDGE ( 'NONE', *, *, #5412, .F. ) ;
#6245 = CARTESIAN_POINT ( 'NONE',  ( 8.474859994195281132, 32.09143805560860585, 47.04930799450051637 ) ) ;
#6246 = ORIENTED_EDGE ( 'NONE', *, *, #26861, .F. ) ;
#6247 = CARTESIAN_POINT ( 'NONE',  ( -42.48178708409979265, 14.60617548783703690, 58.99727659774876543 ) ) ;
#6248 = CARTESIAN_POINT ( 'NONE',  ( 21.09785597605720753, 13.78442380691147839, 47.04930799450052348 ) ) ;
#6249 = CARTESIAN_POINT ( 'NONE',  ( 21.09785597605719332, 25.56454579224779877, 73.04930799450052348 ) ) ;
#6250 = ADVANCED_FACE ( 'NONE', ( #6787 ), #26234, .T. ) ;
#6251 =( NAMED_UNIT ( * ) PLANE_ANGLE_UNIT ( ) SI_UNIT ( $, .RADIAN. ) );
#6252 = ORIENTED_EDGE ( 'NONE', *, *, #1550, .F. ) ;
#6253 = ORIENTED_EDGE ( 'NONE', *, *, #13094, .T. ) ;
#6254 = DIRECTION ( 'NONE',  ( -1.000000000000000000, 0.000000000000000000, 0.000000000000000000 ) ) ;
#6255 = DIRECTION ( 'NONE',  ( -1.101824276508909887E-16, 1.000000000000000000, -0.000000000000000000 ) ) ;
#6256 = AXIS2_PLACEMENT_3D ( 'NONE', #15990, #14184, #9087 ) ;
#6257 = EDGE_CURVE ( 'NONE', #1157, #6923, #31951, .T. ) ;
#6258 = CARTESIAN_POINT ( 'NONE',  ( 21.09785597605720753, 14.86454579224779948, 47.04930799450052348 ) ) ;
#6259 = VERTEX_POINT ( 'NONE', #19863 ) ;
#6260 = DIRECTION ( 'NONE',  ( -1.101824276508909887E-16, 1.000000000000000000, -0.000000000000000000 ) ) ;
#6261 = ORIENTED_EDGE ( 'NONE', *, *, #10555, .F. ) ;
#6262 = DIRECTION ( 'NONE',  ( 0.000000000000000000, 1.000000000000000000, -0.000000000000000000 ) ) ;
#6263 = CARTESIAN_POINT ( 'NONE',  ( 49.28428300279882990, 26.94787913140504543, 48.46772541801551171 ) ) ;
#6264 = EDGE_CURVE ( 'NONE', #1774, #10919, #1494, .T. ) ;
#6265 = TOROIDAL_SURFACE ( 'NONE', #23028, 12.40141737965287660, 0.1250000000000007772 ) ;
#6266 = CIRCLE ( 'NONE', #17269, 1.899999999999999023 ) ;
#6267 = DIRECTION ( 'NONE',  ( -0.000000000000000000, -1.000000000000000000, 0.000000000000000000 ) ) ;
#6268 = TOROIDAL_SURFACE ( 'NONE', #6800, 12.40141737965283220, 0.1250000000000002498 ) ;
#6269 = CIRCLE ( 'NONE', #9953, 0.1250000000000001110 ) ;
#6270 = ORIENTED_EDGE ( 'NONE', *, *, #9227, .T. ) ;
#6271 = DIRECTION ( 'NONE',  ( -1.000000000000000000, 0.000000000000000000, 0.000000000000000000 ) ) ;
#6272 = LINE ( 'NONE', #31232, #24111 ) ;
#6273 = CARTESIAN_POINT ( 'NONE',  ( 48.37829923888483563, 25.39452976649965876, 45.07556196625585443 ) ) ;
#6274 = VECTOR ( 'NONE', #3491, 1000.000000000000000 ) ;
#6275 = ORIENTED_EDGE ( 'NONE', *, *, #28637, .T. ) ;
#6276 = CARTESIAN_POINT ( 'NONE',  ( -42.03703168893574116, 3.954238390689463145, 47.04930799450051637 ) ) ;
#6277 = CARTESIAN_POINT ( 'NONE',  ( -41.07644103349281295, 9.237697617431788188, 34.64930799450051779 ) ) ;
#6278 = DIRECTION ( 'NONE',  ( -0.000000000000000000, -1.000000000000000000, 0.000000000000000000 ) ) ;
#6279 = VECTOR ( 'NONE', #22851, 1000.000000000000000 ) ;
#6280 = EDGE_LOOP ( 'NONE', ( #25294, #28340, #32270, #3495 ) ) ;
#6281 = AXIS2_PLACEMENT_3D ( 'NONE', #20040, #27756, #9716 ) ;
#6282 = CARTESIAN_POINT ( 'NONE',  ( 21.09992658989239089, 28.34143805560861296, 47.04930799450051637 ) ) ;
#6283 = CARTESIAN_POINT ( 'NONE',  ( -40.61574147496721565, 7.605736927813537385, 53.92359549476551450 ) ) ;
#6284 = LINE ( 'NONE', #3981, #537 ) ;
#6285 = CARTESIAN_POINT ( 'NONE',  ( 44.87087493598345134, 25.37587066347689913, 48.18533415931919706 ) ) ;
#6286 = CARTESIAN_POINT ( 'NONE',  ( 0.000000000000000000, 0.000000000000000000, 0.000000000000000000 ) ) ;
#6287 = ORIENTED_EDGE ( 'NONE', *, *, #14382, .T. ) ;
#6288 = CIRCLE ( 'NONE', #4730, 48.97546517713167447 ) ;
#6289 = CARTESIAN_POINT ( 'NONE',  ( -40.02540636251513462, 2.839176264122873050, 37.04930799450052348 ) ) ;
#6290 = CARTESIAN_POINT ( 'NONE',  ( 45.79384627280941089, 27.77957786121581663, 49.05938063676250493 ) ) ;
#6291 = CARTESIAN_POINT ( 'NONE',  ( 81.63175399755476747, -5.935454207809698346, 78.02743327247107175 ) ) ;
#6292 = CARTESIAN_POINT ( 'NONE',  ( -40.11902961310587301, 6.880801488287905165, 34.57491199848074359 ) ) ;
#6293 = CARTESIAN_POINT ( 'NONE',  ( 8.823509210239569356, 30.09164230456639544, 47.04930799450051637 ) ) ;
#6294 = ORIENTED_EDGE ( 'NONE', *, *, #5049, .T. ) ;
#6295 =( BOUNDED_CURVE ( )  B_SPLINE_CURVE ( 2, ( #23394, #20921, #8768, #3038, #901, #10617, #20606, #10927, #18460 ),
 .UNSPECIFIED., .F., .T. ) 
 B_SPLINE_CURVE_WITH_KNOTS ( ( 3, 2, 2, 2, 3 ),
 ( 0.4642857131244416125, 0.4761904761904761640, 0.5000000000000000000, 0.5238095238095238360, 0.5357142845530131758 ),
 .UNSPECIFIED. ) 
 CURVE ( )  GEOMETRIC_REPRESENTATION_ITEM ( )  RATIONAL_B_SPLINE_CURVE ( ( 0.9330127018922199644, 0.9330126953578159466, 1.000000000000000000, 0.8660254037844387076, 1.000000000000000000, 0.8660254037844387076, 1.000000000000000000, 0.9330127084266224280, 0.9330127018922200755 ) ) 
 REPRESENTATION_ITEM ( '' )  );
#6296 = DIRECTION ( 'NONE',  ( -1.224646799147353207E-16, 0.000000000000000000, -1.000000000000000000 ) ) ;
#6297 = CARTESIAN_POINT ( 'NONE',  ( 21.09785597605720753, -16.03545420775220265, 116.6483275080933169 ) ) ;
#6298 = FACE_OUTER_BOUND ( 'NONE', #500, .T. ) ;
#6299 = ORIENTED_EDGE ( 'NONE', *, *, #29258, .T. ) ;
#6300 = FACE_OUTER_BOUND ( 'NONE', #19576, .T. ) ;
#6301 = CARTESIAN_POINT ( 'NONE',  ( 0.6836613156275053171, 11.92558985988973497, 132.0493079945005377 ) ) ;
#6302 = CIRCLE ( 'NONE', #27794, 20.13652856819611969 ) ;
#6303 = CARTESIAN_POINT ( 'NONE',  ( -40.50410981870283678, 7.604537000166497585, 38.76008276981544753 ) ) ;
#6304 = EDGE_CURVE ( 'NONE', #19672, #24538, #4449, .T. ) ;
#6305 = VERTEX_POINT ( 'NONE', #6912 ) ;
#6306 = CARTESIAN_POINT ( 'NONE',  ( 72.77034215320227872, 11.18784031540631574, 22.82302068831501884 ) ) ;
#6307 = ORIENTED_EDGE ( 'NONE', *, *, #15631, .F. ) ;
#6308 = AXIS2_PLACEMENT_3D ( 'NONE', #28540, #21779, #31162 ) ;
#6309 = VECTOR ( 'NONE', #30634, 1000.000000000000114 ) ;
#6310 = ORIENTED_EDGE ( 'NONE', *, *, #29829, .T. ) ;
#6311 = VECTOR ( 'NONE', #15099, 1000.000000000000227 ) ;
#6312 = CIRCLE ( 'NONE', #28854, 12.62506659569710266 ) ;
#6313 = VECTOR ( 'NONE', #19241, 1000.000000000000000 ) ;
#6314 = COLOUR_RGB ( '',0.7921568627450980005, 0.8196078431372548767, 0.9333333333333333481 ) ;
#6315 = DIRECTION ( 'NONE',  ( -1.000000000000000000, -1.101824276508909887E-16, 0.000000000000000000 ) ) ;
#6316 = DIRECTION ( 'NONE',  ( -1.000000000000000000, 0.000000000000000000, 0.000000000000000000 ) ) ;
#6317 = DIRECTION ( 'NONE',  ( -1.000000000000000000, 0.000000000000000000, 0.000000000000000000 ) ) ;
#6318 = CIRCLE ( 'NONE', #25735, 0.1250000000000001110 ) ;
#6319 = ORIENTED_EDGE ( 'NONE', *, *, #10123, .T. ) ;
#6320 = FACE_OUTER_BOUND ( 'NONE', #26532, .T. ) ;
#6321 = ORIENTED_EDGE ( 'NONE', *, *, #14947, .T. ) ;
#6322 = FACE_OUTER_BOUND ( 'NONE', #14016, .T. ) ;
#6323 = FACE_OUTER_BOUND ( 'NONE', #21519, .T. ) ;
#6324 = DIRECTION ( 'NONE',  ( -0.9612616959383200044, -0.2756373558169956106, -8.795445018804684260E-19 ) ) ;
#6325 = EDGE_LOOP ( 'NONE', ( #23278, #9581, #21890, #31152 ) ) ;
#6326 = CARTESIAN_POINT ( 'NONE',  ( -41.77464577679392477, 3.808795504615560379, 47.04930799450051637 ) ) ;
#6327 = DIRECTION ( 'NONE',  ( -1.101824276508909887E-16, 1.000000000000000000, -0.000000000000000000 ) ) ;
#6328 = CARTESIAN_POINT ( 'NONE',  ( 79.37786958444415575, -5.721341737285090545, 15.14745076809877133 ) ) ;
#6329 = CARTESIAN_POINT ( 'NONE',  ( 45.41164638504195494, 22.93807716476589675, 46.96173444154113241 ) ) ;
#6330 = ORIENTED_EDGE ( 'NONE', *, *, #18728, .T. ) ;
#6331 = FACE_OUTER_BOUND ( 'NONE', #21498, .T. ) ;
#6332 = AXIS2_PLACEMENT_3D ( 'NONE', #15383, #28182, #15869 ) ;
#6333 = DIRECTION ( 'NONE',  ( -1.101824276508909887E-16, 1.000000000000000000, -0.000000000000000000 ) ) ;
#6334 = DIRECTION ( 'NONE',  ( -1.101824276508909887E-16, 1.000000000000000000, -0.000000000000000000 ) ) ;
#6335 = DIRECTION ( 'NONE',  ( -1.101824276508909887E-16, 1.000000000000000000, -0.000000000000000000 ) ) ;
#6336 = VERTEX_POINT ( 'NONE', #17075 ) ;
#6337 = VECTOR ( 'NONE', #30692, 1000.000000000000000 ) ;
#6338 = DIRECTION ( 'NONE',  ( 1.000000000000000000, 0.000000000000000000, 0.000000000000000000 ) ) ;
#6339 = DIRECTION ( 'NONE',  ( -0.000000000000000000, -1.000000000000000000, 0.000000000000000000 ) ) ;
#6340 = CIRCLE ( 'NONE', #13169, 0.1000000000000028644 ) ;
#6341 = ORIENTED_EDGE ( 'NONE', *, *, #8229, .T. ) ;
#6342 = CONICAL_SURFACE ( 'NONE', #10551, 0.9031915329475500576, 0.7853981633974548293 ) ;
#6343 = AXIS2_PLACEMENT_3D ( 'NONE', #15027, #7799, #20258 ) ;
#6344 = DIRECTION ( 'NONE',  ( -1.000000000000000000, 0.000000000000000000, 0.000000000000000000 ) ) ;
#6345 = ADVANCED_FACE ( 'NONE', ( #14471 ), #17807, .T. ) ;
#6346 = EDGE_CURVE ( 'NONE', #16617, #2537, #21985, .T. ) ;
#6347 = ORIENTED_EDGE ( 'NONE', *, *, #744, .T. ) ;
#6348 = ADVANCED_FACE ( 'NONE', ( #4779 ), #24465, .T. ) ;
#6349 = VERTEX_POINT ( 'NONE', #19204 ) ;
#6350 = ADVANCED_FACE ( 'NONE', ( #1659 ), #8327, .F. ) ;
#6351 = EDGE_CURVE ( 'NONE', #22098, #15469, #9212, .T. ) ;
#6352 = VERTEX_POINT ( 'NONE', #19699 ) ;
#6353 = AXIS2_PLACEMENT_3D ( 'NONE', #12902, #19938, #25032 ) ;
#6354 = ORIENTED_EDGE ( 'NONE', *, *, #20840, .T. ) ;
#6355 = AXIS2_PLACEMENT_3D ( 'NONE', #7636, #12730, #17628 ) ;
#6356 = DIRECTION ( 'NONE',  ( 0.8746197071393925215, -0.4848096202463429982, -8.676864087101708112E-18 ) ) ;
#6357 = APPLICATION_CONTEXT ( 'automotive_design' ) ;
#6358 = AXIS2_PLACEMENT_3D ( 'NONE', #20935, #10630, #30967 ) ;
#6359 = CIRCLE ( 'NONE', #17295, 0.1249999999999983763 ) ;
#6360 = ORIENTED_EDGE ( 'NONE', *, *, #3107, .F. ) ;
#6361 = CYLINDRICAL_SURFACE ( 'NONE', #20014, 12.36707279061065101 ) ;
#6362 = CARTESIAN_POINT ( 'NONE',  ( 21.09785597605719332, 25.56454579224779877, 23.54930799450051637 ) ) ;
#6363 = CARTESIAN_POINT ( 'NONE',  ( 21.09785597605719332, 17.16451738380053627, 47.04930799450051637 ) ) ;
#6364 = CARTESIAN_POINT ( 'NONE',  ( -40.50726676055796105, 7.559560307024983494, 53.80788663826320573 ) ) ;
#6365 = CARTESIAN_POINT ( 'NONE',  ( 47.20353132263855400, 26.85286309983298025, 45.01455027646041174 ) ) ;
#6366 = EDGE_CURVE ( 'NONE', #25938, #31872, #16687, .T. ) ;
#6367 = ORIENTED_EDGE ( 'NONE', *, *, #26978, .T. ) ;
#6368 = ORIENTED_EDGE ( 'NONE', *, *, #820, .T. ) ;
#6369 = FACE_OUTER_BOUND ( 'NONE', #8986, .T. ) ;
#6370 = AXIS2_PLACEMENT_3D ( 'NONE', #30165, #3382, #23412 ) ;
#6371 = ADVANCED_FACE ( 'NONE', ( #14795 ), #328, .T. ) ;
#6372 = ORIENTED_EDGE ( 'NONE', *, *, #13912, .T. ) ;
#6373 = DIRECTION ( 'NONE',  ( 0.000000000000000000, 0.000000000000000000, -1.000000000000000000 ) ) ;
#6374 = DIRECTION ( 'NONE',  ( -0.4848096202463429982, -0.8746197071393925215, -9.920727850371698576E-18 ) ) ;
#6375 = DIRECTION ( 'NONE',  ( -0.000000000000000000, -1.000000000000000000, 0.000000000000000000 ) ) ;
#6376 = CARTESIAN_POINT ( 'NONE',  ( 44.09250526802607340, 27.35621246473837331, 46.89322480343881949 ) ) ;
#6377 = CARTESIAN_POINT ( 'NONE',  ( 48.89639543821420631, 22.86454579224779948, 46.17372366037167097 ) ) ;
#6378 = CARTESIAN_POINT ( 'NONE',  ( 21.09785597605719332, 17.16451738380053627, 59.73344952167762756 ) ) ;
#6379 = EDGE_LOOP ( 'NONE', ( #12720, #25399, #4185, #71 ) ) ;
#6380 = CARTESIAN_POINT ( 'NONE',  ( 21.09785597605720753, 14.86454579224779948, 47.04930799450052348 ) ) ;
#6381 = FACE_BOUND ( 'NONE', #16204, .T. ) ;
#6382 = DIRECTION ( 'NONE',  ( -0.2603858710390614672, 0.9080734476337354311, 0.3280271511107134552 ) ) ;
#6383 = AXIS2_PLACEMENT_3D ( 'NONE', #2219, #2539, #17633 ) ;
#6384 = DIRECTION ( 'NONE',  ( 0.000000000000000000, 0.000000000000000000, 1.000000000000000000 ) ) ;
#6385 = VERTEX_POINT ( 'NONE', #7728 ) ;
#6386 = DIRECTION ( 'NONE',  ( 1.000000000000000000, 0.000000000000000000, 0.000000000000000000 ) ) ;
#6387 = ORIENTED_EDGE ( 'NONE', *, *, #25885, .F. ) ;
#6388 = LINE ( 'NONE', #13783, #28855 ) ;
#6389 = DIRECTION ( 'NONE',  ( -1.000000000000000000, 0.000000000000000000, 0.000000000000000000 ) ) ;
#6390 = EDGE_CURVE ( 'NONE', #11991, #14790, #14087, .T. ) ;
#6391 = VERTEX_POINT ( 'NONE', #25600 ) ;
#6392 = CIRCLE ( 'NONE', #27365, 12.62506659569710266 ) ;
#6393 = CIRCLE ( 'NONE', #24814, 12.27641737965280555 ) ;
#6394 = ORIENTED_EDGE ( 'NONE', *, *, #15635, .T. ) ;
#6395 = ADVANCED_FACE ( 'NONE', ( #5585 ), #10518, .T. ) ;
#6396 = CARTESIAN_POINT ( 'NONE',  ( 21.09992658989238734, 31.84143805560860940, 47.04930799450051637 ) ) ;
#6397 = DIRECTION ( 'NONE',  ( 0.000000000000000000, 0.5219656503457801300, -0.8529665057076430967 ) ) ;
#6398 = CARTESIAN_POINT ( 'NONE',  ( -44.16105795751995799, -3.935454207752183020, 52.04930799450050927 ) ) ;
#6400 = EDGE_CURVE ( 'NONE', #32220, #26256, #27172, .T. ) ;
#6399 = VECTOR ( 'NONE', #14933, 1000.000000000000114 ) ;
#6401 = VERTEX_POINT ( 'NONE', #8059 ) ;
#6402 = CARTESIAN_POINT ( 'NONE',  ( 21.09785597605719332, 7.094379510609982731, 27.72953811535153079 ) ) ;
#6403 = AXIS2_PLACEMENT_3D ( 'NONE', #9822, #15073, #19819 ) ;
#6404 = CARTESIAN_POINT ( 'NONE',  ( 21.09992658989239089, 28.72145308207318237, 47.04930799450051637 ) ) ;
#6405 = EDGE_CURVE ( 'NONE', #28677, #11490, #3577, .T. ) ;
#6406 = VERTEX_POINT ( 'NONE', #24961 ) ;
#6407 = DIRECTION ( 'NONE',  ( -1.101824276508909887E-16, 1.000000000000000000, -0.000000000000000000 ) ) ;
#6408 = EDGE_CURVE ( 'NONE', #18864, #9903, #18050, .T. ) ;
#6409 = VERTEX_POINT ( 'NONE', #27425 ) ;
#6410 = EDGE_CURVE ( 'NONE', #29883, #4784, #24548, .T. ) ;
#6411 = CARTESIAN_POINT ( 'NONE',  ( -42.41019933908752648, 14.71530103803245915, 58.95721942880052779 ) ) ;
#6412 = CARTESIAN_POINT ( 'NONE',  ( 48.23388202445966755, 15.77906836436399374, 49.27628909396055690 ) ) ;
#6413 = PRODUCT_DEFINITION_SHAPE ( 'NONE', 'NONE',  #32502 ) ;
#6414 = CARTESIAN_POINT ( 'NONE',  ( -40.61463551858322063, 9.441168033762318501, 38.61901908761456781 ) ) ;
#6415 =( NAMED_UNIT ( * ) SI_UNIT ( $, .STERADIAN. ) SOLID_ANGLE_UNIT ( ) );
#6416 = VERTEX_POINT ( 'NONE', #30373 ) ;
#6417 = EDGE_LOOP ( 'NONE', ( #3636, #26328, #26977, #14469 ) ) ;
#6418 = DIRECTION ( 'NONE',  ( -1.000000000000000000, 0.000000000000000000, 0.000000000000000000 ) ) ;
#6419 = DIRECTION ( 'NONE',  ( 0.000000000000000000, 3.761114140369702165E-15, -1.000000000000000000 ) ) ;
#6420 = DIRECTION ( 'NONE',  ( -1.000000000000000000, 0.000000000000000000, 0.000000000000000000 ) ) ;
#6421 = CIRCLE ( 'NONE', #5915, 0.1249999999999983763 ) ;
#6422 = EDGE_LOOP ( 'NONE', ( #24764, #11832 ) ) ;
#6423 = CARTESIAN_POINT ( 'NONE',  ( 21.09992658989238734, 31.09184655352422411, 47.04930799450051637 ) ) ;
#6424 = LINE ( 'NONE', #1165, #28290 ) ;
#6425 = CIRCLE ( 'NONE', #6960, 1.199999999999999734 ) ;
#6426 = ORIENTED_EDGE ( 'NONE', *, *, #7421, .T. ) ;
#6427 = CARTESIAN_POINT ( 'NONE',  ( 33.72499318558949000, 38.56284415653841791, 47.04930799450051637 ) ) ;
#6428 = CARTESIAN_POINT ( 'NONE',  ( 45.46000861347822308, 28.87287913140503548, 49.57397645940629616 ) ) ;
#6429 = ADVANCED_FACE ( 'NONE', ( #17894 ), #3102, .T. ) ;
#6430 = CIRCLE ( 'NONE', #10645, 12.36707279061065101 ) ;
#6431 = CARTESIAN_POINT ( 'NONE',  ( -35.50889619860521407, 10.17704670261596966, 52.04930799450050927 ) ) ;
#6432 = AXIS2_PLACEMENT_3D ( 'NONE', #31461, #29312, #12087 ) ;
#6433 = ORIENTED_EDGE ( 'NONE', *, *, #5712, .F. ) ;
#6434 = DIRECTION ( 'NONE',  ( -1.000000000000000000, -0.000000000000000000, -3.491481338843133355E-15 ) ) ;
#6435 = EDGE_CURVE ( 'NONE', #23854, #116, #17724, .T. ) ;
#6436 = CARTESIAN_POINT ( 'NONE',  ( -40.49636040740121956, 6.939949491715667662, 39.44930799450052206 ) ) ;
#6437 = DIRECTION ( 'NONE',  ( 0.4848096202463673676, 0.8746197071393789768, 0.000000000000000000 ) ) ;
#6438 = CARTESIAN_POINT ( 'NONE',  ( 48.37829923888483563, 26.09452976649965450, 45.07556196625585443 ) ) ;
#6439 = EDGE_CURVE ( 'NONE', #29925, #32344, #31379, .T. ) ;
#6440 = ORIENTED_EDGE ( 'NONE', *, *, #22675, .T. ) ;
#6441 = AXIS2_PLACEMENT_3D ( 'NONE', #1437, #6375, #26396 ) ;
#6442 = LINE ( 'NONE', #26460, #18035 ) ;
#6444 = CARTESIAN_POINT ( 'NONE',  ( 33.72499318558949710, 26.59143805560860940, 47.04930799450051637 ) ) ;
#6443 = AXIS2_PLACEMENT_3D ( 'NONE', #20493, #30520, #13121 ) ;
#6445 = CARTESIAN_POINT ( 'NONE',  ( 71.55936645880203173, 9.702389020015065313, 20.34850893876554423 ) ) ;
#6446 = EDGE_CURVE ( 'NONE', #15214, #18631, #29260, .T. ) ;
#6447 = DIRECTION ( 'NONE',  ( 0.2756373558169932236, -0.9612616959383206705, 1.479773560108267395E-16 ) ) ;
#6448 = EDGE_CURVE ( 'NONE', #7700, #27037, #10193, .T. ) ;
#6449 = CYLINDRICAL_SURFACE ( 'NONE', #26205, 1.000000000000000666 ) ;
#6450 = CARTESIAN_POINT ( 'NONE',  ( 21.09785597605719332, 6.574714862014670480, 47.04930799450051637 ) ) ;
#6451 = AXIS2_PLACEMENT_3D ( 'NONE', #7320, #27342, #22399 ) ;
#6452 = AXIS2_PLACEMENT_3D ( 'NONE', #9981, #22925, #19981 ) ;
#6453 = DIRECTION ( 'NONE',  ( -0.000000000000000000, -1.000000000000000000, -0.000000000000000000 ) ) ;
#6454 = VERTEX_POINT ( 'NONE', #15112 ) ;
#6455 = CARTESIAN_POINT ( 'NONE',  ( 8.698509210239549816, 28.34164230456639544, 47.04930799450051637 ) ) ;
#6456 = CARTESIAN_POINT ( 'NONE',  ( 47.20547626766765603, 28.18791119454915162, 44.97710074790751378 ) ) ;
#6457 = B_SPLINE_CURVE_WITH_KNOTS ( 'NONE', 3,
 ( #20586, #23374, #25832, #23214, #30453, #15828, #731, #15658, #5500, #5652 ),
 .UNSPECIFIED., .F., .F.,
 ( 4, 2, 2, 2, 4 ),
 ( 0.000000000000000000, 0.0002984299662232473113, 0.0005968599324464946227, 0.0008952898986697419882, 0.001193719864892989245 ),
 .UNSPECIFIED. ) ;
#6458 = CARTESIAN_POINT ( 'NONE',  ( 81.57562808514117592, -5.935708903123444458, 78.02297485689277323 ) ) ;
#6459 = DIRECTION ( 'NONE',  ( -1.000000000000000000, 0.000000000000000000, 0.000000000000000000 ) ) ;
#6460 = DIRECTION ( 'NONE',  ( -1.000000000000000000, 0.000000000000000000, 0.000000000000000000 ) ) ;
#6461 = ORIENTED_EDGE ( 'NONE', *, *, #221, .F. ) ;
#6462 = CARTESIAN_POINT ( 'NONE',  ( -43.64647580959332629, 1.256990871545143440, 53.64930799450051779 ) ) ;
#6463 = CARTESIAN_POINT ( 'NONE',  ( -40.23847960489091946, 6.935107575317837281, 39.46395734157443513 ) ) ;
#6464 = DIRECTION ( 'NONE',  ( -1.101824276508909887E-16, 1.000000000000000000, -0.000000000000000000 ) ) ;
#6465 = ORIENTED_EDGE ( 'NONE', *, *, #11344, .T. ) ;
#6466 = CARTESIAN_POINT ( 'NONE',  ( -42.22138300640814634, 14.68176690255379491, 38.19144330556764544 ) ) ;
#6467 = CARTESIAN_POINT ( 'NONE',  ( 21.09992658989239089, 26.21664230456639899, 47.04930799450051637 ) ) ;
#6468 = CARTESIAN_POINT ( 'NONE',  ( -43.86882709718853590, -0.1754741395363378920, 62.04930799450052348 ) ) ;
#6469 = CARTESIAN_POINT ( 'NONE',  ( 49.52052953415556402, 8.310461108307681144, 97.45038561958638468 ) ) ;
#6470 = AXIS2_PLACEMENT_3D ( 'NONE', #32138, #30005, #27535 ) ;
#6471 = ORIENTED_EDGE ( 'NONE', *, *, #14198, .T. ) ;
#6472 = CARTESIAN_POINT ( 'NONE',  ( 47.53612098953208687, 29.43843285659984943, 49.23711617065869461 ) ) ;
#6473 = EDGE_LOOP ( 'NONE', ( #3732, #4994, #23188, #17455 ) ) ;
#6474 = CIRCLE ( 'NONE', #29002, 2.500000000000002220 ) ;
#6475 = EDGE_LOOP ( 'NONE', ( #5388, #11403, #4367, #2211 ) ) ;
#6476 = CIRCLE ( 'NONE', #18528, 0.1000000000000018235 ) ;
#6477 = AXIS2_PLACEMENT_3D ( 'NONE', #22767, #7523, #443 ) ;
#6478 = DIRECTION ( 'NONE',  ( -1.000000000000000000, 0.000000000000000000, 0.000000000000000000 ) ) ;
#6479 = CARTESIAN_POINT ( 'NONE',  ( -32.17061786723157724, -0.8103308248208600517, 80.53195812376419838 ) ) ;
#6480 = DIRECTION ( 'NONE',  ( 0.000000000000000000, 0.000000000000000000, -1.000000000000000000 ) ) ;
#6481 = EDGE_CURVE ( 'NONE', #15416, #14823, #17204, .T. ) ;
#6482 = EDGE_LOOP ( 'NONE', ( #11460, #1704, #15754, #19240 ) ) ;
#6483 = DIRECTION ( 'NONE',  ( 0.000000000000000000, 0.000000000000000000, -1.000000000000000000 ) ) ;
#6484 = ORIENTED_EDGE ( 'NONE', *, *, #20274, .F. ) ;
#6485 = ADVANCED_FACE ( 'NONE', ( #14956 ), #25443, .F. ) ;
#6486 = AXIS2_PLACEMENT_3D ( 'NONE', #23191, #23354, #10735 ) ;
#6487 = EDGE_CURVE ( 'NONE', #16617, #5692, #6206, .T. ) ;
#6488 = CYLINDRICAL_SURFACE ( 'NONE', #5768, 0.1000000000000028644 ) ;
#6489 = CARTESIAN_POINT ( 'NONE',  ( -0.4050397648088443492, 11.88159288520707690, 98.63211136878676655 ) ) ;
#6490 = ORIENTED_EDGE ( 'NONE', *, *, #32117, .T. ) ;
#6491 = DIRECTION ( 'NONE',  ( -1.101824276508909887E-16, 1.000000000000000000, -0.000000000000000000 ) ) ;
#6492 = CARTESIAN_POINT ( 'NONE',  ( 34.39963999142011630, 17.16474120167318418, 47.04930799450052348 ) ) ;
#6493 = DIRECTION ( 'NONE',  ( 7.539678551159015339E-17, -0.7880107536067239016, 0.6156614753256557382 ) ) ;
#6494 = CARTESIAN_POINT ( 'NONE',  ( 8.474859994195286461, 26.09184655352419213, 47.04930799450051637 ) ) ;
#6495 = ORIENTED_EDGE ( 'NONE', *, *, #9867, .T. ) ;
#6496 = CARTESIAN_POINT ( 'NONE',  ( -42.47434154250543514, 4.196643200812633978, 37.04930799450052348 ) ) ;
#6497 = DIRECTION ( 'NONE',  ( 0.1949050434465282866, -0.6797146636928672603, 0.7071067811865470176 ) ) ;
#6498 = DIRECTION ( 'NONE',  ( -1.101824276508909887E-16, 1.000000000000000000, -0.000000000000000000 ) ) ;
#6499 = DIRECTION ( 'NONE',  ( 0.000000000000000000, 3.759183808608825436E-15, -1.000000000000000000 ) ) ;
#6500 = CIRCLE ( 'NONE', #7562, 12.00000000000000355 ) ;
#6501 = CARTESIAN_POINT ( 'NONE',  ( 21.09785597605720753, 13.86454579224779948, 47.04930799450052348 ) ) ;
#6502 = ORIENTED_EDGE ( 'NONE', *, *, #29120, .F. ) ;
#6503 = FACE_OUTER_BOUND ( 'NONE', #25846, .T. ) ;
#6504 = FACE_OUTER_BOUND ( 'NONE', #11847, .T. ) ;
#6505 = ORIENTED_EDGE ( 'NONE', *, *, #22067, .T. ) ;
#6506 = DIRECTION ( 'NONE',  ( -0.8746197071393926326, 0.4848096202463430537, 8.676864087101709653E-18 ) ) ;
#6507 = DIRECTION ( 'NONE',  ( -1.101824276508909887E-16, 1.000000000000000000, -0.000000000000000000 ) ) ;
#6508 = VERTEX_POINT ( 'NONE', #15430 ) ;
#6509 = ORIENTED_EDGE ( 'NONE', *, *, #27057, .F. ) ;
#6510 = UNCERTAINTY_MEASURE_WITH_UNIT (LENGTH_MEASURE( 1.000000000000000082E-05 ), #21204, 'distance_accuracy_value', 'NONE');
#6511 = ORIENTED_EDGE ( 'NONE', *, *, #15358, .F. ) ;
#6512 = TOROIDAL_SURFACE ( 'NONE', #26419, 1.899999999999999467, 0.1000000000000000056 ) ;
#6513 = AXIS2_PLACEMENT_3D ( 'NONE', #28646, #3696, #6928 ) ;
#6514 = CIRCLE ( 'NONE', #6593, 55.67821551822382276 ) ;
#6515 = AXIS2_PLACEMENT_3D ( 'NONE', #10041, #20203, #182 ) ;
#6516 = CARTESIAN_POINT ( 'NONE',  ( -41.61831254958298132, 11.12742816935064560, 38.19144330556764544 ) ) ;
#6517 = ADVANCED_FACE ( 'NONE', ( #2796 ), #7367, .T. ) ;
#6518 = ORIENTED_EDGE ( 'NONE', *, *, #16373, .T. ) ;
#6519 = DIRECTION ( 'NONE',  ( -1.000000000000000000, 0.000000000000000000, 0.000000000000000000 ) ) ;
#6520 = EDGE_CURVE ( 'NONE', #19129, #23289, #28748, .T. ) ;
#6521 = EDGE_CURVE ( 'NONE', #26418, #10913, #6071, .T. ) ;
#6522 = DIRECTION ( 'NONE',  ( -1.101824276508909887E-16, 1.000000000000000000, -0.000000000000000000 ) ) ;
#6523 = EDGE_CURVE ( 'NONE', #6567, #24849, #20889, .T. ) ;
#6524 = DIRECTION ( 'NONE',  ( -1.000000000000000000, 0.000000000000000000, 0.000000000000000000 ) ) ;
#6525 = CARTESIAN_POINT ( 'NONE',  ( 21.09785597605720042, -13.64309448858209528, 47.04930799450051637 ) ) ;
#6526 = EDGE_CURVE ( 'NONE', #22606, #9420, #15644, .T. ) ;
#6527 = EDGE_CURVE ( 'NONE', #17250, #31644, #20993, .T. ) ;
#6528 = CARTESIAN_POINT ( 'NONE',  ( 45.28286642839709231, 29.88619643316631524, 47.97516931882780966 ) ) ;
#6529 = ORIENTED_EDGE ( 'NONE', *, *, #18874, .F. ) ;
#6530 = ORIENTED_EDGE ( 'NONE', *, *, #5320, .T. ) ;
#6531 = CARTESIAN_POINT ( 'NONE',  ( -12.63166379481645585, -2.284241381456149078, -7.028544075678079039 ) ) ;
#6532 = EDGE_LOOP ( 'NONE', ( #21168, #6426, #3132, #10164 ) ) ;
#6533 = CARTESIAN_POINT ( 'NONE',  ( -41.01929587258828747, 9.401204285752058354, 35.44930799450052206 ) ) ;
#6534 = FACE_OUTER_BOUND ( 'NONE', #10532, .T. ) ;
#6535 = DIRECTION ( 'NONE',  ( 1.000000000000000000, 0.000000000000000000, 0.000000000000000000 ) ) ;
#6536 = DIRECTION ( 'NONE',  ( -1.000000000000000000, 0.000000000000000000, 0.000000000000000000 ) ) ;
#6537 = CARTESIAN_POINT ( 'NONE',  ( 45.46000861347822308, 26.77287913140504116, 49.57397645940629616 ) ) ;
#6538 = AXIS2_PLACEMENT_3D ( 'NONE', #1468, #6242, #9026 ) ;
#6539 = DIRECTION ( 'NONE',  ( 0.000000000000000000, 1.000000000000000000, -0.000000000000000000 ) ) ;
#6540 = LINE ( 'NONE', #19647, #32142 ) ;
#6541 = AXIS2_PLACEMENT_3D ( 'NONE', #17093, #7588, #27111 ) ;
#6542 = ORIENTED_EDGE ( 'NONE', *, *, #303, .F. ) ;
#6543 = CARTESIAN_POINT ( 'NONE',  ( 21.09785597605718621, 6.547041198165487685, 67.43013672359793986 ) ) ;
#6544 = DIRECTION ( 'NONE',  ( 0.2029548553014545453, 0.9702957262759968060, 0.1316644609608131067 ) ) ;
#6545 = CIRCLE ( 'NONE', #4454, 22.50178251985260758 ) ;
#6546 = DIRECTION ( 'NONE',  ( 0.000000000000000000, 0.000000000000000000, -1.000000000000000000 ) ) ;
#6547 = VECTOR ( 'NONE', #9706, 1000.000000000000114 ) ;
#6548 = AXIS2_PLACEMENT_3D ( 'NONE', #30515, #18653, #15891 ) ;
#6549 = CARTESIAN_POINT ( 'NONE',  ( 48.82187354100420151, 22.88065857334294861, 46.16985335424440251 ) ) ;
#6550 = DIRECTION ( 'NONE',  ( 0.000000000000000000, -1.000000000000000000, 0.000000000000000000 ) ) ;
#6551 = ORIENTED_EDGE ( 'NONE', *, *, #21432, .T. ) ;
#6552 = DIRECTION ( 'NONE',  ( 7.588956326749211550E-18, -4.206627182996911684E-18, 1.000000000000000000 ) ) ;
#6553 = EDGE_LOOP ( 'NONE', ( #30381, #20640, #5436, #425 ) ) ;
#6554 = FACE_OUTER_BOUND ( 'NONE', #5130, .T. ) ;
#6555 = CARTESIAN_POINT ( 'NONE',  ( 21.09992658989238734, 38.56284415653841791, 47.04930799450051637 ) ) ;
#6556 = EDGE_LOOP ( 'NONE', ( #12790, #10963, #28604, #25017 ) ) ;
#6557 = EDGE_CURVE ( 'NONE', #7574, #4462, #8415, .T. ) ;
#6558 = AXIS2_PLACEMENT_3D ( 'NONE', #22788, #13443, #15562 ) ;
#6559 = ORIENTED_EDGE ( 'NONE', *, *, #5755, .T. ) ;
#6560 = AXIS2_PLACEMENT_3D ( 'NONE', #27929, #26102, #31045 ) ;
#6561 = DIRECTION ( 'NONE',  ( -1.000000000000000000, 0.000000000000000000, 0.000000000000000000 ) ) ;
#6562 = CARTESIAN_POINT ( 'NONE',  ( 21.09785597605719687, 40.56454579224779877, 30.04930799450051282 ) ) ;
#6564 = DIRECTION ( 'NONE',  ( 1.000000000000000000, 0.000000000000000000, 0.000000000000000000 ) ) ;
#6563 = AXIS2_PLACEMENT_3D ( 'NONE', #27326, #20096, #4845 ) ;
#6565 = AXIS2_PLACEMENT_3D ( 'NONE', #10747, #7792, #13047 ) ;
#6566 = VECTOR ( 'NONE', #2210, 1000.000000000000000 ) ;
#6567 = VERTEX_POINT ( 'NONE', #26248 ) ;
#6568 = CARTESIAN_POINT ( 'NONE',  ( -40.32034427004700916, 8.384459687302960873, 54.64930799450051779 ) ) ;
#6569 = EDGE_CURVE ( 'NONE', #7978, #21737, #4640, .T. ) ;
#6570 = DIRECTION ( 'NONE',  ( -0.000000000000000000, -1.000000000000000000, 0.000000000000000000 ) ) ;
#6571 = CARTESIAN_POINT ( 'NONE',  ( 75.81187038318674354, -1.761407059904347649, 13.37723125802458490 ) ) ;
#6572 = ADVANCED_FACE ( 'NONE', ( #18842 ), #31022, .F. ) ;
#6573 = EDGE_LOOP ( 'NONE', ( #17580, #13110 ) ) ;
#6574 = DIRECTION ( 'NONE',  ( -1.101824276508909887E-16, 1.000000000000000000, -0.000000000000000000 ) ) ;
#6575 = EDGE_LOOP ( 'NONE', ( #28199, #7165, #2695, #24685 ) ) ;
#6576 = CARTESIAN_POINT ( 'NONE',  ( 21.09785597605719332, 38.31023907818019580, 47.04930799450051637 ) ) ;
#6577 = CYLINDRICAL_SURFACE ( 'NONE', #7488, 2.499999999999997335 ) ;
#6578 = CARTESIAN_POINT ( 'NONE',  ( -45.72330504332163059, -5.935454207752205669, 40.04930799450050216 ) ) ;
#6579 = EDGE_LOOP ( 'NONE', ( #10713, #29263, #4150, #31946, #4860 ) ) ;
#6580 = ORIENTED_EDGE ( 'NONE', *, *, #10696, .F. ) ;
#6581 = CARTESIAN_POINT ( 'NONE',  ( 21.09992658989239089, 26.96183152705960495, 47.04930799450051637 ) ) ;
#6582 = DIRECTION ( 'NONE',  ( -0.000000000000000000, -1.000000000000000000, 0.000000000000000000 ) ) ;
#6583 = DIRECTION ( 'NONE',  ( -1.101824276508909887E-16, 1.000000000000000000, -0.000000000000000000 ) ) ;
#6584 = AXIS2_PLACEMENT_3D ( 'NONE', #24732, #19473, #17165 ) ;
#6585 = ORIENTED_EDGE ( 'NONE', *, *, #12778, .T. ) ;
#6586 = CARTESIAN_POINT ( 'NONE',  ( 21.09785597605719332, 34.59164230456639899, 47.04930799450051637 ) ) ;
#6587 = CARTESIAN_POINT ( 'NONE',  ( 79.32175637497277876, -13.74047052604243646, 50.86005336442920566 ) ) ;
#6588 = ORIENTED_EDGE ( 'NONE', *, *, #20291, .T. ) ;
#6589 = DIRECTION ( 'NONE',  ( 0.9612616959383205595, 0.2756373558169932791, -1.660411357259282445E-16 ) ) ;
#6590 = CARTESIAN_POINT ( 'NONE',  ( 47.23302798462060537, 27.18121246473837616, 44.44659793406428605 ) ) ;
#6591 = EDGE_CURVE ( 'NONE', #13209, #8738, #15116, .T. ) ;
#6592 = DIRECTION ( 'NONE',  ( -1.101824276508909887E-16, 1.000000000000000000, -0.000000000000000000 ) ) ;
#6593 = AXIS2_PLACEMENT_3D ( 'NONE', #29090, #24481, #26306 ) ;
#6594 = EDGE_CURVE ( 'NONE', #30310, #22128, #27703, .T. ) ;
#6595 = EDGE_CURVE ( 'NONE', #31343, #29220, #13620, .T. ) ;
#6596 = AXIS2_PLACEMENT_3D ( 'NONE', #15521, #6152, #15850 ) ;
#6597 = ORIENTED_EDGE ( 'NONE', *, *, #13062, .F. ) ;
#6598 = DIRECTION ( 'NONE',  ( 0.000000000000000000, -0.000000000000000000, -1.000000000000000000 ) ) ;
#6599 = DIRECTION ( 'NONE',  ( 0.9612616959383205595, 0.2756373558169931681, -1.660411357259282445E-16 ) ) ;
#6600 = CARTESIAN_POINT ( 'NONE',  ( -42.66751614955960292, 15.14923148629343430, 35.64930799450052490 ) ) ;
#6601 = CARTESIAN_POINT ( 'NONE',  ( 46.00908685603034343, 28.33284706826092503, 44.91496614357594552 ) ) ;
#6602 = ORIENTED_EDGE ( 'NONE', *, *, #25671, .F. ) ;
#6603 = CARTESIAN_POINT ( 'NONE',  ( -40.14354458344919863, 7.767885906595227929, 60.29072935073781991 ) ) ;
#6604 = PLANE ( 'NONE',  #5175 ) ;
#6605 = ADVANCED_FACE ( 'NONE', ( #3925 ), #13546, .T. ) ;
#6606 = AXIS2_PLACEMENT_3D ( 'NONE', #23172, #18078, #1005 ) ;
#6607 = DIRECTION ( 'NONE',  ( -1.101824276508909887E-16, 1.000000000000000000, -0.000000000000000000 ) ) ;
#6608 = CARTESIAN_POINT ( 'NONE',  ( 21.09785597605719332, 13.06454579224779877, 101.3493079945005064 ) ) ;
#6609 = CARTESIAN_POINT ( 'NONE',  ( 21.09785597605719332, -16.63545420775219696, 47.04930799450051637 ) ) ;
#6610 = CARTESIAN_POINT ( 'NONE',  ( -25.19641122222150287, -13.74047052604243646, 11.53332310724657539 ) ) ;
#6611 = DIRECTION ( 'NONE',  ( 0.2756373558169959437, -0.9612616959383197823, 0.000000000000000000 ) ) ;
#6612 = CARTESIAN_POINT ( 'NONE',  ( -40.47970302497625994, 7.463434137431150361, 60.54930799450051637 ) ) ;
#6613 =( NAMED_UNIT ( * ) PLANE_ANGLE_UNIT ( ) SI_UNIT ( $, .RADIAN. ) );
#6614 = ORIENTED_EDGE ( 'NONE', *, *, #7576, .F. ) ;
#6615 = CARTESIAN_POINT ( 'NONE',  ( 45.64903328369346269, 22.95310733321322161, 46.28042130680973543 ) ) ;
#6616 = CARTESIAN_POINT ( 'NONE',  ( 46.99023568444674481, 25.73791119454915588, 49.12151524109405898 ) ) ;
#6617 = DIRECTION ( 'NONE',  ( 0.000000000000000000, 1.000000000000000000, 0.000000000000000000 ) ) ;
#6618 = DIRECTION ( 'NONE',  ( 1.000000000000000000, 0.000000000000000000, 0.000000000000000000 ) ) ;
#6619 = VECTOR ( 'NONE', #14688, 1000.000000000000000 ) ;
#6620 = DIRECTION ( 'NONE',  ( -1.000000000000000000, 0.000000000000000000, 0.000000000000000000 ) ) ;
#6621 = ORIENTED_EDGE ( 'NONE', *, *, #23574, .F. ) ;
#6622 = DIRECTION ( 'NONE',  ( -0.000000000000000000, -1.000000000000000000, 0.000000000000000000 ) ) ;
#6623 = CARTESIAN_POINT ( 'NONE',  ( 46.33059210211230550, 22.93807716476589675, 45.54522087609679204 ) ) ;
#6624 = DIRECTION ( 'NONE',  ( -1.000000000000000000, -1.101824276508909887E-16, 0.000000000000000000 ) ) ;
#6625 = EDGE_CURVE ( 'NONE', #28013, #32254, #1290, .T. ) ;
#6626 = VERTEX_POINT ( 'NONE', #5745 ) ;
#6627 = FACE_OUTER_BOUND ( 'NONE', #28071, .T. ) ;
#6628 = CARTESIAN_POINT ( 'NONE',  ( 33.71785032049135111, 27.21664230456639899, 47.04930799450051637 ) ) ;
#6629 = LINE ( 'NONE', #19082, #19372 ) ;
#6630 = ADVANCED_FACE ( 'NONE', ( #15752 ), #19833, .F. ) ;
#6631 = CARTESIAN_POINT ( 'NONE',  ( 46.47461290750400309, 22.93807716476589675, 45.47175308309371644 ) ) ;
#6632 = ORIENTED_EDGE ( 'NONE', *, *, #10196, .F. ) ;
#6633 = CARTESIAN_POINT ( 'NONE',  ( 8.732853799281738105, 26.96183152705960495, 47.04930799450051637 ) ) ;
#6634 = ORIENTED_EDGE ( 'NONE', *, *, #809, .T. ) ;
#6635 = AXIS2_PLACEMENT_3D ( 'NONE', #6870, #28870, #13937 ) ;
#6636 = EDGE_CURVE ( 'NONE', #24883, #22063, #9895, .T. ) ;
#6637 = EDGE_LOOP ( 'NONE', ( #14247, #23679 ) ) ;
#6638 = ADVANCED_FACE ( 'NONE', ( #19170 ), #9014, .T. ) ;
#6639 = B_SPLINE_CURVE_WITH_KNOTS ( 'NONE', 3,
 ( #25364, #28154, #18127, #22734, #2871, #15665, #5831, #20262, #15836, #25837 ),
 .UNSPECIFIED., .F., .F.,
 ( 4, 2, 2, 2, 4 ),
 ( 0.000000000000000000, 0.0008384749106984347097, 0.001257712366047654233, 0.001467331093722267898, 0.001676949821396881346 ),
 .UNSPECIFIED. ) ;
#6640 = LINE ( 'NONE', #6797, #17899 ) ;
#6641 = B_SPLINE_CURVE_WITH_KNOTS ( 'NONE', 3,
 ( #7702, #18344, #25744, #30676, #27723, #5241, #15250, #8190, #17871, #8036, #8343, #27889, #25260, #467, #18024, #28374 ),
 .UNSPECIFIED., .F., .F.,
 ( 4, 2, 2, 2, 2, 2, 2, 4 ),
 ( 0.000000000000000000, 0.0004663348940371102379, 0.0009326697880742204757, 0.001399004682111330659, 0.001865339576148440951, 0.002798009364222690375, 0.003264344258259825604, 0.003730679152296960399 ),
 .UNSPECIFIED. ) ;
#6642 = CIRCLE ( 'NONE', #869, 12.27641737965282687 ) ;
#6643 = DIRECTION ( 'NONE',  ( -1.000000000000000000, 0.000000000000000000, 0.000000000000000000 ) ) ;
#6644 = DIRECTION ( 'NONE',  ( -1.000000000000000000, 0.000000000000000000, 0.000000000000000000 ) ) ;
#6645 = ORIENTED_EDGE ( 'NONE', *, *, #8890, .F. ) ;
#6646 = CARTESIAN_POINT ( 'NONE',  ( 33.72499318558949710, 30.09143805560860585, 47.04930799450051637 ) ) ;
#6647 = ORIENTED_EDGE ( 'NONE', *, *, #22018, .T. ) ;
#6648 = CARTESIAN_POINT ( 'NONE',  ( 21.09785597605720753, 14.86454579224779948, 47.04930799450052348 ) ) ;
#6649 = CARTESIAN_POINT ( 'NONE',  ( -5.602943079677954685, 9.702389020015065313, 97.51081847724526597 ) ) ;
#6650 = VERTEX_POINT ( 'NONE', #6709 ) ;
#6651 = CARTESIAN_POINT ( 'NONE',  ( -25.59477481493196294, 13.68462854903246573, 47.04930799450052348 ) ) ;
#6652 = CARTESIAN_POINT ( 'NONE',  ( -41.52218637998914375, 11.15499190493234494, 38.19144330556764544 ) ) ;
#6654 = DIRECTION ( 'NONE',  ( 0.4544104193609903586, 0.000000000000000000, 0.8907924397839088737 ) ) ;
#6653 = AXIS2_PLACEMENT_3D ( 'NONE', #27542, #5654, #132 ) ;
#6655 = ORIENTED_EDGE ( 'NONE', *, *, #29004, .T. ) ;
#6656 = DIRECTION ( 'NONE',  ( -1.000000000000000000, 0.000000000000000000, 0.000000000000000000 ) ) ;
#6657 = CARTESIAN_POINT ( 'NONE',  ( -45.72330504332160217, -5.935454207752198563, 54.04930799450053058 ) ) ;
#6658 = LINE ( 'NONE', #1561, #22079 ) ;
#6659 = DIRECTION ( 'NONE',  ( -1.000000000000000000, 0.000000000000000000, 0.000000000000000000 ) ) ;
#6660 = FACE_OUTER_BOUND ( 'NONE', #26848, .T. ) ;
#6661 = VERTEX_POINT ( 'NONE', #96 ) ;
#6662 = DIRECTION ( 'NONE',  ( -1.224646799147353207E-16, 0.000000000000000000, -1.000000000000000000 ) ) ;
#6663 = CYLINDRICAL_SURFACE ( 'NONE', #25894, 0.1000000000000018235 ) ;
#6664 = EDGE_CURVE ( 'NONE', #15469, #30180, #32437, .T. ) ;
#6665 = ORIENTED_EDGE ( 'NONE', *, *, #4667, .T. ) ;
#6666 = FACE_OUTER_BOUND ( 'NONE', #1695, .T. ) ;
#6667 = ADVANCED_FACE ( 'NONE', ( #1620 ), #18257, .F. ) ;
#6668 = DIRECTION ( 'NONE',  ( 8.659560562354932858E-17, -0.7071067811865474617, 0.7071067811865474617 ) ) ;
#6669 = ORIENTED_EDGE ( 'NONE', *, *, #8030, .T. ) ;
#6670 = EDGE_LOOP ( 'NONE', ( #19412, #23972, #29221, #1971 ) ) ;
#6671 = ADVANCED_FACE ( 'NONE', ( #19005 ), #23518, .T. ) ;
#6672 = ORIENTED_EDGE ( 'NONE', *, *, #23092, .T. ) ;
#6673 = ADVANCED_FACE ( 'NONE', ( #15194 ), #31913, .T. ) ;
#6674 = TOROIDAL_SURFACE ( 'NONE', #19235, 1.142135311067127068, 0.1000000000000000056 ) ;
#6675 = AXIS2_PLACEMENT_3D ( 'NONE', #13816, #15618, #18403 ) ;
#6676 = PRODUCT_DEFINITION_SHAPE ( 'NONE', 'NONE',  #32505 ) ;
#6677 = AXIS2_PLACEMENT_3D ( 'NONE', #31573, #15826, #3989 ) ;
#6678 = CARTESIAN_POINT ( 'NONE',  ( -41.91739890389096956, 13.90674392281399818, 54.59993297551692848 ) ) ;
#6679 = VERTEX_POINT ( 'NONE', #10116 ) ;
#6680 = CARTESIAN_POINT ( 'NONE',  ( 45.37383841111020644, 22.88065857334295217, 47.92876263475718446 ) ) ;
#6681 = CARTESIAN_POINT ( 'NONE',  ( 46.21408258523083390, 22.84434098701873239, 49.00610453205841566 ) ) ;
#6682 = DIRECTION ( 'NONE',  ( -0.000000000000000000, -1.000000000000000000, 0.000000000000000000 ) ) ;
#6683 = CARTESIAN_POINT ( 'NONE',  ( 21.09992658989239089, 30.46183152705961561, 47.04930799450051637 ) ) ;
#6684 = CARTESIAN_POINT ( 'NONE',  ( 44.74832014356462651, 27.72786309983298025, 46.92728461490987257 ) ) ;
#6685 = EDGE_LOOP ( 'NONE', ( #13660, #11027, #1657, #16407 ) ) ;
#6686 = DIRECTION ( 'NONE',  ( -1.101824276508909887E-16, 1.000000000000000000, -0.000000000000000000 ) ) ;
#6687 = ORIENTED_EDGE ( 'NONE', *, *, #22373, .T. ) ;
#6688 = DIRECTION ( 'NONE',  ( -0.000000000000000000, 1.000000000000000000, -0.000000000000000000 ) ) ;
#6689 = EDGE_LOOP ( 'NONE', ( #18251, #8301, #10419, #5218 ) ) ;
#6690 = FACE_OUTER_BOUND ( 'NONE', #27098, .T. ) ;
#6691 = CARTESIAN_POINT ( 'NONE',  ( 8.698509210239526723, 26.09164230456639899, 47.04930799450051637 ) ) ;
#6692 = DIRECTION ( 'NONE',  ( 0.000000000000000000, 0.000000000000000000, 1.000000000000000000 ) ) ;
#6693 = DIRECTION ( 'NONE',  ( 0.000000000000000000, 1.000000000000000000, 0.000000000000000000 ) ) ;
#6694 = CARTESIAN_POINT ( 'NONE',  ( 49.28428300279882990, 26.94787913140504543, 48.46772541801551171 ) ) ;
#6695 = CARTESIAN_POINT ( 'NONE',  ( 46.33206787849857022, 22.99884124225578574, 48.22973596570440691 ) ) ;
#6696 = LINE ( 'NONE', #24580, #32159 ) ;
#6697 = EDGE_LOOP ( 'NONE', ( #25460, #21704, #6347, #20153 ) ) ;
#6698 = DIRECTION ( 'NONE',  ( 0.000000000000000000, 0.000000000000000000, -1.000000000000000000 ) ) ;
#6699 = DIRECTION ( 'NONE',  ( 0.000000000000000000, -0.000000000000000000, -1.000000000000000000 ) ) ;
#6700 = VECTOR ( 'NONE', #25858, 1000.000000000000000 ) ;
#6701 = FACE_OUTER_BOUND ( 'NONE', #4938, .T. ) ;
#6702 = AXIS2_PLACEMENT_3D ( 'NONE', #30306, #7328, #9954 ) ;
#6703 = FACE_OUTER_BOUND ( 'NONE', #13449, .T. ) ;
#6704 = EDGE_LOOP ( 'NONE', ( #15581, #10, #9805, #21447 ) ) ;
#6705 = DIRECTION ( 'NONE',  ( 0.8746197071393925215, -0.4848096202463429982, -8.676864087101708112E-18 ) ) ;
#6706 = AXIS2_PLACEMENT_3D ( 'NONE', #10992, #2671, #19893 ) ;
#6707 = EDGE_LOOP ( 'NONE', ( #11496, #24901, #19577, #19952 ) ) ;
#6708 = CARTESIAN_POINT ( 'NONE',  ( -42.32583647289407480, 13.67174551105522617, 54.57447098782054695 ) ) ;
#6709 = CARTESIAN_POINT ( 'NONE',  ( 21.09785597605719332, -16.63545420775219696, -25.16074251183828636 ) ) ;
#6710 = EDGE_CURVE ( 'NONE', #25964, #25453, #10441, .T. ) ;
#6711 = AXIS2_PLACEMENT_3D ( 'NONE', #26336, #25699, #23236 ) ;
#6712 = VERTEX_POINT ( 'NONE', #21467 ) ;
#6713 = EDGE_CURVE ( 'NONE', #27697, #19462, #11475, .T. ) ;
#6714 = ADVANCED_FACE ( 'NONE', ( #11645 ), #21638, .T. ) ;
#6715 = VERTEX_POINT ( 'NONE', #16548 ) ;
#6716 = CARTESIAN_POINT ( 'NONE',  ( 47.23884743062419744, 22.86454579224779948, 45.05393496349946503 ) ) ;
#6717 = AXIS2_PLACEMENT_3D ( 'NONE', #6436, #18416, #26295 ) ;
#6718 = DIRECTION ( 'NONE',  ( -0.1949050434465251780, 0.6797146636928671493, -0.7071067811865481278 ) ) ;
#6719 = CARTESIAN_POINT ( 'NONE',  ( 46.59785597605721108, -5.098646251524523443, 47.04930799450052348 ) ) ;
#6720 = ORIENTED_EDGE ( 'NONE', *, *, #25059, .T. ) ;
#6721 = AXIS2_PLACEMENT_3D ( 'NONE', #32380, #29755, #22192 ) ;
#6722 = CARTESIAN_POINT ( 'NONE',  ( 46.04302072787191946, 22.93328494799376571, 45.69307819878901000 ) ) ;
#6723 = CIRCLE ( 'NONE', #25083, 0.1250000000000001110 ) ;
#6724 = DIRECTION ( 'NONE',  ( -1.188208965918165239E-16, -1.880121038077813132E-16, -1.000000000000000000 ) ) ;
#6725 = CARTESIAN_POINT ( 'NONE',  ( 79.37786958444415575, -5.721341737285090545, 15.14745076809877133 ) ) ;
#6726 = ORIENTED_EDGE ( 'NONE', *, *, #32113, .F. ) ;
#6727 = DIRECTION ( 'NONE',  ( 0.000000000000000000, -0.2964022880492104273, 0.9550631830613055540 ) ) ;
#6728 = ORIENTED_EDGE ( 'NONE', *, *, #521, .T. ) ;
#6729 = AXIS2_PLACEMENT_3D ( 'NONE', #21851, #6924, #26784 ) ;
#6730 = DIRECTION ( 'NONE',  ( -1.000000000000000000, 0.000000000000000000, 0.000000000000000000 ) ) ;
#6731 = CARTESIAN_POINT ( 'NONE',  ( 8.698509210239521394, 25.59164230456639899, 47.04930799450051637 ) ) ;
#6732 = CARTESIAN_POINT ( 'NONE',  ( 21.09785597605719332, 30.56454579224779522, 15.54930799450051460 ) ) ;
#6733 = FILL_AREA_STYLE_COLOUR ( '', #9232 ) ;
#6734 = ORIENTED_EDGE ( 'NONE', *, *, #8851, .F. ) ;
#6735 = ORIENTED_EDGE ( 'NONE', *, *, #5152, .F. ) ;
#6736 = ADVANCED_FACE ( 'NONE', ( #7491 ), #30347, .T. ) ;
#6737 = CARTESIAN_POINT ( 'NONE',  ( 21.09785597605720753, -5.098646251524523443, 47.04930799450052348 ) ) ;
#6738 = FACE_OUTER_BOUND ( 'NONE', #28916, .T. ) ;
#6739 = CARTESIAN_POINT ( 'NONE',  ( 21.09992658989238734, 38.56284415653841791, 47.04930799450051637 ) ) ;
#6740 = VERTEX_POINT ( 'NONE', #4080 ) ;
#6741 = DIRECTION ( 'NONE',  ( -1.000000000000000000, -1.101824276508909764E-16, 0.000000000000000000 ) ) ;
#6742 = CARTESIAN_POINT ( 'NONE',  ( 78.94643999631823306, -13.74047052604243646, 54.67070450616910904 ) ) ;
#6743 = ORIENTED_EDGE ( 'NONE', *, *, #5577, .T. ) ;
#6744 = DIRECTION ( 'NONE',  ( -1.000000000000000000, -1.101824276508909887E-16, 0.000000000000000000 ) ) ;
#6745 = CARTESIAN_POINT ( 'NONE',  ( 45.46000861347822308, 26.07287913140504543, 49.57397645940629616 ) ) ;
#6746 = CIRCLE ( 'NONE', #22452, 0.1250000000000001110 ) ;
#6747 = AXIS2_PLACEMENT_3D ( 'NONE', #20190, #20514, #30542 ) ;
#6748 = LINE ( 'NONE', #9378, #14878 ) ;
#6749 = EDGE_CURVE ( 'NONE', #12175, #9356, #27718, .T. ) ;
#6750 = ADVANCED_FACE ( 'NONE', ( #21801 ), #14273, .T. ) ;
#6751 = ADVANCED_FACE ( 'NONE', ( #24267 ), #9334, .T. ) ;
#6752 = EDGE_CURVE ( 'NONE', #19450, #24287, #27509, .T. ) ;
#6753 = AXIS2_PLACEMENT_3D ( 'NONE', #7234, #32348, #19858 ) ;
#6754 = VERTEX_POINT ( 'NONE', #15037 ) ;
#6755 = CARTESIAN_POINT ( 'NONE',  ( 21.09992658989238734, 38.56284415653841791, 47.04930799450051637 ) ) ;
#6756 = CARTESIAN_POINT ( 'NONE',  ( -42.38687957179149635, 4.148162238787999279, 37.04930799450052348 ) ) ;
#6757 = CARTESIAN_POINT ( 'NONE',  ( 47.22751897799751220, 28.64253733014355774, 44.55267275764142454 ) ) ;
#6758 = CARTESIAN_POINT ( 'NONE',  ( 45.35708200440645044, 27.69118040159425931, 45.92000246470679770 ) ) ;
#6759 = EDGE_LOOP ( 'NONE', ( #623, #22827, #20146, #28642 ) ) ;
#6760 = DIRECTION ( 'NONE',  ( -1.000000000000000000, -1.101824276508909887E-16, 0.000000000000000000 ) ) ;
#6761 = CARTESIAN_POINT ( 'NONE',  ( 21.09785597605720753, -13.88867167006704939, -11.65212399594570769 ) ) ;
#6762 = CARTESIAN_POINT ( 'NONE',  ( -40.13606231985500017, 7.635531802539801127, 53.80788663826320573 ) ) ;
#6763 = AXIS2_PLACEMENT_3D ( 'NONE', #5402, #22942, #466 ) ;
#6764 = CIRCLE ( 'NONE', #13577, 1.499999999999994449 ) ;
#6765 = DIRECTION ( 'NONE',  ( -0.000000000000000000, -1.000000000000000000, 0.000000000000000000 ) ) ;
#6766 = FACE_OUTER_BOUND ( 'NONE', #21262, .T. ) ;
#6767 = CARTESIAN_POINT ( 'NONE',  ( -35.26384896152210757, -13.74047052604243646, 62.14575043855078462 ) ) ;
#6768 = DIRECTION ( 'NONE',  ( -0.000000000000000000, -1.000000000000000000, -0.000000000000000000 ) ) ;
#6769 =( BOUNDED_CURVE ( )  B_SPLINE_CURVE ( 2, ( #7430, #12518, #34, #7587, #17585, #27601, #5604, #25941, #20855 ),
 .UNSPECIFIED., .F., .F. ) 
 B_SPLINE_CURVE_WITH_KNOTS ( ( 3, 2, 2, 2, 3 ),
 ( 0.3928571440184155938, 0.4047619047619047672, 0.4285714285714285476, 0.4523809523809523836, 0.4642857154469869352 ),
 .UNSPECIFIED. ) 
 CURVE ( )  GEOMETRIC_REPRESENTATION_ITEM ( )  RATIONAL_B_SPLINE_CURVE ( ( 0.9330127018922200755, 0.9330127084266233162, 1.000000000000000000, 0.8660254037844388186, 1.000000000000000000, 0.8660254037844388186, 1.000000000000000000, 0.9330126953578159466, 0.9330127018922200755 ) ) 
 REPRESENTATION_ITEM ( '' )  );
#6770 = DIRECTION ( 'NONE',  ( -1.101824276508909887E-16, 1.000000000000000000, -0.000000000000000000 ) ) ;
#6771 = ORIENTED_EDGE ( 'NONE', *, *, #17859, .F. ) ;
#6772 = EDGE_CURVE ( 'NONE', #30637, #6106, #25041, .T. ) ;
#6773 = FACE_OUTER_BOUND ( 'NONE', #13650, .T. ) ;
#6774 = EDGE_CURVE ( 'NONE', #27708, #27524, #24057, .T. ) ;
#6775 = CARTESIAN_POINT ( 'NONE',  ( -40.41141501439636841, 8.548644083377668679, 34.56232498761289662 ) ) ;
#6776 = CARTESIAN_POINT ( 'NONE',  ( -40.61178118339597631, 9.038025460530262123, 57.04930799450051637 ) ) ;
#6777 = CIRCLE ( 'NONE', #25129, 85.00000000000001421 ) ;
#6778 = CARTESIAN_POINT ( 'NONE',  ( 33.72499318558949710, 26.84143805560860940, 47.04930799450051637 ) ) ;
#6779 = ORIENTED_EDGE ( 'NONE', *, *, #1550, .T. ) ;
#6780 = CARTESIAN_POINT ( 'NONE',  ( -39.56822316924148453, -5.935876471981492486, 77.89643810228372445 ) ) ;
#6781 = AXIS2_PLACEMENT_3D ( 'NONE', #20189, #7727, #17723 ) ;
#6782 = DIRECTION ( 'NONE',  ( -0.8746197071393895239, 0.4848096202463481053, 0.000000000000000000 ) ) ;
#6783 = CARTESIAN_POINT ( 'NONE',  ( 33.72499318558949710, 26.34184655352419213, 47.04930799450051637 ) ) ;
#6784 = ORIENTED_EDGE ( 'NONE', *, *, #1891, .F. ) ;
#6785 = ORIENTED_EDGE ( 'NONE', *, *, #6390, .T. ) ;
#6786 = CARTESIAN_POINT ( 'NONE',  ( -40.14234630318158281, 6.912323292265333485, 39.54347762122440457 ) ) ;
#6787 = FACE_OUTER_BOUND ( 'NONE', #10979, .T. ) ;
#6788 = CARTESIAN_POINT ( 'NONE',  ( 8.698509210239574685, 31.09164230456639544, 47.04930799450051637 ) ) ;
#6789 = CARTESIAN_POINT ( 'NONE',  ( 53.16169625780806740, -5.983766253076982622, 97.45038561958638468 ) ) ;
#6790 = ORIENTED_EDGE ( 'NONE', *, *, #7723, .F. ) ;
#6791 = CARTESIAN_POINT ( 'NONE',  ( -40.51045226066063520, 7.589116544599138869, 60.22001867261916885 ) ) ;
#6792 = ORIENTED_EDGE ( 'NONE', *, *, #24153, .F. ) ;
#6793 = EDGE_CURVE ( 'NONE', #30739, #17357, #6233, .T. ) ;
#6794 = VECTOR ( 'NONE', #22584, 1000.000000000000000 ) ;
#6795 = AXIS2_PLACEMENT_3D ( 'NONE', #15512, #30775, #887 ) ;
#6796 = ORIENTED_EDGE ( 'NONE', *, *, #18887, .T. ) ;
#6797 = CARTESIAN_POINT ( 'NONE',  ( 21.09785597605720753, -13.68834655544033652, 102.7436001025633772 ) ) ;
#6798 = VECTOR ( 'NONE', #12374, 1000.000000000000114 ) ;
#6799 = AXIS2_PLACEMENT_3D ( 'NONE', #7115, #17113, #27134 ) ;
#6800 = AXIS2_PLACEMENT_3D ( 'NONE', #2440, #25086, #3069 ) ;
#6801 = EDGE_CURVE ( 'NONE', #4992, #24759, #19313, .T. ) ;
#6802 = DIRECTION ( 'NONE',  ( 0.2756373558169946114, -0.9612616959383201154, 3.004509245426093872E-15 ) ) ;
#6803 = DIRECTION ( 'NONE',  ( -0.4544104659272507063, 0.000000000000000000, -0.8907924160295589422 ) ) ;
#6804 = DIRECTION ( 'NONE',  ( -0.8746197071393926326, 0.4848096202463430537, 8.676864087101709653E-18 ) ) ;
#6805 = AXIS2_PLACEMENT_3D ( 'NONE', #14582, #1445, #24584 ) ;
#6806 = EDGE_CURVE ( 'NONE', #1229, #8522, #15994, .T. ) ;
#6807 = VERTEX_POINT ( 'NONE', #576 ) ;
#6808 = DIRECTION ( 'NONE',  ( 0.000000000000000000, 0.000000000000000000, -1.000000000000000000 ) ) ;
#6809 = ORIENTED_EDGE ( 'NONE', *, *, #5673, .T. ) ;
#6810 = CARTESIAN_POINT ( 'NONE',  ( 33.50134396954526750, 24.59164230456639544, 47.04930799450051637 ) ) ;
#6811 = DIRECTION ( 'NONE',  ( -0.000000000000000000, -1.000000000000000000, -0.000000000000000000 ) ) ;
#6812 = DIRECTION ( 'NONE',  ( 1.000000000000000000, 0.000000000000000000, 2.775557561562892534E-15 ) ) ;
#6813 = ORIENTED_EDGE ( 'NONE', *, *, #16112, .T. ) ;
#6814 = EDGE_CURVE ( 'NONE', #14753, #7068, #13389, .T. ) ;
#6815 = DIRECTION ( 'NONE',  ( 0.000000000000000000, -1.000000000000000000, 0.000000000000000000 ) ) ;
#6816 = DIRECTION ( 'NONE',  ( -1.000000000000000000, -1.101824276508909887E-16, 0.000000000000000000 ) ) ;
#6817 = CIRCLE ( 'NONE', #29360, 0.1250000000000001110 ) ;
#6818 = EDGE_CURVE ( 'NONE', #7331, #25938, #463, .T. ) ;
#6819 = CARTESIAN_POINT ( 'NONE',  ( -43.64073206722599707, 1.267352857069779848, 39.44930799450052916 ) ) ;
#6820 = CYLINDRICAL_SURFACE ( 'NONE', #28346, 0.1000000000000018235 ) ;
#6821 = CARTESIAN_POINT ( 'NONE',  ( -40.65235181538429288, 9.419364959807719373, 39.50704302141948432 ) ) ;
#6822 = ADVANCED_FACE ( 'NONE', ( #27997 ), #5355, .T. ) ;
#6823 = CARTESIAN_POINT ( 'NONE',  ( -42.36153388572594025, 13.68895619636815475, 54.63750615257477961 ) ) ;
#6824 = ORIENTED_EDGE ( 'NONE', *, *, #13469, .F. ) ;
#6825 = CARTESIAN_POINT ( 'NONE',  ( -40.02353495282660845, 6.996741953892291477, 34.61178260766359926 ) ) ;
#6826 = DIRECTION ( 'NONE',  ( -1.000000000000000000, -1.101824276508909887E-16, 0.000000000000000000 ) ) ;
#6827 = ORIENTED_EDGE ( 'NONE', *, *, #30719, .T. ) ;
#6828 = CARTESIAN_POINT ( 'NONE',  ( -45.38823791396688989, -5.820268484099551998, 53.36341473305946437 ) ) ;
#6829 = CIRCLE ( 'NONE', #12607, 27.99999999999999645 ) ;
#6830 = AXIS2_PLACEMENT_3D ( 'NONE', #18691, #9186, #16714 ) ;
#6831 = CARTESIAN_POINT ( 'NONE',  ( 33.37634396954525329, 26.09164230456639899, 47.04930799450051637 ) ) ;
#6832 = ORIENTED_EDGE ( 'NONE', *, *, #29808, .T. ) ;
#6833 = AXIS2_PLACEMENT_3D ( 'NONE', #25311, #17917, #352 ) ;
#6834 = ORIENTED_EDGE ( 'NONE', *, *, #18561, .T. ) ;
#6835 = CIRCLE ( 'NONE', #23602, 0.1000000000000014905 ) ;
#6836 = EDGE_CURVE ( 'NONE', #30572, #8513, #22740, .T. ) ;
#6837 = AXIS2_PLACEMENT_3D ( 'NONE', #4816, #32066, #14837 ) ;
#6838 = CONICAL_SURFACE ( 'NONE', #17322, 84.50502525316943547, 0.7853981633974621568 ) ;
#6839 = EDGE_LOOP ( 'NONE', ( #27466, #20610, #8824, #22255 ) ) ;
#6840 = CIRCLE ( 'NONE', #2650, 55.85791022362053582 ) ;
#6841 = ADVANCED_FACE ( 'NONE', ( #22899 ), #7292, .T. ) ;
#6842 = PLANE ( 'NONE',  #26632 ) ;
#6843 = VECTOR ( 'NONE', #32265, 1000.000000000000000 ) ;
#6844 = EDGE_CURVE ( 'NONE', #8185, #11676, #2579, .T. ) ;
#6845 = ORIENTED_EDGE ( 'NONE', *, *, #8974, .T. ) ;
#6846 = ORIENTED_EDGE ( 'NONE', *, *, #12619, .F. ) ;
#6847 = DIRECTION ( 'NONE',  ( -1.234978253042719660E-16, 1.000000000000000000, 1.109335647967047851E-31 ) ) ;
#6848 = CARTESIAN_POINT ( 'NONE',  ( 64.59785597605720397, 14.86454579224779948, 47.04930799450051637 ) ) ;
#6849 = VECTOR ( 'NONE', #25590, 1000.000000000000114 ) ;
#6850 = FACE_BOUND ( 'NONE', #14123, .T. ) ;
#6851 = CARTESIAN_POINT ( 'NONE',  ( 8.474859994195286461, 24.34143805560860940, 47.04930799450051637 ) ) ;
#6852 = CARTESIAN_POINT ( 'NONE',  ( 44.74832014356462651, 26.32786309983298878, 46.92728461490987257 ) ) ;
#6853 = AXIS2_PLACEMENT_3D ( 'NONE', #17991, #12923, #22912 ) ;
#6854 = EDGE_LOOP ( 'NONE', ( #29889, #8246, #1811, #11190 ) ) ;
#6855 = DIRECTION ( 'NONE',  ( -0.9612616959383200044, -0.2756373558169954996, 1.660411357259285896E-16 ) ) ;
#6856 = EDGE_LOOP ( 'NONE', ( #853, #23700, #1647, #17755 ) ) ;
#6857 = LINE ( 'NONE', #14248, #31593 ) ;
#6858 =( GEOMETRIC_REPRESENTATION_CONTEXT ( 3 ) GLOBAL_UNCERTAINTY_ASSIGNED_CONTEXT ( ( #19289 ) ) GLOBAL_UNIT_ASSIGNED_CONTEXT ( ( #28350, #15874, #19449 ) ) REPRESENTATION_CONTEXT ( 'NONE', 'WORKASPACE' ) );
#6859 = EDGE_CURVE ( 'NONE', #26186, #23946, #6764, .T. ) ;
#6860 = ORIENTED_EDGE ( 'NONE', *, *, #10274, .T. ) ;
#6861 = CARTESIAN_POINT ( 'NONE',  ( 21.09785597605720753, 14.86454579224779948, 47.04930799450052348 ) ) ;
#6862 = FACE_OUTER_BOUND ( 'NONE', #3256, .T. ) ;
#6863 = CYLINDRICAL_SURFACE ( 'NONE', #14683, 12.36707279061065101 ) ;
#6864 = DIRECTION ( 'NONE',  ( 0.1949050434465276760, -0.6797146636928699248, -0.7071067811865447972 ) ) ;
#6865 = DIRECTION ( 'NONE',  ( -1.224646799147353207E-16, -1.349345573449484691E-32, 1.000000000000000000 ) ) ;
#6866 = CARTESIAN_POINT ( 'NONE',  ( 46.96268396749378127, 24.73121246473838042, 49.65201805493727960 ) ) ;
#6867 = CARTESIAN_POINT ( 'NONE',  ( 46.45074414369405957, 22.93328494799376571, 48.64093701409239401 ) ) ;
#6868 = PLANE ( 'NONE',  #26366 ) ;
#6869 = ORIENTED_EDGE ( 'NONE', *, *, #3822, .T. ) ;
#6870 = CARTESIAN_POINT ( 'NONE',  ( 21.09992658989238734, 38.56284415653841791, 47.04930799450051637 ) ) ;
#6871 = DIRECTION ( 'NONE',  ( -1.000000000000000000, 0.000000000000000000, 0.000000000000000000 ) ) ;
#6872 = CIRCLE ( 'NONE', #28365, 12.62506659569710266 ) ;
#6873 = DIRECTION ( 'NONE',  ( -1.000000000000000000, 0.000000000000000000, 0.000000000000000000 ) ) ;
#6874 = DIRECTION ( 'NONE',  ( 0.9986540920324801229, 1.233316085972235327E-16, 0.05186525298099653458 ) ) ;
#6875 = CARTESIAN_POINT ( 'NONE',  ( -29.27337757263006424, 11.92829594627139933, 24.97746215641624090 ) ) ;
#6876 = ORIENTED_EDGE ( 'NONE', *, *, #10546, .F. ) ;
#6877 = CARTESIAN_POINT ( 'NONE',  ( 21.09785597605719332, 25.56454579224779167, 47.04930799450051637 ) ) ;
#6878 = ORIENTED_EDGE ( 'NONE', *, *, #186, .T. ) ;
#6879 = DIRECTION ( 'NONE',  ( -1.000000000000000000, -1.101824276508909887E-16, 0.000000000000000000 ) ) ;
#6880 = CARTESIAN_POINT ( 'NONE',  ( -42.38687957179149635, 4.148162238787999279, 37.04930799450052348 ) ) ;
#6881 = ORIENTED_EDGE ( 'NONE', *, *, #23468, .F. ) ;
#6882 = AXIS2_PLACEMENT_3D ( 'NONE', #17019, #9492, #16864 ) ;
#6883 = AXIS2_PLACEMENT_3D ( 'NONE', #6612, #8591, #9237 ) ;
#6884 = VECTOR ( 'NONE', #12243, 1000.000000000000000 ) ;
#6885 = ORIENTED_EDGE ( 'NONE', *, *, #31431, .T. ) ;
#6886 = DIRECTION ( 'NONE',  ( -0.9612616959383213366, -0.2756373558169906701, 9.294164490659098336E-15 ) ) ;
#6887 = DIRECTION ( 'NONE',  ( 0.1949050434465267045, -0.6797146636928664831, -0.7071067811865482389 ) ) ;
#6888 = CARTESIAN_POINT ( 'NONE',  ( 21.09785597605720753, 14.86454579224779948, 47.04930799450052348 ) ) ;
#6889 = AXIS2_PLACEMENT_3D ( 'NONE', #6961, #27312, #2368 ) ;
#6890 = EDGE_LOOP ( 'NONE', ( #453, #30917 ) ) ;
#6891 = DIRECTION ( 'NONE',  ( -0.5442436726714893203, -6.721291001053903893E-17, 0.8389271868029124501 ) ) ;
#6892 = DIRECTION ( 'NONE',  ( 0.000000000000000000, 0.000000000000000000, 1.000000000000000000 ) ) ;
#6893 = LINE ( 'NONE', #16894, #26332 ) ;
#6894 = ORIENTED_EDGE ( 'NONE', *, *, #24233, .T. ) ;
#6895 = ORIENTED_EDGE ( 'NONE', *, *, #25491, .F. ) ;
#6896 = EDGE_CURVE ( 'NONE', #7848, #154, #9377, .T. ) ;
#6897 = ORIENTED_EDGE ( 'NONE', *, *, #7458, .T. ) ;
#6898 = CIRCLE ( 'NONE', #14778, 39.49999999999999289 ) ;
#6899 = DIRECTION ( 'NONE',  ( -0.000000000000000000, -1.000000000000000000, -0.000000000000000000 ) ) ;
#6900 = DIRECTION ( 'NONE',  ( -1.000000000000000000, 0.000000000000000000, 0.000000000000000000 ) ) ;
#6901 = EDGE_CURVE ( 'NONE', #12307, #5411, #15740, .T. ) ;
#6902 = CARTESIAN_POINT ( 'NONE',  ( 21.09785597605719332, 30.56454579224779522, 64.04930799450050927 ) ) ;
#6903 = SURFACE_STYLE_FILL_AREA ( #29384 ) ;
#6904 = ORIENTED_EDGE ( 'NONE', *, *, #18446, .T. ) ;
#6905 = ORIENTED_EDGE ( 'NONE', *, *, #3104, .F. ) ;
#6906 = DIRECTION ( 'NONE',  ( -1.000000000000000000, 0.000000000000000000, 0.000000000000000000 ) ) ;
#6907 = LINE ( 'NONE', #32014, #30865 ) ;
#6908 = VERTEX_POINT ( 'NONE', #18452 ) ;
#6909 = DIRECTION ( 'NONE',  ( -0.000000000000000000, 1.000000000000000000, 0.000000000000000000 ) ) ;
#6910 = VERTEX_POINT ( 'NONE', #5992 ) ;
#6911 = DIRECTION ( 'NONE',  ( -1.000000000000000000, 0.000000000000000000, 0.000000000000000000 ) ) ;
#6912 = CARTESIAN_POINT ( 'NONE',  ( -58.11219453028166981, -15.93545420775219945, 44.54930799450023216 ) ) ;
#6913 = AXIS2_PLACEMENT_3D ( 'NONE', #29836, #12605, #29512 ) ;
#6914 = CYLINDRICAL_SURFACE ( 'NONE', #15919, 12.36707279061065101 ) ;
#6915 = ORIENTED_EDGE ( 'NONE', *, *, #5124, .T. ) ;
#6916 = AXIS2_PLACEMENT_3D ( 'NONE', #3343, #30449, #31088 ) ;
#6917 = B_SPLINE_CURVE_WITH_KNOTS ( 'NONE', 3,
 ( #14369, #24366, #1883, #21896, #2216, #22062, #26998, #4511, #27153, #15499, #7961, #17793, #10101, #15651, #20094, #30123, #10264, #557, #13214 ),
 .UNSPECIFIED., .F., .F.,
 ( 4, 3, 3, 3, 3, 3, 4 ),
 ( 5.204170427930421283E-17, 4.880491127589490851E-05, 6.736105324526939382E-05, 7.908518729062757934E-05, 8.835348272573385604E-05, 9.246404311662424498E-05, 9.397889733287322230E-05 ),
 .UNSPECIFIED. ) ;
#6918 = AXIS2_PLACEMENT_3D ( 'NONE', #883, #23534, #16137 ) ;
#6919 = FACE_OUTER_BOUND ( 'NONE', #15988, .T. ) ;
#6920 = DIRECTION ( 'NONE',  ( -0.2756373558169947779, 0.9612616959383200044, 0.000000000000000000 ) ) ;
#6921 = DIRECTION ( 'NONE',  ( -1.000000000000000000, -1.101824276508909887E-16, 0.000000000000000000 ) ) ;
#6922 = CARTESIAN_POINT ( 'NONE',  ( 48.94625023931840246, 28.85784706826092716, 46.10640627770150246 ) ) ;
#6923 = VERTEX_POINT ( 'NONE', #3029 ) ;
#6924 = DIRECTION ( 'NONE',  ( 0.1949050434465265935, -0.6797146636928685925, -0.7071067811865462405 ) ) ;
#6925 = CIRCLE ( 'NONE', #25290, 12.62506659569710266 ) ;
#6926 = CARTESIAN_POINT ( 'NONE',  ( 54.07257848512811194, -4.853532562205614020, -9.150780730119983275 ) ) ;
#6927 = DIRECTION ( 'NONE',  ( -1.101824276508909887E-16, 1.000000000000000000, -0.000000000000000000 ) ) ;
#6928 = DIRECTION ( 'NONE',  ( -1.000000000000000000, -1.101824276508909887E-16, 0.000000000000000000 ) ) ;
#6929 = FACE_OUTER_BOUND ( 'NONE', #816, .T. ) ;
#6930 = EDGE_CURVE ( 'NONE', #2726, #8315, #10608, .T. ) ;
#6931 = CARTESIAN_POINT ( 'NONE',  ( -22.76726271559793702, -13.74047052604243646, 85.52521890125204607 ) ) ;
#6933 = EDGE_CURVE ( 'NONE', #22591, #29694, #30625, .T. ) ;
#6932 = CARTESIAN_POINT ( 'NONE',  ( 21.09785597605719332, 11.92558985988973497, 47.04930799450051637 ) ) ;
#6934 = CIRCLE ( 'NONE', #25291, 0.1250000000000001110 ) ;
#6935 = B_SPLINE_SURFACE_WITH_KNOTS ( 'NONE', 3, 3, ( 
 ( #14094, #1606, #22111, #21624, #6695, #1930 ),
 ( #27043, #24415, #4557, #24089, #21455, #19490 ),
 ( #14576, #29344, #1440, #26883, #4064, #6867 ),
 ( #29518, #11947, #1772, #31656, #32143, #29183 ),
 ( #29678, #7184, #26719, #14257, #4396, #7023 ),
 ( #16693, #17181, #4240, #24253, #31972, #24579 ) ),
 .UNSPECIFIED., .F., .F., .F.,
 ( 4, 2, 4 ),
 ( 4, 2, 4 ),
 ( 0.000000000000000000, 0.5000000000000000000, 1.000000000000000000 ),
 ( 0.000000000000000000, 0.5000000000000000000, 1.000000000000000000 ),
 .UNSPECIFIED. ) ;
#6936 = ADVANCED_FACE ( 'NONE', ( #18284 ), #14926, .T. ) ;
#6937 = EDGE_CURVE ( 'NONE', #14823, #15416, #17760, .T. ) ;
#6938 = EDGE_LOOP ( 'NONE', ( #15090, #9621, #31171, #9096 ) ) ;
#6939 = CARTESIAN_POINT ( 'NONE',  ( 45.86034435575247414, 22.98765316579147111, 46.24648758314307173 ) ) ;
#6940 = CARTESIAN_POINT ( 'NONE',  ( 44.41710432008958520, 25.31454579807170191, 48.41681133995267317 ) ) ;
#6941 = VECTOR ( 'NONE', #5896, 1000.000000000000341 ) ;
#6942 = CARTESIAN_POINT ( 'NONE',  ( 21.09785597605719332, 13.06454579224779877, 102.0493079945005093 ) ) ;
#6943 = CARTESIAN_POINT ( 'NONE',  ( 54.32959031772210068, -4.491775094913927013, 102.8641432012177148 ) ) ;
#6944 = ORIENTED_EDGE ( 'NONE', *, *, #28841, .T. ) ;
#6945 = AXIS2_PLACEMENT_3D ( 'NONE', #2828, #23935, #31499 ) ;
#6946 = CARTESIAN_POINT ( 'NONE',  ( -39.57252254196389885, -5.936104880602451672, 77.91875142326841797 ) ) ;
#6947 = LINE ( 'NONE', #8753, #12716 ) ;
#6948 = FACE_OUTER_BOUND ( 'NONE', #32005, .T. ) ;
#6949 = ORIENTED_EDGE ( 'NONE', *, *, #24383, .T. ) ;
#6950 = EDGE_LOOP ( 'NONE', ( #22748, #22333, #11949, #11853 ) ) ;
#6951 = CARTESIAN_POINT ( 'NONE',  ( -40.65093765668705572, 9.567768634527945792, 35.64930799450052490 ) ) ;
#6952 = CARTESIAN_POINT ( 'NONE',  ( 45.24946171279598417, 29.20784706826092503, 47.99220971130007030 ) ) ;
#6953 = CARTESIAN_POINT ( 'NONE',  ( -42.60588768478345401, 14.57151196022700290, 38.19144330556764544 ) ) ;
#6954 = CARTESIAN_POINT ( 'NONE',  ( 49.52052953415556402, 8.310461108307681144, 106.7232700815558957 ) ) ;
#6955 = ORIENTED_EDGE ( 'NONE', *, *, #28426, .T. ) ;
#6956 = CARTESIAN_POINT ( 'NONE',  ( 71.55936645880203173, 9.702389020015065313, 20.34850893876554423 ) ) ;
#6957 = EDGE_LOOP ( 'NONE', ( #27657, #22779, #12673, #6944 ) ) ;
#6958 = ORIENTED_EDGE ( 'NONE', *, *, #25491, .T. ) ;
#6959 = AXIS2_PLACEMENT_3D ( 'NONE', #29181, #6865, #19155 ) ;
#6960 = AXIS2_PLACEMENT_3D ( 'NONE', #23157, #16244, #14119 ) ;
#6961 = CARTESIAN_POINT ( 'NONE',  ( -41.24971778908466291, 11.62557032131817181, 57.04930799450051637 ) ) ;
#6962 = EDGE_CURVE ( 'NONE', #24589, #4920, #4868, .T. ) ;
#6963 = ORIENTED_EDGE ( 'NONE', *, *, #15397, .F. ) ;
#6964 = VECTOR ( 'NONE', #14710, 1000.000000000000114 ) ;
#6965 =( BOUNDED_SURFACE ( )  B_SPLINE_SURFACE ( 3, 2, ( 
 ( #17424, #12520, #22994 ),
 ( #25143, #20213, #2969 ),
 ( #7261, #27603, #10541 ),
 ( #22835, #30236, #10372 ) ),
 .UNSPECIFIED., .F., .F., .F. ) 
 B_SPLINE_SURFACE_WITH_KNOTS ( ( 4, 4 ),
 ( 3, 3 ),
 ( 0.0002011154675331821196, 0.0003574932873931827796 ),
 ( 0.000000000000000000, 1.000000000000000000 ),
 .UNSPECIFIED. ) 
 GEOMETRIC_REPRESENTATION_ITEM ( )  RATIONAL_B_SPLINE_SURFACE ( (
 ( 1.000000000000000000, 0.7460133799027759416, 1.000000000000000000),
 ( 1.000000000000000000, 0.7464018141889758873, 1.000000000000000000),
 ( 1.000000000000000000, 0.7343312752103077212, 1.000000000000000000),
 ( 1.000000000000000000, 0.7219065546282223966, 1.000000000000000000) ) ) 
 REPRESENTATION_ITEM ( '' )  SURFACE ( )  );
#6966 = CARTESIAN_POINT ( 'NONE',  ( 8.474859994195281132, 31.84143805560860940, 47.04930799450051637 ) ) ;
#6967 = CARTESIAN_POINT ( 'NONE',  ( 21.09992658989239089, 24.09184655352419213, 47.04930799450051637 ) ) ;
#6968 = DIRECTION ( 'NONE',  ( 0.000000000000000000, -1.000000000000000000, 0.000000000000000000 ) ) ;
#6969 = ORIENTED_EDGE ( 'NONE', *, *, #12260, .T. ) ;
#6970 = DIRECTION ( 'NONE',  ( -0.000000000000000000, -1.000000000000000000, 0.000000000000000000 ) ) ;
#6971 = ORIENTED_EDGE ( 'NONE', *, *, #11130, .F. ) ;
#6972 = DIRECTION ( 'NONE',  ( -0.000000000000000000, -1.000000000000000000, 0.000000000000000000 ) ) ;
#6973 = CARTESIAN_POINT ( 'NONE',  ( -40.68422973805265030, 6.807290781432339344, 39.54930799450052348 ) ) ;
#6974 = ADVANCED_FACE ( 'NONE', ( #26329 ), #19339, .T. ) ;
#6975 = CARTESIAN_POINT ( 'NONE',  ( 72.15764468888175998, 11.56063108660457495, 70.19967134400259567 ) ) ;
#6976 = ORIENTED_EDGE ( 'NONE', *, *, #28609, .F. ) ;
#6977 = CARTESIAN_POINT ( 'NONE',  ( 33.72499318558949000, 38.56284415653841791, 47.04930799450051637 ) ) ;
#6978 = DIRECTION ( 'NONE',  ( 1.000000000000000000, 0.000000000000000000, -1.224646799147353207E-16 ) ) ;
#6979 = PRESENTATION_STYLE_ASSIGNMENT (( #11743 ) ) ;
#6980 = DIRECTION ( 'NONE',  ( -0.000000000000000000, -1.000000000000000000, 0.000000000000000000 ) ) ;
#6981 = DIRECTION ( 'NONE',  ( 0.000000000000000000, 1.000000000000000000, -0.000000000000000000 ) ) ;
#6982 = DIRECTION ( 'NONE',  ( -1.101824276508909887E-16, 1.000000000000000000, -0.000000000000000000 ) ) ;
#6983 = AXIS2_PLACEMENT_3D ( 'NONE', #23128, #18671, #28693 ) ;
#6984 = SURFACE_STYLE_FILL_AREA ( #29475 ) ;
#6985 = ORIENTED_EDGE ( 'NONE', *, *, #19979, .F. ) ;
#6986 = LINE ( 'NONE', #31773, #18413 ) ;
#6987 = CARTESIAN_POINT ( 'NONE',  ( 21.09992658989238734, 38.56284415653841791, 47.04930799450051637 ) ) ;
#6988 = ORIENTED_EDGE ( 'NONE', *, *, #28124, .T. ) ;
#6989 = DIRECTION ( 'NONE',  ( -1.000000000000000000, -1.101824276508909887E-16, 0.000000000000000000 ) ) ;
#6990 = DIRECTION ( 'NONE',  ( -0.2756373558169954441, 0.9612616959383198934, -1.479773560108263204E-16 ) ) ;
#6991 = ORIENTED_EDGE ( 'NONE', *, *, #27507, .F. ) ;
#6992 = AXIS2_PLACEMENT_3D ( 'NONE', #1865, #16470, #31585 ) ;
#6993 = VECTOR ( 'NONE', #29025, 1000.000000000000000 ) ;
#6994 = EDGE_CURVE ( 'NONE', #8369, #12497, #24183, .T. ) ;
#6995 = ORIENTED_EDGE ( 'NONE', *, *, #15437, .T. ) ;
#6996 = ADVANCED_FACE ( 'NONE', ( #13705 ), #28961, .F. ) ;
#6997 = VERTEX_POINT ( 'NONE', #8763 ) ;
#6998 = EDGE_CURVE ( 'NONE', #27103, #29811, #2370, .T. ) ;
#6999 = EDGE_CURVE ( 'NONE', #26617, #15153, #31107, .T. ) ;
#7000 = CIRCLE ( 'NONE', #17478, 43.00000000000000000 ) ;
#7001 = FACE_OUTER_BOUND ( 'NONE', #28482, .T. ) ;
#7002 = ORIENTED_EDGE ( 'NONE', *, *, #22194, .F. ) ;
#7003 = EDGE_LOOP ( 'NONE', ( #16498, #23640, #17082, #9718 ) ) ;
#7004 = FACE_OUTER_BOUND ( 'NONE', #8633, .T. ) ;
#7005 = AXIS2_PLACEMENT_3D ( 'NONE', #22559, #248, #89 ) ;
#7006 = CARTESIAN_POINT ( 'NONE',  ( 46.98893894479710553, 19.86454579224779948, 49.14648158776898867 ) ) ;
#7007 = AXIS2_PLACEMENT_3D ( 'NONE', #29234, #14145, #14308 ) ;
#7008 = CARTESIAN_POINT ( 'NONE',  ( 21.09785597605720753, -14.04221034894631615, 105.7124997376166391 ) ) ;
#7009 = DIRECTION ( 'NONE',  ( -1.101824276508909887E-16, 1.000000000000000000, -0.000000000000000000 ) ) ;
#7010 = CARTESIAN_POINT ( 'NONE',  ( 45.81741271322955100, 25.00122849631043565, 49.02305402274571122 ) ) ;
#7011 = EDGE_CURVE ( 'NONE', #32358, #10736, #27293, .T. ) ;
#7012 = EDGE_LOOP ( 'NONE', ( #12862, #9503, #20635, #6985 ) ) ;
#7013 = DIRECTION ( 'NONE',  ( -1.000000000000000000, 0.000000000000000000, 0.000000000000000000 ) ) ;
#7014 = ORIENTED_EDGE ( 'NONE', *, *, #11648, .F. ) ;
#7015 = LINE ( 'NONE', #16528, #1713 ) ;
#7016 = ORIENTED_EDGE ( 'NONE', *, *, #15204, .F. ) ;
#7017 = CARTESIAN_POINT ( 'NONE',  ( 47.09785597605719687, 25.16454579224780019, 47.04930799450078638 ) ) ;
#7018 = CARTESIAN_POINT ( 'NONE',  ( -40.70335362822509495, 9.387769322903325886, 39.54930799450052348 ) ) ;
#7019 = CARTESIAN_POINT ( 'NONE',  ( 52.07920815280782989, -5.935668478901860112, 107.6362644806661990 ) ) ;
#7020 = DIRECTION ( 'NONE',  ( -0.000000000000000000, -1.000000000000000000, -0.000000000000000000 ) ) ;
#7021 = CARTESIAN_POINT ( 'NONE',  ( 21.09992658989239089, 26.46183152705960140, 47.04930799450051637 ) ) ;
#7022 = CARTESIAN_POINT ( 'NONE',  ( 49.41945501136223839, 27.06454579807170902, 45.86501535757901848 ) ) ;
#7023 = CARTESIAN_POINT ( 'NONE',  ( 46.86059137560834387, 22.89977464660286444, 48.89819542093576388 ) ) ;
#7024 = LINE ( 'NONE', #17020, #6993 ) ;
#7025 = EDGE_LOOP ( 'NONE', ( #13740, #31535, #6949, #5275 ) ) ;
#7026 = CARTESIAN_POINT ( 'NONE',  ( 47.16329704288476421, 29.59056480653310217, 44.97634117946077481 ) ) ;
#7027 = FACE_OUTER_BOUND ( 'NONE', #19247, .T. ) ;
#7028 = CARTESIAN_POINT ( 'NONE',  ( 21.09992658989238734, 38.56284415653841791, 47.04930799450051637 ) ) ;
#7029 = LINE ( 'NONE', #7193, #4841 ) ;
#7030 = LINE ( 'NONE', #17032, #28777 ) ;
#7031 = EDGE_LOOP ( 'NONE', ( #5354, #7973, #24362, #9616 ) ) ;
#7032 = AXIS2_PLACEMENT_3D ( 'NONE', #12316, #12153, #2296 ) ;
#7033 = ADVANCED_FACE ( 'NONE', ( #11391 ), #11240, .T. ) ;
#7034 = VERTEX_POINT ( 'NONE', #6633 ) ;
#7035 = CARTESIAN_POINT ( 'NONE',  ( 21.09992658989239089, 28.34143805560861296, 47.04930799450051637 ) ) ;
#7036 = EDGE_CURVE ( 'NONE', #13067, #25764, #18002, .T. ) ;
#7037 = ORIENTED_EDGE ( 'NONE', *, *, #6859, .T. ) ;
#7038 = EDGE_CURVE ( 'NONE', #10115, #7900, #1507, .T. ) ;
#7039 = EDGE_CURVE ( 'NONE', #20933, #20144, #16186, .T. ) ;
#7040 = ORIENTED_EDGE ( 'NONE', *, *, #3021, .F. ) ;
#7041 = CARTESIAN_POINT ( 'NONE',  ( 21.09992658989239089, 24.21183152705959785, 47.04930799450051637 ) ) ;
#7042 = FACE_OUTER_BOUND ( 'NONE', #10643, .T. ) ;
#7043 = FACE_OUTER_BOUND ( 'NONE', #8677, .T. ) ;
#7044 = ORIENTED_EDGE ( 'NONE', *, *, #19696, .F. ) ;
#7045 = AXIS2_PLACEMENT_3D ( 'NONE', #6603, #1346, #28931 ) ;
#7046 = DIRECTION ( 'NONE',  ( -0.000000000000000000, -1.000000000000000000, 0.000000000000000000 ) ) ;
#7047 = AXIS2_PLACEMENT_3D ( 'NONE', #1471, #11489, #30720 ) ;
#7048 = CYLINDRICAL_SURFACE ( 'NONE', #5514, 10.00000000000000178 ) ;
#7049 = CARTESIAN_POINT ( 'NONE',  ( 21.09785597605719332, 15.43591091851533115, 47.04930799450051637 ) ) ;
#7050 = AXIS2_PLACEMENT_3D ( 'NONE', #18302, #10294, #2567 ) ;
#7051 = EDGE_LOOP ( 'NONE', ( #1579, #28415, #29978, #19054 ) ) ;
#7052 = ORIENTED_EDGE ( 'NONE', *, *, #4157, .F. ) ;
#7054 = CARTESIAN_POINT ( 'NONE',  ( 33.50134396954522487, 29.09164230456639899, 47.04930799450051637 ) ) ;
#7053 = TOROIDAL_SURFACE ( 'NONE', #12834, 0.2000000000000000111, 0.1000000000000000056 ) ;
#7055 = VECTOR ( 'NONE', #30217, 1000.000000000000000 ) ;
#7056 = VERTEX_POINT ( 'NONE', #7288 ) ;
#7057 = CARTESIAN_POINT ( 'NONE',  ( 21.09785597605719332, 12.78350261226561280, 47.04930799450051637 ) ) ;
#7058 = AXIS2_PLACEMENT_3D ( 'NONE', #16592, #16919, #9383 ) ;
#7059 = DIRECTION ( 'NONE',  ( 0.000000000000000000, 0.000000000000000000, -1.000000000000000000 ) ) ;
#7060 = DIRECTION ( 'NONE',  ( -1.000000000000000000, 0.000000000000000000, 0.000000000000000000 ) ) ;
#7061 = FACE_OUTER_BOUND ( 'NONE', #1089, .T. ) ;
#7062 = CARTESIAN_POINT ( 'NONE',  ( 0.000000000000000000, 0.000000000000000000, 0.000000000000000000 ) ) ;
#7063 = ORIENTED_EDGE ( 'NONE', *, *, #4627, .T. ) ;
#7064 = ORIENTED_EDGE ( 'NONE', *, *, #4371, .F. ) ;
#7065 = DIRECTION ( 'NONE',  ( -1.224646799147353207E-16, -1.349345573449484691E-32, 1.000000000000000000 ) ) ;
#7066 = CARTESIAN_POINT ( 'NONE',  ( 49.00637973737335074, 24.76454579224779806, 50.79063624159320511 ) ) ;
#7067 = LINE ( 'NONE', #17561, #25617 ) ;
#7068 = VERTEX_POINT ( 'NONE', #32241 ) ;
#7069 = DIRECTION ( 'NONE',  ( -0.000000000000000000, 1.000000000000000000, -0.000000000000000000 ) ) ;
#7070 = CARTESIAN_POINT ( 'NONE',  ( -5.602943079677954685, 9.702389020015065313, 97.51081847724526597 ) ) ;
#7071 = ADVANCED_FACE ( 'NONE', ( #4989 ), #22533, .T. ) ;
#7072 = ORIENTED_EDGE ( 'NONE', *, *, #5793, .T. ) ;
#7073 = DIRECTION ( 'NONE',  ( -0.6797146636928675933, -0.1949050434465284254, 0.7071067811865466846 ) ) ;
#7074 = CARTESIAN_POINT ( 'NONE',  ( 49.41945501136223839, 25.66454579807171044, 45.86501535757901848 ) ) ;
#7075 = DIRECTION ( 'NONE',  ( -1.000000000000000000, 0.000000000000000000, 0.000000000000000000 ) ) ;
#7076 = AXIS2_PLACEMENT_3D ( 'NONE', #24647, #22176, #32204 ) ;
#7077 = AXIS2_PLACEMENT_3D ( 'NONE', #6090, #678, #28254 ) ;
#7078 = CIRCLE ( 'NONE', #26475, 12.62506659569710266 ) ;
#7079 = VECTOR ( 'NONE', #30277, 1000.000000000000114 ) ;
#7080 = ADVANCED_FACE ( 'NONE', ( #9421, #12542 ), #62, .F. ) ;
#7081 = AXIS2_PLACEMENT_3D ( 'NONE', #2604, #9670, #12633 ) ;
#7082 = ORIENTED_EDGE ( 'NONE', *, *, #22974, .F. ) ;
#7083 = DIRECTION ( 'NONE',  ( -1.000000000000000000, 0.000000000000000000, 0.000000000000000000 ) ) ;
#7084 = CARTESIAN_POINT ( 'NONE',  ( -41.52218637998915085, 11.15499190493234671, 37.04930799450052348 ) ) ;
#7085 = DIRECTION ( 'NONE',  ( -1.101824276508909887E-16, 1.000000000000000000, -0.000000000000000000 ) ) ;
#7086 = CARTESIAN_POINT ( 'NONE',  ( 45.24946171279598417, 27.10784706826093071, 47.99220971130007030 ) ) ;
#7087 = EDGE_LOOP ( 'NONE', ( #32060, #1150 ) ) ;
#7088 = CARTESIAN_POINT ( 'NONE',  ( 21.09785597605718976, 6.671061906060458568, 67.63280429334794519 ) ) ;
#7089 = DIRECTION ( 'NONE',  ( 0.000000000000000000, -4.336808689941893885E-15, -1.000000000000000000 ) ) ;
#7090 = FACE_OUTER_BOUND ( 'NONE', #30358, .T. ) ;
#7091 = DIRECTION ( 'NONE',  ( -1.224646799147353207E-16, -1.349345573449484691E-32, 1.000000000000000000 ) ) ;
#7092 = FACE_OUTER_BOUND ( 'NONE', #10589, .T. ) ;
#7093 = CARTESIAN_POINT ( 'NONE',  ( -17.37805493069431151, -13.74047052604243646, 90.91442668615566447 ) ) ;
#7094 = PLANE ( 'NONE',  #1581 ) ;
#7095 = AXIS2_PLACEMENT_3D ( 'NONE', #16200, #16675, #31156 ) ;
#7096 = DIRECTION ( 'NONE',  ( 0.000000000000000000, 1.000000000000000000, -0.000000000000000000 ) ) ;
#7097 = DIRECTION ( 'NONE',  ( -0.000000000000000000, -1.000000000000000000, 0.000000000000000000 ) ) ;
#7098 = CIRCLE ( 'NONE', #9181, 0.09999999999999766020 ) ;
#7099 = FILL_AREA_STYLE_COLOUR ( '', #29650 ) ;
#7100 = VERTEX_POINT ( 'NONE', #30106 ) ;
#7101 = CARTESIAN_POINT ( 'NONE',  ( 45.45032030167665482, 22.91413368675619111, 46.31675765204602868 ) ) ;
#7102 = CIRCLE ( 'NONE', #16527, 12.62506659569710266 ) ;
#7103 = CARTESIAN_POINT ( 'NONE',  ( 46.93316184409368930, 25.34819976284614640, 50.22046065185270436 ) ) ;
#7104 = CARTESIAN_POINT ( 'NONE',  ( -29.34881829548723786, 9.303215551142470119, 19.84796387032580967 ) ) ;
#7105 = AXIS2_PLACEMENT_3D ( 'NONE', #3482, #13033, #28282 ) ;
#7106 = CARTESIAN_POINT ( 'NONE',  ( 54.77221030306374416, -1.714651486836145322, 100.7893516206941342 ) ) ;
#7107 = ORIENTED_EDGE ( 'NONE', *, *, #3600, .T. ) ;
#7108 = CARTESIAN_POINT ( 'NONE',  ( 21.09992658989239089, 28.71183152705961206, 47.04930799450051637 ) ) ;
#7109 = DIRECTION ( 'NONE',  ( 0.000000000000000000, 0.000000000000000000, -1.000000000000000000 ) ) ;
#7110 = CARTESIAN_POINT ( 'NONE',  ( -43.37834615508418068, 1.121909970995877526, 39.54930799450052348 ) ) ;
#7111 = ORIENTED_EDGE ( 'NONE', *, *, #23868, .F. ) ;
#7112 = VERTEX_POINT ( 'NONE', #19740 ) ;
#7113 = CARTESIAN_POINT ( 'NONE',  ( -40.17244512953781310, 6.931285263614340941, 39.54930799450052348 ) ) ;
#7114 = CARTESIAN_POINT ( 'NONE',  ( 45.35708200440645044, 29.09118040159425789, 45.92000246470679770 ) ) ;
#7115 = CARTESIAN_POINT ( 'NONE',  ( 8.698509210239503631, 23.84164230456639544, 47.04930799450051637 ) ) ;
#7116 = AXIS2_PLACEMENT_3D ( 'NONE', #22131, #29369, #14766 ) ;
#7117 = CARTESIAN_POINT ( 'NONE',  ( 21.09785597605720753, 13.86454579224779948, 47.04930799450052348 ) ) ;
#7118 = CARTESIAN_POINT ( 'NONE',  ( -42.37913764077812573, 15.23192269303852697, 38.44930799450052916 ) ) ;
#7119 = ORIENTED_EDGE ( 'NONE', *, *, #23968, .T. ) ;
#7120 = EDGE_CURVE ( 'NONE', #10702, #321, #18796, .T. ) ;
#7121 = ORIENTED_EDGE ( 'NONE', *, *, #10321, .T. ) ;
#7122 = EDGE_CURVE ( 'NONE', #17663, #16815, #28264, .T. ) ;
#7123 = EDGE_CURVE ( 'NONE', #29537, #3515, #15676, .T. ) ;
#7124 = EDGE_CURVE ( 'NONE', #7136, #14930, #4136, .T. ) ;
#7125 = EDGE_CURVE ( 'NONE', #31589, #15480, #30248, .T. ) ;
#7126 = CARTESIAN_POINT ( 'NONE',  ( 52.16615856333482526, -5.937394852768787423, 107.6772108465075490 ) ) ;
#7127 = EDGE_CURVE ( 'NONE', #16912, #27697, #12419, .T. ) ;
#7128 = AXIS2_PLACEMENT_3D ( 'NONE', #6581, #29223, #1972 ) ;
#7129 = AXIS2_PLACEMENT_3D ( 'NONE', #2139, #16726, #1969 ) ;
#7130 = ORIENTED_EDGE ( 'NONE', *, *, #20443, .T. ) ;
#7131 = DIRECTION ( 'NONE',  ( 0.2756373558169974425, -0.9612616959383193382, 0.000000000000000000 ) ) ;
#7132 = CARTESIAN_POINT ( 'NONE',  ( -30.97925791506041904, 2.249770678923472378, 79.23692945862572401 ) ) ;
#7133 = AXIS2_PLACEMENT_3D ( 'NONE', #15327, #2206, #17125 ) ;
#7134 = EDGE_LOOP ( 'NONE', ( #13048, #22772 ) ) ;
#7135 = CYLINDRICAL_SURFACE ( 'NONE', #13397, 0.1000000000000018235 ) ;
#7136 = VERTEX_POINT ( 'NONE', #219 ) ;
#7137 = DIRECTION ( 'NONE',  ( -0.000000000000000000, -1.000000000000000000, -0.000000000000000000 ) ) ;
#7138 = CARTESIAN_POINT ( 'NONE',  ( -41.88090303775678080, 13.82677487427665497, 59.44930799450051495 ) ) ;
#7139 = DIRECTION ( 'NONE',  ( 0.000000000000000000, -1.000000000000000000, 0.000000000000000000 ) ) ;
#7140 = ORIENTED_EDGE ( 'NONE', *, *, #5320, .F. ) ;
#7141 = DIRECTION ( 'NONE',  ( 0.000000000000000000, 0.000000000000000000, -1.000000000000000000 ) ) ;
#7142 = DIRECTION ( 'NONE',  ( -1.101824276508909887E-16, 1.000000000000000000, -0.000000000000000000 ) ) ;
#7143 = CARTESIAN_POINT ( 'NONE',  ( -9.905649660384604260, -5.936382080411358508, -13.56946478339649964 ) ) ;
#7144 = CYLINDRICAL_SURFACE ( 'NONE', #28428, 2.000000000000001776 ) ;
#7145 = DIRECTION ( 'NONE',  ( -0.8746197071393926326, 0.4848096202463430537, 8.676864087101709653E-18 ) ) ;
#7146 = DIRECTION ( 'NONE',  ( -0.2756373558170082672, 0.9612616959383162296, 0.000000000000000000 ) ) ;
#7147 = EDGE_LOOP ( 'NONE', ( #8126, #7980, #7277, #25868 ) ) ;
#7148 = DIRECTION ( 'NONE',  ( 0.000000000000000000, 0.000000000000000000, -1.000000000000000000 ) ) ;
#7149 = CARTESIAN_POINT ( 'NONE',  ( 21.09785597605720753, 15.11603238453479037, 47.04930799450052348 ) ) ;
#7150 = ORIENTED_EDGE ( 'NONE', *, *, #25244, .T. ) ;
#7152 = EDGE_CURVE ( 'NONE', #22214, #21573, #11887, .T. ) ;
#7151 = CARTESIAN_POINT ( 'NONE',  ( 34.29950969015404638, 17.36467600858027183, 47.04930799450052348 ) ) ;
#7153 = FACE_OUTER_BOUND ( 'NONE', #27737, .T. ) ;
#7154 = VERTEX_POINT ( 'NONE', #374 ) ;
#7155 = EDGE_LOOP ( 'NONE', ( #1198, #12944 ) ) ;
#7156 = PRODUCT_DEFINITION_CONTEXT ( 'detailed design', #29222, 'design' ) ;
#7157 = AXIS2_PLACEMENT_3D ( 'NONE', #7057, #24948, #12480 ) ;
#7158 = ORIENTED_EDGE ( 'NONE', *, *, #5, .F. ) ;
#7159 = EDGE_CURVE ( 'NONE', #26439, #16663, #23923, .T. ) ;
#7160 = EDGE_CURVE ( 'NONE', #20645, #4648, #17613, .T. ) ;
#7161 = EDGE_CURVE ( 'NONE', #4474, #27343, #13472, .T. ) ;
#7162 = DIRECTION ( 'NONE',  ( -1.000000000000000000, 0.000000000000000000, 0.000000000000000000 ) ) ;
#7163 = AXIS2_PLACEMENT_3D ( 'NONE', #16061, #7885, #30367 ) ;
#7164 = ORIENTED_EDGE ( 'NONE', *, *, #11045, .F. ) ;
#7165 = ORIENTED_EDGE ( 'NONE', *, *, #3477, .F. ) ;
#7166 = CARTESIAN_POINT ( 'NONE',  ( 76.06281145073309347, -3.543532154952161228, 13.42751279571587375 ) ) ;
#7167 = CARTESIAN_POINT ( 'NONE',  ( 33.72499318558949000, 38.56284415653841791, 47.04930799450051637 ) ) ;
#7168 = DIRECTION ( 'NONE',  ( -2.779292025043186357E-18, 1.288349127009862211E-17, -1.000000000000000000 ) ) ;
#7169 = FACE_OUTER_BOUND ( 'NONE', #15398, .T. ) ;
#7170 = DIRECTION ( 'NONE',  ( -1.101824276508909887E-16, 1.000000000000000000, -0.000000000000000000 ) ) ;
#7171 = VERTEX_POINT ( 'NONE', #5316 ) ;
#7172 = DIRECTION ( 'NONE',  ( -1.000000000000000000, 0.000000000000000000, -1.224646799147353207E-16 ) ) ;
#7173 = VERTEX_POINT ( 'NONE', #5147 ) ;
#7174 = DIRECTION ( 'NONE',  ( -0.000000000000000000, -1.000000000000000000, 0.000000000000000000 ) ) ;
#7175 = CARTESIAN_POINT ( 'NONE',  ( -40.57832940339291383, 7.446916344587776848, 60.44930799450051495 ) ) ;
#7176 = ORIENTED_EDGE ( 'NONE', *, *, #14270, .T. ) ;
#7177 = DIRECTION ( 'NONE',  ( 0.000000000000000000, -0.000000000000000000, -1.000000000000000000 ) ) ;
#7178 = CARTESIAN_POINT ( 'NONE',  ( -40.23971823762673239, 6.784144620117122493, 53.64930799450051779 ) ) ;
#7179 = AXIS2_PLACEMENT_3D ( 'NONE', #30869, #22665, #339 ) ;
#7180 = CARTESIAN_POINT ( 'NONE',  ( 21.09992658989239089, 27.96183152705961206, 47.04930799450051637 ) ) ;
#7181 = CARTESIAN_POINT ( 'NONE',  ( 8.732853799281734553, 38.56284415653841791, 47.04930799450051637 ) ) ;
#7182 = CARTESIAN_POINT ( 'NONE',  ( 46.72376704384358703, 22.91413368675619111, 48.81312807415246624 ) ) ;
#7183 = CARTESIAN_POINT ( 'NONE',  ( 48.18662509608405031, 26.49624452788248874, 49.18364984542562013 ) ) ;
#7184 = CARTESIAN_POINT ( 'NONE',  ( 47.59795910211924763, 22.99884124225578219, 48.37376509570535887 ) ) ;
#7185 = DIRECTION ( 'NONE',  ( -1.101824276508909887E-16, 1.000000000000000000, -0.000000000000000000 ) ) ;
#7186 = ORIENTED_EDGE ( 'NONE', *, *, #4340, .T. ) ;
#7187 = CARTESIAN_POINT ( 'NONE',  ( 21.09785597605719332, 24.86454579224779948, 47.04930799450051637 ) ) ;
#7189 = ADVANCED_FACE ( 'NONE', ( #25333 ), #24994, .T. ) ;
#7188 = DIRECTION ( 'NONE',  ( -1.224646799147353207E-16, -1.349345573449484691E-32, 1.000000000000000000 ) ) ;
#7190 = ORIENTED_EDGE ( 'NONE', *, *, #11165, .F. ) ;
#7191 = CARTESIAN_POINT ( 'NONE',  ( 21.09785597605719332, 40.56454579224779877, 47.04930799450051637 ) ) ;
#7192 = EDGE_CURVE ( 'NONE', #24444, #32232, #26255, .T. ) ;
#7193 = CARTESIAN_POINT ( 'NONE',  ( 8.474859994195282908, 38.56284415653841791, 47.04930799450051637 ) ) ;
#7194 = CARTESIAN_POINT ( 'NONE',  ( 8.732853799281736329, 25.47145308207319303, 47.04930799450051637 ) ) ;
#7195 = ORIENTED_EDGE ( 'NONE', *, *, #10167, .F. ) ;
#7196 = ORIENTED_EDGE ( 'NONE', *, *, #2311, .F. ) ;
#7197 = CARTESIAN_POINT ( 'NONE',  ( -42.36691375901575185, 13.72999064396537250, 54.61480954800870791 ) ) ;
#7198 = AXIS2_PLACEMENT_3D ( 'NONE', #13851, #30932, #20905 ) ;
#7199 = ORIENTED_EDGE ( 'NONE', *, *, #15196, .T. ) ;
#7200 = CIRCLE ( 'NONE', #25034, 12.36707279061065279 ) ;
#7201 = EDGE_CURVE ( 'NONE', #12012, #11938, #4552, .T. ) ;
#7202 = PRODUCT ( 'MAT-060', 'MAT-060', '', ( #17394 ) ) ;
#7203 = EDGE_LOOP ( 'NONE', ( #21805, #31449, #23804, #17681 ) ) ;
#7204 = CARTESIAN_POINT ( 'NONE',  ( 46.48525799733394592, 23.04411619146717882, 47.99360027521537830 ) ) ;
#7205 = CARTESIAN_POINT ( 'NONE',  ( 56.35042632428687881, -3.295808585244886402, -12.70392589783158499 ) ) ;
#7206 = ORIENTED_EDGE ( 'NONE', *, *, #13825, .T. ) ;
#7207 = DIRECTION ( 'NONE',  ( -1.000000000000000000, 0.000000000000000000, 0.000000000000000000 ) ) ;
#7208 = DIRECTION ( 'NONE',  ( -1.000000000000000000, 0.000000000000000000, 0.000000000000000000 ) ) ;
#7209 = DIRECTION ( 'NONE',  ( -0.4848096202463431648, -0.8746197071393924105, 0.000000000000000000 ) ) ;
#7210 = ADVANCED_FACE ( 'NONE', ( #27074 ), #4010, .T. ) ;
#7211 = CARTESIAN_POINT ( 'NONE',  ( 46.99023568444673060, 25.03791119454915659, 49.12151524109405898 ) ) ;
#7212 = ORIENTED_EDGE ( 'NONE', *, *, #11607, .F. ) ;
#7213 = VECTOR ( 'NONE', #18709, 1000.000000000000114 ) ;
#7214 = ORIENTED_EDGE ( 'NONE', *, *, #29534, .F. ) ;
#7215 = CYLINDRICAL_SURFACE ( 'NONE', #26964, 30.00000000000000711 ) ;
#7216 = CIRCLE ( 'NONE', #12478, 29.01837281655233269 ) ;
#7217 = ORIENTED_EDGE ( 'NONE', *, *, #18967, .T. ) ;
#7218 = EDGE_CURVE ( 'NONE', #8103, #14337, #31804, .T. ) ;
#7219 = FACE_OUTER_BOUND ( 'NONE', #12930, .T. ) ;
#7220 = CYLINDRICAL_SURFACE ( 'NONE', #13920, 12.36707279061065101 ) ;
#7221 = DIRECTION ( 'NONE',  ( 3.761114140369701376E-15, 1.000000000000000000, 0.000000000000000000 ) ) ;
#7222 = CIRCLE ( 'NONE', #5112, 0.1250000000000001110 ) ;
#7223 = DIRECTION ( 'NONE',  ( -0.4848096202463429427, -0.8746197071393925215, 2.352477780477436294E-16 ) ) ;
#7224 = CARTESIAN_POINT ( 'NONE',  ( 49.49063479933183629, 28.01291119454915091, 47.17357720316391578 ) ) ;
#7225 = DIRECTION ( 'NONE',  ( 1.000000000000000000, 0.000000000000000000, 0.000000000000000000 ) ) ;
#7226 = ORIENTED_EDGE ( 'NONE', *, *, #25212, .T. ) ;
#7227 = VERTEX_POINT ( 'NONE', #9524 ) ;
#7228 = DIRECTION ( 'NONE',  ( -1.000000000000000000, -1.101824276508909887E-16, 0.000000000000000000 ) ) ;
#7229 = ADVANCED_FACE ( 'NONE', ( #7393 ), #8727, .T. ) ;
#7230 = DIRECTION ( 'NONE',  ( 0.000000000000000000, 0.000000000000000000, -1.000000000000000000 ) ) ;
#7231 = ADVANCED_FACE ( 'NONE', ( #29710 ), #24448, .F. ) ;
#7232 = CIRCLE ( 'NONE', #25052, 39.69941114636694124 ) ;
#7233 = EDGE_CURVE ( 'NONE', #26085, #27014, #7699, .T. ) ;
#7234 = CARTESIAN_POINT ( 'NONE',  ( -42.03703168893574116, 3.954238390689463145, 47.04930799450051637 ) ) ;
#7235 = ORIENTED_EDGE ( 'NONE', *, *, #26667, .F. ) ;
#7236 = CARTESIAN_POINT ( 'NONE',  ( 48.80698780008784610, 29.57276968525846073, 45.83340656927448009 ) ) ;
#7237 = CARTESIAN_POINT ( 'NONE',  ( 56.61384086331115384, -13.74047052604243646, 93.34357519277922677 ) ) ;
#7238 = ORIENTED_EDGE ( 'NONE', *, *, #24722, .T. ) ;
#7239 = CARTESIAN_POINT ( 'NONE',  ( 21.09785597605719332, 42.30003263981368633, 47.04930799450051637 ) ) ;
#7240 = DIRECTION ( 'NONE',  ( 0.000000000000000000, 0.000000000000000000, -1.000000000000000000 ) ) ;
#7241 = DIRECTION ( 'NONE',  ( 0.9915148059396263758, 0.1299938060159218089, -1.080935127887223745E-18 ) ) ;
#7242 = ADVANCED_FACE ( 'NONE', ( #7219 ), #12942, .F. ) ;
#7243 = AXIS2_PLACEMENT_3D ( 'NONE', #11468, #19167, #13781 ) ;
#7244 = CIRCLE ( 'NONE', #29235, 0.9999999999999998890 ) ;
#7245 = ORIENTED_EDGE ( 'NONE', *, *, #23027, .T. ) ;
#7246 = CIRCLE ( 'NONE', #18242, 1.100000000000000311 ) ;
#7247 = AXIS2_PLACEMENT_3D ( 'NONE', #18676, #26724, #4401 ) ;
#7248 = VERTEX_POINT ( 'NONE', #9687 ) ;
#7249 = CYLINDRICAL_SURFACE ( 'NONE', #22778, 71.29999999999996874 ) ;
#7250 = CARTESIAN_POINT ( 'NONE',  ( 49.64105649875294546, 24.93604219378083542, 46.47965702198763438 ) ) ;
#7251 = CARTESIAN_POINT ( 'NONE',  ( -41.96544240928614755, 13.75880317176705603, 59.54930799450050927 ) ) ;
#7252 = CIRCLE ( 'NONE', #7775, 12.78419020052701960 ) ;
#7253 = ORIENTED_EDGE ( 'NONE', *, *, #24639, .T. ) ;
#7254 = CARTESIAN_POINT ( 'NONE',  ( -40.45390504179176361, 8.517838719579989615, 39.46050754198200394 ) ) ;
#7255 = FACE_OUTER_BOUND ( 'NONE', #6145, .T. ) ;
#7256 = EDGE_CURVE ( 'NONE', #21115, #6406, #29178, .T. ) ;
#7257 = DIRECTION ( 'NONE',  ( 0.9612616959383205595, 0.2756373558169930571, -1.660411357259282199E-16 ) ) ;
#7258 = EDGE_CURVE ( 'NONE', #14586, #23429, #17220, .T. ) ;
#7259 = CARTESIAN_POINT ( 'NONE',  ( 21.09785597605719332, 40.56454579224780588, 47.04930799450051637 ) ) ;
#7260 = FACE_OUTER_BOUND ( 'NONE', #6685, .T. ) ;
#7261 = CARTESIAN_POINT ( 'NONE',  ( -40.50745992490246294, 7.570570027725508133, 60.23867152839895311 ) ) ;
#7262 = CARTESIAN_POINT ( 'NONE',  ( -29.43068460852080648, -13.74047052604243646, 17.87036105788322260 ) ) ;
#7263 = CYLINDRICAL_SURFACE ( 'NONE', #5797, 1.624998423334082620 ) ;
#7264 = FACE_OUTER_BOUND ( 'NONE', #19843, .T. ) ;
#7265 = DIRECTION ( 'NONE',  ( 0.1138751963119829791, -0.8685717160922530322, -0.4823024089401439785 ) ) ;
#7266 = SURFACE_SIDE_STYLE ('',( #19066 ) ) ;
#7267 = ORIENTED_EDGE ( 'NONE', *, *, #4107, .T. ) ;
#7268 = EDGE_LOOP ( 'NONE', ( #3605, #97, #2402, #30742 ) ) ;
#7269 = DIRECTION ( 'NONE',  ( -1.101824276508909887E-16, 1.000000000000000000, -0.000000000000000000 ) ) ;
#7270 = AXIS2_PLACEMENT_3D ( 'NONE', #23716, #1221, #11248 ) ;
#7271 = CARTESIAN_POINT ( 'NONE',  ( 49.62252444096254322, 24.84787913140503690, 48.68715535708000886 ) ) ;
#7272 = EDGE_CURVE ( 'NONE', #23768, #16751, #16075, .T. ) ;
#7273 = CARTESIAN_POINT ( 'NONE',  ( -40.14234630318158281, 6.912323292265332597, 34.55513836777664238 ) ) ;
#7274 = VECTOR ( 'NONE', #8847, 1000.000000000000000 ) ;
#7275 = EDGE_CURVE ( 'NONE', #3586, #8390, #17650, .T. ) ;
#7276 = CARTESIAN_POINT ( 'NONE',  ( 1.597855976057205973, 13.86454579224779948, 47.04930799450052348 ) ) ;
#7277 = ORIENTED_EDGE ( 'NONE', *, *, #31220, .T. ) ;
#7278 = CARTESIAN_POINT ( 'NONE',  ( -39.53644225062161155, -5.935901483590497740, 77.96306619390172443 ) ) ;
#7279 = CARTESIAN_POINT ( 'NONE',  ( 21.09785597605720753, 14.46497581658974063, 47.04930799450052348 ) ) ;
#7280 = LINE ( 'NONE', #17766, #13104 ) ;
#7281 = TOROIDAL_SURFACE ( 'NONE', #25611, 12.40141737965285706, 0.1250000000000007494 ) ;
#7282 = VERTEX_POINT ( 'NONE', #32173 ) ;
#7283 = ORIENTED_EDGE ( 'NONE', *, *, #19049, .T. ) ;
#7284 = CYLINDRICAL_SURFACE ( 'NONE', #24662, 2.000000000000001776 ) ;
#7285 = CARTESIAN_POINT ( 'NONE',  ( 33.50134396954519644, 31.09164230456639544, 47.04930799450051637 ) ) ;
#7286 = CARTESIAN_POINT ( 'NONE',  ( 33.72499318558949000, 38.56284415653841791, 47.04930799450051637 ) ) ;
#7287 = CARTESIAN_POINT ( 'NONE',  ( 47.19823469859255738, 22.88065857334294861, 45.11653766655789610 ) ) ;
#7288 = CARTESIAN_POINT ( 'NONE',  ( 48.23388202445966044, 28.92822092656773947, 49.27628909396054979 ) ) ;
#7289 = EDGE_LOOP ( 'NONE', ( #17602, #32411, #5861, #15706 ) ) ;
#7290 = EDGE_LOOP ( 'NONE', ( #6033, #24864, #15076, #20773 ) ) ;
#7291 = FACE_OUTER_BOUND ( 'NONE', #21147, .T. ) ;
#7292 = TOROIDAL_SURFACE ( 'NONE', #25125, 12.61792373059860495, 0.1250000000000008604 ) ;
#7293 = VERTEX_POINT ( 'NONE', #29551 ) ;
#7294 = CIRCLE ( 'NONE', #2037, 1.500000000000001332 ) ;
#7295 = CARTESIAN_POINT ( 'NONE',  ( 21.09992658989239089, 26.21664230456639899, 47.04930799450051637 ) ) ;
#7296 = CARTESIAN_POINT ( 'NONE',  ( 33.72499318558949710, 26.84184655352419568, 47.04930799450051637 ) ) ;
#7297 = ORIENTED_EDGE ( 'NONE', *, *, #4903, .F. ) ;
#7298 = VECTOR ( 'NONE', #4247, 1000.000000000000000 ) ;
#7299 = CARTESIAN_POINT ( 'NONE',  ( -40.85838585144898616, 8.484324852566594188, 34.62702073480610210 ) ) ;
#7300 = ORIENTED_EDGE ( 'NONE', *, *, #2553, .F. ) ;
#7301 = DIRECTION ( 'NONE',  ( 0.000000000000000000, 0.000000000000000000, -1.000000000000000000 ) ) ;
#7302 = TOROIDAL_SURFACE ( 'NONE', #1525, 12.61792373059898686, 0.1249999999999964195 ) ;
#7303 = DIRECTION ( 'NONE',  ( 0.000000000000000000, 1.000000000000000000, 0.000000000000000000 ) ) ;
#7304 = DIRECTION ( 'NONE',  ( 0.000000000000000000, 0.000000000000000000, -1.000000000000000000 ) ) ;
#7305 = VERTEX_POINT ( 'NONE', #30199 ) ;
#7306 = CARTESIAN_POINT ( 'NONE',  ( 72.55809747643107244, 4.272108154687154880, 78.09619054489033374 ) ) ;
#7307 = DIRECTION ( 'NONE',  ( -1.000000000000000000, 0.000000000000000000, 0.000000000000000000 ) ) ;
#7308 = CARTESIAN_POINT ( 'NONE',  ( 21.09992658989238734, 30.84164230456639544, 47.04930799450051637 ) ) ;
#7309 = DIRECTION ( 'NONE',  ( -1.000000000000000000, -1.101824276508909887E-16, 0.000000000000000000 ) ) ;
#7310 = EDGE_CURVE ( 'NONE', #3444, #20933, #25503, .T. ) ;
#7311 = CARTESIAN_POINT ( 'NONE',  ( 21.09992658989239089, 24.84164230456639544, 47.04930799450051637 ) ) ;
#7312 = CARTESIAN_POINT ( 'NONE',  ( 72.70371229542294600, 7.324825086315909672, 76.07540346930043995 ) ) ;
#7313 = EDGE_LOOP ( 'NONE', ( #21819, #2673, #27185, #18228 ) ) ;
#7314 = CARTESIAN_POINT ( 'NONE',  ( 21.09785597605719332, -15.93545420775219945, -34.66074251183835031 ) ) ;
#7315 = DIRECTION ( 'NONE',  ( -0.2756373558169900040, 0.9612616959383215587, 0.000000000000000000 ) ) ;
#7316 = ORIENTED_EDGE ( 'NONE', *, *, #5412, .T. ) ;
#7317 = DIRECTION ( 'NONE',  ( 0.000000000000000000, 0.000000000000000000, -1.000000000000000000 ) ) ;
#7318 = B_SPLINE_CURVE_WITH_KNOTS ( 'NONE', 3,
 ( #22551, #7639, #2703, #29962, #2538, #9930, #19930, #19762, #10421, #24866, #7963, #7306, #2385, #10103, #7477, #559, #15179, #27977, #5492, #15501, #12403, #239, #25511, #5013, #3010, #13049, #23040, #30125, #29793, #15023, #22387, #27648, #5172, #25191, #12733, #22724 ),
 .UNSPECIFIED., .F., .F.,
 ( 4, 2, 2, 2, 2, 2, 2, 2, 2, 2, 2, 2, 2, 2, 2, 2, 2, 4 ),
 ( 0.000000000000000000, 0.001327013081135465034, 0.002654026162270930068, 0.003981039243406394451, 0.005308052324541860136, 0.006635065405677324953, 0.007962078486812788902, 0.01061610464908372894, 0.01194311773021918509, 0.01327013081135464123, 0.01459714389249009564, 0.01592415697362555005, 0.01725117005476100446, 0.01857818313589645540, 0.01924168967646419648, 0.01990519621703193062, 0.02056870275759966823, 0.02123220929816740585 ),
 .UNSPECIFIED. ) ;
#7319 = AXIS2_PLACEMENT_3D ( 'NONE', #32390, #1863, #29270 ) ;
#7320 = CARTESIAN_POINT ( 'NONE',  ( -38.36853489569023168, 7.065850718397949315, 32.04930799450052348 ) ) ;
#7321 = ORIENTED_EDGE ( 'NONE', *, *, #11634, .T. ) ;
#7322 = ORIENTED_EDGE ( 'NONE', *, *, #7125, .T. ) ;
#7323 = VECTOR ( 'NONE', #27621, 1000.000000000000000 ) ;
#7324 = CIRCLE ( 'NONE', #6799, 0.1250000000000001110 ) ;
#7325 = ORIENTED_EDGE ( 'NONE', *, *, #9139, .T. ) ;
#7326 = AXIS2_PLACEMENT_3D ( 'NONE', #2107, #29529, #6879 ) ;
#7327 = CIRCLE ( 'NONE', #24609, 1.199999999999999734 ) ;
#7328 = DIRECTION ( 'NONE',  ( -0.000000000000000000, -1.000000000000000000, -0.000000000000000000 ) ) ;
#7329 = AXIS2_PLACEMENT_3D ( 'NONE', #29958, #12066, #30119 ) ;
#7330 = AXIS2_PLACEMENT_3D ( 'NONE', #3331, #20886, #31238 ) ;
#7331 = VERTEX_POINT ( 'NONE', #12314 ) ;
#7332 = VERTEX_POINT ( 'NONE', #32006 ) ;
#7333 = DIRECTION ( 'NONE',  ( -1.101824276508909887E-16, 1.000000000000000000, -0.000000000000000000 ) ) ;
#7334 = CARTESIAN_POINT ( 'NONE',  ( -43.97612096762308198, -5.099423983826959272, 52.41794874062419751 ) ) ;
#7335 = CARTESIAN_POINT ( 'NONE',  ( 8.096071960694297687, -5.098646251524523443, 47.04930799450052348 ) ) ;
#7336 = CARTESIAN_POINT ( 'NONE',  ( -41.08785830660042393, 9.277514380576530328, 38.60788663826321709 ) ) ;
#7337 = DIRECTION ( 'NONE',  ( 0.000000000000000000, 0.000000000000000000, 1.000000000000000000 ) ) ;
#7338 = ORIENTED_EDGE ( 'NONE', *, *, #32176, .T. ) ;
#7339 = DIRECTION ( 'NONE',  ( -1.224646799147353207E-16, -1.349345573449484691E-32, 1.000000000000000000 ) ) ;
#7340 = ORIENTED_EDGE ( 'NONE', *, *, #5753, .F. ) ;
#7341 = CARTESIAN_POINT ( 'NONE',  ( -36.86160217714372322, -5.510939734907921661, 14.80706798662212265 ) ) ;
#7342 = FACE_OUTER_BOUND ( 'NONE', #7492, .T. ) ;
#7343 = ORIENTED_EDGE ( 'NONE', *, *, #22973, .F. ) ;
#7344 = DIRECTION ( 'NONE',  ( 0.4544104193609912468, 5.611869858668455538E-17, 0.8907924397839084296 ) ) ;
#7345 = CARTESIAN_POINT ( 'NONE',  ( 33.50134396954523908, 27.34164230456639544, 47.04930799450051637 ) ) ;
#7346 = CIRCLE ( 'NONE', #17288, 0.1249999999999983763 ) ;
#7347 = LINE ( 'NONE', #4553, #16764 ) ;
#7348 = DIRECTION ( 'NONE',  ( -0.4848096202463424431, -0.8746197071393927436, 2.220446049250312588E-16 ) ) ;
#7349 = PLANE ( 'NONE',  #27419 ) ;
#7350 = EDGE_CURVE ( 'NONE', #3737, #30294, #23424, .T. ) ;
#7351 = CARTESIAN_POINT ( 'NONE',  ( 48.40186567930498285, 26.72957786121581947, 45.03923535223908203 ) ) ;
#7352 = EDGE_CURVE ( 'NONE', #15557, #14283, #20039, .T. ) ;
#7353 = VECTOR ( 'NONE', #3980, 1000.000000000000000 ) ;
#7354 = DIRECTION ( 'NONE',  ( 0.000000000000000000, 0.000000000000000000, 1.000000000000000000 ) ) ;
#7355 = LINE ( 'NONE', #30329, #10664 ) ;
#7356 = EDGE_CURVE ( 'NONE', #10177, #2557, #1380, .T. ) ;
#7357 = EDGE_CURVE ( 'NONE', #2614, #3078, #20272, .T. ) ;
#7358 = VERTEX_POINT ( 'NONE', #12010 ) ;
#7359 = AXIS2_PLACEMENT_3D ( 'NONE', #13931, #28863, #6374 ) ;
#7360 = CARTESIAN_POINT ( 'NONE',  ( 21.09785597605719332, -5.935454207752205669, 47.04930799450048085 ) ) ;
#7361 = AXIS2_PLACEMENT_3D ( 'NONE', #13661, #6262, #21178 ) ;
#7362 = CARTESIAN_POINT ( 'NONE',  ( 48.72149481846882679, 22.88065857334295217, 48.10262368218729279 ) ) ;
#7363 = ORIENTED_EDGE ( 'NONE', *, *, #20777, .F. ) ;
#7364 = CARTESIAN_POINT ( 'NONE',  ( 45.36511207810799107, 28.03213139976340429, 45.12672418911605376 ) ) ;
#7365 = DIRECTION ( 'NONE',  ( 0.2756373558170082672, -0.9612616959383162296, 0.000000000000000000 ) ) ;
#7366 = ORIENTED_EDGE ( 'NONE', *, *, #28288, .T. ) ;
#7367 =( BOUNDED_SURFACE ( )  B_SPLINE_SURFACE ( 3, 2, ( 
 ( #22814, #10349, #26410 ),
 ( #25921, #23465, #10843 ),
 ( #30703, #975, #20834 ),
 ( #3436, #5913, #13466 ) ),
 .UNSPECIFIED., .F., .F., .F. ) 
 B_SPLINE_SURFACE_WITH_KNOTS ( ( 4, 4 ),
 ( 3, 3 ),
 ( 0.0002661489594880761360, 0.0004225458590890279168 ),
 ( 0.000000000000000000, 1.000000000000000000 ),
 .UNSPECIFIED. ) 
 GEOMETRIC_REPRESENTATION_ITEM ( )  RATIONAL_B_SPLINE_SURFACE ( (
 ( 1.000000000000000000, 0.7219065546282040780, 1.000000000000000000),
 ( 1.000000000000000000, 0.7343063454201389506, 1.000000000000000000),
 ( 1.000000000000000000, 0.7464000351581004944, 1.000000000000000000),
 ( 1.000000000000000000, 0.7460133799027759416, 1.000000000000000000) ) ) 
 REPRESENTATION_ITEM ( '' )  SURFACE ( )  );
#7368 = ORIENTED_EDGE ( 'NONE', *, *, #4575, .T. ) ;
#7369 = DIRECTION ( 'NONE',  ( 1.000000000000000000, 0.000000000000000000, 0.000000000000000000 ) ) ;
#7370 = AXIS2_PLACEMENT_3D ( 'NONE', #24822, #7591, #29587 ) ;
#7371 = ORIENTED_EDGE ( 'NONE', *, *, #10587, .F. ) ;
#7372 = CIRCLE ( 'NONE', #28845, 12.36707279061065101 ) ;
#7373 = AXIS2_PLACEMENT_3D ( 'NONE', #27062, #5519, #2560 ) ;
#7374 = AXIS2_PLACEMENT_3D ( 'NONE', #6249, #28257, #6091 ) ;
#7375 = VERTEX_POINT ( 'NONE', #29575 ) ;
#7376 = AXIS2_PLACEMENT_3D ( 'NONE', #11746, #6982, #26843 ) ;
#7377 = CARTESIAN_POINT ( 'NONE',  ( 45.68457171659533600, 22.99884124225578574, 47.13247861182188103 ) ) ;
#7378 = VECTOR ( 'NONE', #30858, 999.9999999999998863 ) ;
#7379 = EDGE_CURVE ( 'NONE', #19462, #31503, #28134, .T. ) ;
#7380 = CARTESIAN_POINT ( 'NONE',  ( 21.09992658989239089, 25.34164230456639899, 47.04930799450051637 ) ) ;
#7381 = EDGE_CURVE ( 'NONE', #10189, #20217, #13711, .T. ) ;
#7382 = CIRCLE ( 'NONE', #17850, 12.36707279061065101 ) ;
#7383 = ORIENTED_EDGE ( 'NONE', *, *, #20755, .F. ) ;
#7384 = CARTESIAN_POINT ( 'NONE',  ( 21.09785597605720042, -14.04221034894631615, 47.04930799450051637 ) ) ;
#7385 = DIRECTION ( 'NONE',  ( -1.101824276508909887E-16, 1.000000000000000000, -0.000000000000000000 ) ) ;
#7386 = CARTESIAN_POINT ( 'NONE',  ( -40.47970302497626705, 7.463434137431151250, 60.44930799450051495 ) ) ;
#7387 = CARTESIAN_POINT ( 'NONE',  ( 46.99023568444673060, 27.13791119454915446, 49.12151524109405898 ) ) ;
#7388 = VERTEX_POINT ( 'NONE', #19544 ) ;
#7389 = EDGE_LOOP ( 'NONE', ( #18603, #32324, #24673, #17552 ) ) ;
#7390 = DIRECTION ( 'NONE',  ( -1.101824276508909887E-16, 1.000000000000000000, -0.000000000000000000 ) ) ;
#7391 = TOROIDAL_SURFACE ( 'NONE', #59, 12.40141737965283220, 0.1250000000000002498 ) ;
#7392 = EDGE_LOOP ( 'NONE', ( #26591, #27893, #18183, #30315 ) ) ;
#7393 = FACE_OUTER_BOUND ( 'NONE', #6697, .T. ) ;
#7394 = LINE ( 'NONE', #17388, #17043 ) ;
#7395 = FACE_OUTER_BOUND ( 'NONE', #4102, .T. ) ;
#7396 = CARTESIAN_POINT ( 'NONE',  ( 8.732853799281734553, 38.56284415653841791, 47.04930799450051637 ) ) ;
#7397 = CARTESIAN_POINT ( 'NONE',  ( 45.24946171279598417, 27.02124452788248732, 47.99220971130007740 ) ) ;
#7398 = EDGE_CURVE ( 'NONE', #13343, #2726, #22356, .T. ) ;
#7399 = ORIENTED_EDGE ( 'NONE', *, *, #24984, .T. ) ;
#7400 = ORIENTED_EDGE ( 'NONE', *, *, #18447, .F. ) ;
#7401 = LINE ( 'NONE', #10342, #19173 ) ;
#7402 = DIRECTION ( 'NONE',  ( 0.8746197071393926326, -0.4848096202463430537, -8.676864087101709653E-18 ) ) ;
#7403 = VECTOR ( 'NONE', #11745, 1000.000000000000114 ) ;
#7404 = CYLINDRICAL_SURFACE ( 'NONE', #10965, 12.36707279061065101 ) ;
#7405 = ORIENTED_EDGE ( 'NONE', *, *, #15588, .F. ) ;
#7406 = CARTESIAN_POINT ( 'NONE',  ( 52.20929446027399479, -5.935454354499447582, 107.4890962774978220 ) ) ;
#7407 = VECTOR ( 'NONE', #17843, 1000.000000000000000 ) ;
#7408 = VERTEX_POINT ( 'NONE', #17085 ) ;
#7409 = DIRECTION ( 'NONE',  ( 0.000000000000000000, 0.000000000000000000, -1.000000000000000000 ) ) ;
#7410 = CIRCLE ( 'NONE', #10032, 15.52755282421446026 ) ;
#7411 = DIRECTION ( 'NONE',  ( 0.000000000000000000, -0.000000000000000000, -1.000000000000000000 ) ) ;
#7412 = CIRCLE ( 'NONE', #1625, 2.500000000000002220 ) ;
#7413 = DIRECTION ( 'NONE',  ( -0.1949050434465282589, 0.6797146636928674823, 0.7071067811865470176 ) ) ;
#7414 = EDGE_CURVE ( 'NONE', #7845, #21311, #19872, .T. ) ;
#7415 = EDGE_CURVE ( 'NONE', #9903, #20095, #19206, .T. ) ;
#7416 = ORIENTED_EDGE ( 'NONE', *, *, #18980, .F. ) ;
#7417 = ORIENTED_EDGE ( 'NONE', *, *, #25528, .F. ) ;
#7418 = ADVANCED_FACE ( 'NONE', ( #22172 ), #26551, .T. ) ;
#7419 = CARTESIAN_POINT ( 'NONE',  ( 33.37634396954518934, 32.09164230456639899, 47.04930799450051637 ) ) ;
#7420 = CARTESIAN_POINT ( 'NONE',  ( 45.79384627280941089, 25.76618040159426570, 49.05938063676249072 ) ) ;
#7421 = EDGE_CURVE ( 'NONE', #8855, #28053, #32199, .T. ) ;
#7422 = ORIENTED_EDGE ( 'NONE', *, *, #31509, .F. ) ;
#7423 = AXIS2_PLACEMENT_3D ( 'NONE', #19931, #19765, #29963 ) ;
#7424 = AXIS2_PLACEMENT_3D ( 'NONE', #5020, #10272, #32268 ) ;
#7425 = FACE_OUTER_BOUND ( 'NONE', #7003, .T. ) ;
#7426 = CARTESIAN_POINT ( 'NONE',  ( -42.37913764077812573, 15.23192269303852875, 35.64930799450052490 ) ) ;
#7427 = B_SPLINE_CURVE_WITH_KNOTS ( 'NONE', 3,
 ( #613, #20947, #16026, #6176, #26194, #3230 ),
 .UNSPECIFIED., .F., .F.,
 ( 4, 2, 4 ),
 ( 0.000000000000000000, 0.5000000000000000000, 1.000000000000000000 ),
 .UNSPECIFIED. ) ;
#7428 = TOROIDAL_SURFACE ( 'NONE', #20808, 12.61792373059859607, 0.1249999999999979738 ) ;
#7429 = DIRECTION ( 'NONE',  ( -1.101824276508909887E-16, 1.000000000000000000, -0.000000000000000000 ) ) ;
#7430 = CARTESIAN_POINT ( 'NONE',  ( 48.23388202445966044, 27.65087065737811756, 49.27628909396056400 ) ) ;
#7431 = CARTESIAN_POINT ( 'NONE',  ( 21.09992658989238734, 31.72145308207317171, 47.04930799450051637 ) ) ;
#7432 = FACE_OUTER_BOUND ( 'NONE', #5440, .T. ) ;
#7433 = DIRECTION ( 'NONE',  ( 0.000000000000000000, -1.000000000000000000, 0.000000000000000000 ) ) ;
#7434 = DIRECTION ( 'NONE',  ( 0.2756373558169945559, -0.9612616959383202264, 0.000000000000000000 ) ) ;
#7435 = DIRECTION ( 'NONE',  ( 0.000000000000000000, 0.000000000000000000, -1.000000000000000000 ) ) ;
#7436 = DIRECTION ( 'NONE',  ( -1.101824276508909887E-16, 1.000000000000000000, -0.000000000000000000 ) ) ;
#7437 = EDGE_CURVE ( 'NONE', #11362, #25360, #13869, .T. ) ;
#7438 = ORIENTED_EDGE ( 'NONE', *, *, #11275, .T. ) ;
#7439 = ORIENTED_EDGE ( 'NONE', *, *, #31466, .F. ) ;
#7440 = DIRECTION ( 'NONE',  ( -1.101824276508909887E-16, 1.000000000000000000, -0.000000000000000000 ) ) ;
#7441 = AXIS2_PLACEMENT_3D ( 'NONE', #6861, #27530, #11941 ) ;
#7442 = CARTESIAN_POINT ( 'NONE',  ( 33.72499318558949710, 28.34184655352419213, 47.04930799450051637 ) ) ;
#7443 = CARTESIAN_POINT ( 'NONE',  ( 71.48501281440435662, -3.295808585244886402, 82.30187834273039016 ) ) ;
#7444 = ORIENTED_EDGE ( 'NONE', *, *, #2119, .T. ) ;
#7445 = DIRECTION ( 'NONE',  ( -0.000000000000000000, -1.000000000000000000, -0.000000000000000000 ) ) ;
#7446 = CARTESIAN_POINT ( 'NONE',  ( 21.09785597605720042, -16.63545420775220407, 47.04930799450051637 ) ) ;
#7447 = DIRECTION ( 'NONE',  ( 0.2756373558169974980, -0.9612616959383193382, -1.315048337272770589E-17 ) ) ;
#7448 = ORIENTED_EDGE ( 'NONE', *, *, #15523, .T. ) ;
#7449 = ORIENTED_EDGE ( 'NONE', *, *, #16659, .T. ) ;
#7450 = DIRECTION ( 'NONE',  ( -0.4848096202463424431, -0.8746197071393927436, 2.220446049250312588E-16 ) ) ;
#7451 = CARTESIAN_POINT ( 'NONE',  ( 46.00908685603034343, 29.73284706826092361, 44.91496614357595263 ) ) ;
#7452 = DIRECTION ( 'NONE',  ( -2.779292025043186357E-18, 1.288349127009862211E-17, -1.000000000000000000 ) ) ;
#7453 = LINE ( 'NONE', #4987, #25878 ) ;
#7454 = AXIS2_PLACEMENT_3D ( 'NONE', #1424, #6847, #19133 ) ;
#7455 = CARTESIAN_POINT ( 'NONE',  ( 73.09176707068579049, 11.92558985988973497, 26.63511333407100778 ) ) ;
#7456 = ORIENTED_EDGE ( 'NONE', *, *, #4334, .T. ) ;
#7457 = EDGE_CURVE ( 'NONE', #6508, #8606, #6121, .T. ) ;
#7458 = EDGE_CURVE ( 'NONE', #18578, #13589, #14518, .T. ) ;
#7459 = ORIENTED_EDGE ( 'NONE', *, *, #30696, .F. ) ;
#7460 = DIRECTION ( 'NONE',  ( -1.101824276508909887E-16, 1.000000000000000000, -0.000000000000000000 ) ) ;
#7461 = TOROIDAL_SURFACE ( 'NONE', #18454, 12.40141737965283575, 0.1250000000000000278 ) ;
#7462 = EDGE_CURVE ( 'NONE', #13441, #19026, #6642, .T. ) ;
#7463 = ORIENTED_EDGE ( 'NONE', *, *, #31023, .T. ) ;
#7464 = EDGE_CURVE ( 'NONE', #29193, #21016, #9264, .T. ) ;
#7465 = AXIS2_PLACEMENT_3D ( 'NONE', #19883, #15135, #9882 ) ;
#7466 = DIRECTION ( 'NONE',  ( -0.9612616959383200044, -0.2756373558169954996, 1.660411357259285896E-16 ) ) ;
#7467 = DIRECTION ( 'NONE',  ( -2.472450503250596893E-15, -7.226442137580869828E-16, 1.000000000000000000 ) ) ;
#7468 = CIRCLE ( 'NONE', #11146, 13.00000000000000533 ) ;
#7469 = VERTEX_POINT ( 'NONE', #7419 ) ;
#7470 = CARTESIAN_POINT ( 'NONE',  ( -40.86542064515101202, 8.501822640387086238, 34.64781247685129273 ) ) ;
#7471 = ORIENTED_EDGE ( 'NONE', *, *, #15012, .T. ) ;
#7472 = DIRECTION ( 'NONE',  ( -0.000000000000000000, -1.000000000000000000, 0.000000000000000000 ) ) ;
#7473 = CARTESIAN_POINT ( 'NONE',  ( -41.91739890389096956, 13.90674392281398930, 59.49868301348410426 ) ) ;
#7474 = CIRCLE ( 'NONE', #28951, 0.1250000000000001110 ) ;
#7475 = DIRECTION ( 'NONE',  ( -1.000000000000000000, 0.000000000000000000, 0.000000000000000000 ) ) ;
#7476 = ORIENTED_EDGE ( 'NONE', *, *, #20274, .T. ) ;
#7477 = CARTESIAN_POINT ( 'NONE',  ( 73.23467398643032311, 2.044662169668950646, 79.35654811903377492 ) ) ;
#7478 = DIRECTION ( 'NONE',  ( 0.03667427209081842304, 0.7071067811865463515, -0.7061550805358625116 ) ) ;
#7479 = CARTESIAN_POINT ( 'NONE',  ( 21.09785597605719332, 44.06454579224779877, 47.04930799450051637 ) ) ;
#7480 = CARTESIAN_POINT ( 'NONE',  ( 21.09992658989239089, 28.47145308207318237, 47.04930799450051637 ) ) ;
#7481 = CARTESIAN_POINT ( 'NONE',  ( 73.38832120396322978, 4.618558202237204924, 77.89250913842629132 ) ) ;
#7482 = EDGE_LOOP ( 'NONE', ( #14120, #15995, #8755, #21664 ) ) ;
#7483 = DIRECTION ( 'NONE',  ( -1.101824276508909887E-16, 1.000000000000000000, -0.000000000000000000 ) ) ;
#7484 = DIRECTION ( 'NONE',  ( 0.2530443915477140204, -0.8824706660164525207, 0.3965022818682459316 ) ) ;
#7485 = ORIENTED_EDGE ( 'NONE', *, *, #7192, .F. ) ;
#7486 = CARTESIAN_POINT ( 'NONE',  ( 21.09992658989239089, 24.09164230456639544, 47.04930799450051637 ) ) ;
#7487 = CARTESIAN_POINT ( 'NONE',  ( 33.71785032049099584, 30.21664230456641675, 47.04930799450051637 ) ) ;
#7488 = AXIS2_PLACEMENT_3D ( 'NONE', #11337, #9033, #29382 ) ;
#7489 = VERTEX_POINT ( 'NONE', #17415 ) ;
#7490 = PRODUCT ( 'Screw M5', 'Screw M5', '', ( #12815 ) ) ;
#7491 = FACE_OUTER_BOUND ( 'NONE', #13233, .T. ) ;
#7492 = EDGE_LOOP ( 'NONE', ( #14636, #27706, #30064, #12888 ) ) ;
#7493 = CIRCLE ( 'NONE', #25815, 12.51969897791880015 ) ;
#7494 = EDGE_CURVE ( 'NONE', #6454, #19454, #27435, .T. ) ;
#7495 = CIRCLE ( 'NONE', #31526, 16.99999999999999289 ) ;
#7496 = ORIENTED_EDGE ( 'NONE', *, *, #3846, .F. ) ;
#7497 = CIRCLE ( 'NONE', #8033, 12.27641737965283042 ) ;
#7498 = ADVANCED_FACE ( 'NONE', ( #10852 ), #26037, .T. ) ;
#7499 = DIRECTION ( 'NONE',  ( -2.779292025043186357E-18, 1.288349127009862211E-17, -1.000000000000000000 ) ) ;
#7500 = EDGE_LOOP ( 'NONE', ( #26278, #14223, #12913, #14935 ) ) ;
#7501 = EDGE_LOOP ( 'NONE', ( #20597, #12957, #21382, #5061 ) ) ;
#7502 = CARTESIAN_POINT ( 'NONE',  ( 74.08334718032483579, -0.1676091211930581248, 13.78591818875846364 ) ) ;
#7503 = CIRCLE ( 'NONE', #21114, 12.36707279061065279 ) ;
#7504 = CARTESIAN_POINT ( 'NONE',  ( 45.32003422012917326, 11.18949478403750142, -4.624087122051892429 ) ) ;
#7505 = DIRECTION ( 'NONE',  ( -1.101824276508909887E-16, 1.000000000000000000, -0.000000000000000000 ) ) ;
#7506 = CARTESIAN_POINT ( 'NONE',  ( 8.474859994195282908, 38.56284415653841791, 47.04930799450051637 ) ) ;
#7507 = AXIS2_PLACEMENT_3D ( 'NONE', #3254, #30835, #8344 ) ;
#7508 = DIRECTION ( 'NONE',  ( -1.000000000000000000, 0.000000000000000000, 0.000000000000000000 ) ) ;
#7509 = EDGE_LOOP ( 'NONE', ( #29783, #23717, #16279, #30594 ) ) ;
#7510 = CARTESIAN_POINT ( 'NONE',  ( 21.09785597605720753, 14.86454579224779948, 47.04930799450052348 ) ) ;
#7511 = EDGE_LOOP ( 'NONE', ( #14350, #16464, #523, #30144 ) ) ;
#7512 = CARTESIAN_POINT ( 'NONE',  ( -31.41155082672278454, 3.821193253715539750, 15.70784009975334250 ) ) ;
#7513 = CARTESIAN_POINT ( 'NONE',  ( 80.71684048725118998, -5.935454207752202116, 16.07118271501079221 ) ) ;
#7514 = ORIENTED_EDGE ( 'NONE', *, *, #21691, .F. ) ;
#7515 = DIRECTION ( 'NONE',  ( -0.9612616959383206705, -0.2756373558169931681, 1.660411357259282445E-16 ) ) ;
#7516 = CARTESIAN_POINT ( 'NONE',  ( 8.698509210239517842, 25.34164230456639899, 47.04930799450051637 ) ) ;
#7517 = PLANE ( 'NONE',  #606 ) ;
#7518 = CARTESIAN_POINT ( 'NONE',  ( -40.11286833322907341, 2.887657226147505973, 38.24930799450051921 ) ) ;
#7519 = CARTESIAN_POINT ( 'NONE',  ( 46.99023568444673060, 28.53791119454914949, 49.12151524109405898 ) ) ;
#7520 = CIRCLE ( 'NONE', #15895, 0.6000000000000033085 ) ;
#7521 = AXIS2_PLACEMENT_3D ( 'NONE', #6378, #5904, #6213 ) ;
#7522 = FACE_OUTER_BOUND ( 'NONE', #14012, .T. ) ;
#7523 = DIRECTION ( 'NONE',  ( -1.101824276508909887E-16, 1.000000000000000000, -0.000000000000000000 ) ) ;
#7524 = ORIENTED_EDGE ( 'NONE', *, *, #5815, .F. ) ;
#7525 = CYLINDRICAL_SURFACE ( 'NONE', #16085, 37.00000000000000711 ) ;
#7526 = DIRECTION ( 'NONE',  ( -0.4544104659272780733, 0.000000000000000000, -0.8907924160295450644 ) ) ;
#7527 = ORIENTED_EDGE ( 'NONE', *, *, #49, .T. ) ;
#7528 = DIRECTION ( 'NONE',  ( -0.9612616959383183390, -0.2756373558170014948, -8.795445018805493151E-19 ) ) ;
#7529 = EDGE_LOOP ( 'NONE', ( #14736, #11136, #3751, #6824 ) ) ;
#7530 = EDGE_LOOP ( 'NONE', ( #10527, #10428, #20939, #19662 ) ) ;
#7531 = CARTESIAN_POINT ( 'NONE',  ( 21.09785597605719332, 30.56554579224779644, 73.04930799450052348 ) ) ;
#7532 = EDGE_LOOP ( 'NONE', ( #5620, #17803, #6252, #17625 ) ) ;
#7533 = AXIS2_PLACEMENT_3D ( 'NONE', #7021, #32303, #9977 ) ;
#7534 = CONICAL_SURFACE ( 'NONE', #4310, 11.79999999999997762, 0.7853981633974786991 ) ;
#7535 = ADVANCED_FACE ( 'NONE', ( #25771 ), #3285, .T. ) ;
#7536 = AXIS2_PLACEMENT_3D ( 'NONE', #28782, #21707, #6624 ) ;
#7537 = EDGE_CURVE ( 'NONE', #3694, #29832, #22983, .T. ) ;
#7538 = EDGE_CURVE ( 'NONE', #29304, #1340, #25298, .T. ) ;
#7539 = EDGE_CURVE ( 'NONE', #4111, #2645, #19750, .T. ) ;
#7540 = AXIS2_PLACEMENT_3D ( 'NONE', #27539, #5385, #24917 ) ;
#7541 = ORIENTED_EDGE ( 'NONE', *, *, #17454, .T. ) ;
#7542 = ADVANCED_FACE ( 'NONE', ( #8379 ), #15556, .T. ) ;
#7543 = ADVANCED_FACE ( 'NONE', ( #17904 ), #2978, .T. ) ;
#7544 = CARTESIAN_POINT ( 'NONE',  ( 45.78383729499237376, 22.98765316579147111, 47.71961428948426231 ) ) ;
#7545 = ORIENTED_EDGE ( 'NONE', *, *, #5611, .T. ) ;
#7546 = FACE_OUTER_BOUND ( 'NONE', #13275, .T. ) ;
#7547 = DIRECTION ( 'NONE',  ( -0.000000000000000000, -1.000000000000000000, 0.000000000000000000 ) ) ;
#7548 = CARTESIAN_POINT ( 'NONE',  ( -9.949682596861894268, -5.936967987714537820, -13.32519756455022808 ) ) ;
#7549 = CARTESIAN_POINT ( 'NONE',  ( 48.40186567930498285, 25.32957786121582089, 45.03923535223908203 ) ) ;
#7550 = ORIENTED_EDGE ( 'NONE', *, *, #550, .T. ) ;
#7551 = VERTEX_POINT ( 'NONE', #2805 ) ;
#7552 = DIRECTION ( 'NONE',  ( 0.4544104193609903586, 0.000000000000000000, 0.8907924397839087627 ) ) ;
#7553 = ORIENTED_EDGE ( 'NONE', *, *, #31181, .F. ) ;
#7554 = FACE_OUTER_BOUND ( 'NONE', #15412, .T. ) ;
#7555 = CARTESIAN_POINT ( 'NONE',  ( 21.09992658989239089, 26.96183152705960495, 47.04930799450051637 ) ) ;
#7556 = CARTESIAN_POINT ( 'NONE',  ( -38.34904439134557919, 6.997879252028663011, 61.94930799450052206 ) ) ;
#7557 = CARTESIAN_POINT ( 'NONE',  ( 21.09992658989238734, 32.54735957529758394, 47.04930799450051637 ) ) ;
#7558 = ORIENTED_EDGE ( 'NONE', *, *, #19334, .F. ) ;
#7559 = ORIENTED_EDGE ( 'NONE', *, *, #29391, .F. ) ;
#7560 = CARTESIAN_POINT ( 'NONE',  ( 8.698509210239549816, 28.34164230456639544, 47.04930799450051637 ) ) ;
#7561 = DIRECTION ( 'NONE',  ( -1.101824276508909887E-16, 1.000000000000000000, -0.000000000000000000 ) ) ;
#7562 = AXIS2_PLACEMENT_3D ( 'NONE', #1092, #5874, #28516 ) ;
#7563 = DIRECTION ( 'NONE',  ( 5.937205496305277864E-17, -0.8746197071393925215, 0.4848096202463429982 ) ) ;
#7564 = ORIENTED_EDGE ( 'NONE', *, *, #5127, .F. ) ;
#7565 = CARTESIAN_POINT ( 'NONE',  ( 52.07598125554711999, -5.935454207752202116, 107.5832303370038403 ) ) ;
#7566 = VERTEX_POINT ( 'NONE', #10202 ) ;
#7567 = DIRECTION ( 'NONE',  ( -1.101824276508909887E-16, 1.000000000000000000, -0.000000000000000000 ) ) ;
#7568 = DIRECTION ( 'NONE',  ( 0.4544104193609905806, 5.611869858668446909E-17, 0.8907924397839086517 ) ) ;
#7569 = EDGE_CURVE ( 'NONE', #10653, #22393, #21310, .T. ) ;
#7570 = CARTESIAN_POINT ( 'NONE',  ( -39.67555847965937943, 2.645252416024337361, 48.94930799450051495 ) ) ;
#7571 = ORIENTED_EDGE ( 'NONE', *, *, #22901, .T. ) ;
#7572 = TOROIDAL_SURFACE ( 'NONE', #22785, 12.61792373059893713, 0.1249999999999992506 ) ;
#7573 = EDGE_CURVE ( 'NONE', #14294, #30985, #18400, .T. ) ;
#7574 = VERTEX_POINT ( 'NONE', #15440 ) ;
#7575 = CONICAL_SURFACE ( 'NONE', #30122, 54.50502525316942126, 0.7853981633974552734 ) ;
#7576 = EDGE_CURVE ( 'NONE', #2178, #27701, #23373, .T. ) ;
#7577 = CARTESIAN_POINT ( 'NONE',  ( 21.09785597605719332, 40.56454579224779877, 47.04930799450051637 ) ) ;
#7578 = CARTESIAN_POINT ( 'NONE',  ( 21.09992658989239089, 24.96664230456639899, 47.04930799450051637 ) ) ;
#7580 = CARTESIAN_POINT ( 'NONE',  ( 48.18662509608405031, 27.28284706826093142, 49.18364984542562013 ) ) ;
#7579 = CIRCLE ( 'NONE', #27495, 0.1000000000000004774 ) ;
#7581 = AXIS2_PLACEMENT_3D ( 'NONE', #1141, #11171, #8542 ) ;
#7582 = ORIENTED_EDGE ( 'NONE', *, *, #12172, .T. ) ;
#7583 = CARTESIAN_POINT ( 'NONE',  ( -29.27613032885505007, -5.472247659560185440, 79.55937378679692529 ) ) ;
#7584 = DIRECTION ( 'NONE',  ( -1.101824276508909887E-16, 1.000000000000000000, -0.000000000000000000 ) ) ;
#7585 = DIRECTION ( 'NONE',  ( -0.2530443915477366690, 0.8824706660164322036, 0.3965022818682769623 ) ) ;
#7586 = DIRECTION ( 'NONE',  ( -1.101824276508909887E-16, 1.000000000000000000, -0.000000000000000000 ) ) ;
#7587 = CARTESIAN_POINT ( 'NONE',  ( 45.52675994804781112, 27.53420399681022346, 49.47108226228596806 ) ) ;
#7588 = DIRECTION ( 'NONE',  ( -1.101824276508909887E-16, 1.000000000000000000, -0.000000000000000000 ) ) ;
#7589 = DIRECTION ( 'NONE',  ( 0.4151817967359235362, -0.9097384655268405673, 0.000000000000000000 ) ) ;
#7590 = DIRECTION ( 'NONE',  ( -0.3879443550132459229, -0.6998701428318346851, 0.5997340748914504749 ) ) ;
#7591 = DIRECTION ( 'NONE',  ( -0.000000000000000000, -1.000000000000000000, -0.000000000000000000 ) ) ;
#7592 = CARTESIAN_POINT ( 'NONE',  ( 41.78468839005763158, 11.92558985988973497, 98.93617424376159875 ) ) ;
#7593 = FILL_AREA_STYLE_COLOUR ( '', #21036 ) ;
#7594 =( NAMED_UNIT ( * ) PLANE_ANGLE_UNIT ( ) SI_UNIT ( $, .RADIAN. ) );
#7595 = VERTEX_POINT ( 'NONE', #12991 ) ;
#7596 = ORIENTED_EDGE ( 'NONE', *, *, #8345, .T. ) ;
#7597 = LINE ( 'NONE', #2342, #3964 ) ;
#7598 = DIRECTION ( 'NONE',  ( -1.000000000000000000, -1.101824276508909887E-16, 0.000000000000000000 ) ) ;
#7599 = EDGE_CURVE ( 'NONE', #11226, #25945, #10288, .T. ) ;
#7600 = CARTESIAN_POINT ( 'NONE',  ( 54.81484111678624771, -3.025068871688596062, 101.6183422021972689 ) ) ;
#7601 = AXIS2_PLACEMENT_3D ( 'NONE', #24283, #19348, #19836 ) ;
#7602 = ORIENTED_EDGE ( 'NONE', *, *, #26202, .F. ) ;
#7603 = CARTESIAN_POINT ( 'NONE',  ( -43.64073206722599707, 1.267352857069778960, 34.54930799450052348 ) ) ;
#7604 = CARTESIAN_POINT ( 'NONE',  ( 21.09992658989239089, 23.59164230456639544, 47.04930799450051637 ) ) ;
#7605 = DIRECTION ( 'NONE',  ( -0.8746197071393955191, 0.4848096202463378357, 8.676864087101651105E-18 ) ) ;
#7606 = VERTEX_POINT ( 'NONE', #5595 ) ;
#7607 = EDGE_LOOP ( 'NONE', ( #15072, #15613, #17684, #15117 ) ) ;
#7609 = AXIS2_PLACEMENT_3D ( 'NONE', #2492, #17257, #10055 ) ;
#7608 = DIRECTION ( 'NONE',  ( 0.000000000000000000, 0.000000000000000000, -1.000000000000000000 ) ) ;
#7610 = CARTESIAN_POINT ( 'NONE',  ( 48.94625023931840957, 26.75784706826093284, 46.10640627770150246 ) ) ;
#7611 = EDGE_CURVE ( 'NONE', #4901, #11910, #18619, .T. ) ;
#7612 = CIRCLE ( 'NONE', #27513, 55.85791022362053582 ) ;
#7613 = EDGE_CURVE ( 'NONE', #26283, #17205, #6081, .T. ) ;
#7614 = AXIS2_PLACEMENT_3D ( 'NONE', #10300, #30318, #22101 ) ;
#7615 = CARTESIAN_POINT ( 'NONE',  ( -42.22138300640813924, 14.68176690255378603, 36.00717268343339583 ) ) ;
#7616 = DIRECTION ( 'NONE',  ( 1.000000000000000000, 0.000000000000000000, 0.000000000000000000 ) ) ;
#7617 = AXIS2_PLACEMENT_3D ( 'NONE', #25928, #15923, #28243 ) ;
#7618 = CARTESIAN_POINT ( 'NONE',  ( 8.698509210239580014, 31.59164230456639544, 47.04930799450051637 ) ) ;
#7619 = VERTEX_POINT ( 'NONE', #20684 ) ;
#7620 = ADVANCED_FACE ( 'NONE', ( #8222 ), #16037, .T. ) ;
#7621 = CARTESIAN_POINT ( 'NONE',  ( -40.65120636623950645, 8.087130829066872195, 57.04930799450051637 ) ) ;
#7622 = VERTEX_POINT ( 'NONE', #13475 ) ;
#7623 = AXIS2_PLACEMENT_3D ( 'NONE', #8815, #21122, #24073 ) ;
#7624 = CARTESIAN_POINT ( 'NONE',  ( 21.09992658989239089, 27.34164230456639544, 47.04930799450051637 ) ) ;
#7625 = CARTESIAN_POINT ( 'NONE',  ( 33.71785032049130137, 31.96664230456639544, 47.04930799450051637 ) ) ;
#7626 = CIRCLE ( 'NONE', #24386, 12.36707279061065101 ) ;
#7627 = AXIS2_PLACEMENT_3D ( 'NONE', #14212, #22227, #12236 ) ;
#7628 = AXIS2_PLACEMENT_3D ( 'NONE', #19760, #2383, #7475 ) ;
#7629 = ORIENTED_EDGE ( 'NONE', *, *, #30104, .F. ) ;
#7630 = DIRECTION ( 'NONE',  ( -1.101824276508909887E-16, 1.000000000000000000, -0.000000000000000000 ) ) ;
#7631 = ORIENTED_EDGE ( 'NONE', *, *, #10771, .F. ) ;
#7632 = TOROIDAL_SURFACE ( 'NONE', #30178, 12.40141737965283220, 0.1250000000000002498 ) ;
#7633 = CARTESIAN_POINT ( 'NONE',  ( 8.474859994195286461, 26.34143805560860940, 47.04930799450051637 ) ) ;
#7634 = CARTESIAN_POINT ( 'NONE',  ( 8.732853799281738105, 29.46183152705961206, 47.04930799450051637 ) ) ;
#7635 = ADVANCED_FACE ( 'NONE', ( #1630 ), #31349, .T. ) ;
#7636 = CARTESIAN_POINT ( 'NONE',  ( -40.11286833322907341, 2.887657226147507306, 38.34930799450052064 ) ) ;
#7637 = CYLINDRICAL_SURFACE ( 'NONE', #31195, 12.62506659569710266 ) ;
#7638 = ORIENTED_EDGE ( 'NONE', *, *, #8851, .T. ) ;
#7639 = CARTESIAN_POINT ( 'NONE',  ( 71.55165960851208240, 9.421471677506302100, 74.09761384657856809 ) ) ;
#7640 = DIRECTION ( 'NONE',  ( -1.000000000000000000, -1.101824276508909887E-16, 0.000000000000000000 ) ) ;
#7641 = CARTESIAN_POINT ( 'NONE',  ( 81.70930933238793159, -5.935454207752202116, 77.87546120947918382 ) ) ;
#7642 = ADVANCED_FACE ( 'NONE', ( #8857 ), #314, .T. ) ;
#7643 = CARTESIAN_POINT ( 'NONE',  ( -40.82323252358241206, 8.354654602666819585, 40.36793714460204541 ) ) ;
#7644 = LINE ( 'NONE', #14538, #17346 ) ;
#7645 = ORIENTED_EDGE ( 'NONE', *, *, #7689, .F. ) ;
#7646 = DIRECTION ( 'NONE',  ( 0.000000000000000000, 0.000000000000000000, -1.000000000000000000 ) ) ;
#7647 = DIRECTION ( 'NONE',  ( -0.9612616959383194493, -0.2756373558169972759, -8.795445018804907668E-19 ) ) ;
#7648 = ORIENTED_EDGE ( 'NONE', *, *, #4793, .F. ) ;
#7649 = DIRECTION ( 'NONE',  ( 0.000000000000000000, 0.000000000000000000, 1.000000000000000000 ) ) ;
#7650 = EDGE_CURVE ( 'NONE', #30366, #2286, #24947, .T. ) ;
#7651 = EDGE_CURVE ( 'NONE', #11226, #26412, #31192, .T. ) ;
#7652 = CARTESIAN_POINT ( 'NONE',  ( 21.09785597605719332, 44.99492099041257376, 24.40795046456371153 ) ) ;
#7653 = ADVANCED_FACE ( 'NONE', ( #28565 ), #16240, .T. ) ;
#7654 = ORIENTED_EDGE ( 'NONE', *, *, #16232, .T. ) ;
#7655 = DIRECTION ( 'NONE',  ( -1.000000000000000000, 0.000000000000000000, 0.000000000000000000 ) ) ;
#7656 = ORIENTED_EDGE ( 'NONE', *, *, #3963, .T. ) ;
#7657 = AXIS2_PLACEMENT_3D ( 'NONE', #9735, #19726, #17595 ) ;
#7658 = EDGE_LOOP ( 'NONE', ( #17763, #13388, #21879, #16474 ) ) ;
#7659 = CIRCLE ( 'NONE', #24437, 12.36707279061065101 ) ;
#7660 = DIRECTION ( 'NONE',  ( 0.000000000000000000, 0.000000000000000000, -1.000000000000000000 ) ) ;
#7661 = CARTESIAN_POINT ( 'NONE',  ( 45.36511207810798396, 25.80948166895303686, 45.12672418911604666 ) ) ;
#7662 = ORIENTED_EDGE ( 'NONE', *, *, #29534, .T. ) ;
#7663 = EDGE_LOOP ( 'NONE', ( #8070, #6157, #1720, #23909 ) ) ;
#7664 = CARTESIAN_POINT ( 'NONE',  ( 77.20159755473073915, -4.768257113790719259, 14.00407067606322897 ) ) ;
#7665 = CARTESIAN_POINT ( 'NONE',  ( -43.80906883710621713, -4.771375425951670302, 52.22812131641889977 ) ) ;
#7666 = CARTESIAN_POINT ( 'NONE',  ( -40.22018024869838371, 7.672350704644241404, 60.22001867261916885 ) ) ;
#7667 = FACE_OUTER_BOUND ( 'NONE', #31896, .T. ) ;
#7668 = EDGE_CURVE ( 'NONE', #25453, #25964, #25988, .T. ) ;
#7669 = CYLINDRICAL_SURFACE ( 'NONE', #25739, 13.00000000000000533 ) ;
#7670 = ORIENTED_EDGE ( 'NONE', *, *, #14719, .F. ) ;
#7671 = DIRECTION ( 'NONE',  ( -0.000000000000000000, -1.000000000000000000, 0.000000000000000000 ) ) ;
#7672 = ORIENTED_EDGE ( 'NONE', *, *, #3249, .F. ) ;
#7673 = CARTESIAN_POINT ( 'NONE',  ( -31.70662748216360782, 2.874681785498175657, 15.18106132554749621 ) ) ;
#7675 = CARTESIAN_POINT ( 'NONE',  ( 8.698509210239539158, 27.34164230456639544, 47.04930799450051637 ) ) ;
#7674 = CIRCLE ( 'NONE', #18654, 0.1000000000000006301 ) ;
#7676 = PRESENTATION_LAYER_ASSIGNMENT (  '', '', ( #11858 ) ) ;
#7677 = VERTEX_POINT ( 'NONE', #16079 ) ;
#7678 = LINE ( 'NONE', #13092, #4289 ) ;
#7679 = DIRECTION ( 'NONE',  ( 1.000000000000000000, 0.000000000000000000, 0.000000000000000000 ) ) ;
#7680 = EDGE_CURVE ( 'NONE', #25242, #28129, #30198, .T. ) ;
#7681 = FACE_OUTER_BOUND ( 'NONE', #30454, .T. ) ;
#7682 = CARTESIAN_POINT ( 'NONE',  ( 8.474859994195281132, 31.34143805560860585, 47.04930799450051637 ) ) ;
#7683 = CARTESIAN_POINT ( 'NONE',  ( 46.99747725352182925, 22.88065857334294861, 48.98207832244369087 ) ) ;
#7684 = CARTESIAN_POINT ( 'NONE',  ( 46.00908685603034343, 29.64624452788248021, 44.91496614357595263 ) ) ;
#7685 = CARTESIAN_POINT ( 'NONE',  ( 21.09992658989239089, 24.34184655352419213, 47.04930799450051637 ) ) ;
#7686 = ORIENTED_EDGE ( 'NONE', *, *, #7233, .T. ) ;
#7687 = FACE_OUTER_BOUND ( 'NONE', #2985, .T. ) ;
#7688 = ORIENTED_EDGE ( 'NONE', *, *, #21881, .T. ) ;
#7689 = EDGE_CURVE ( 'NONE', #13790, #1027, #16400, .T. ) ;
#7690 = TOROIDAL_SURFACE ( 'NONE', #7133, 46.75000000000000000, 0.7905694150421007649 ) ;
#7691 = CARTESIAN_POINT ( 'NONE',  ( 21.09785597605719332, -15.93545420775219945, 126.2593585008393831 ) ) ;
#7692 = ORIENTED_EDGE ( 'NONE', *, *, #11761, .F. ) ;
#7693 = EDGE_LOOP ( 'NONE', ( #1700, #1637, #21075, #9308 ) ) ;
#7694 = CARTESIAN_POINT ( 'NONE',  ( -40.11286833322907341, 2.887657226147507306, 35.14930799450051779 ) ) ;
#7695 = ORIENTED_EDGE ( 'NONE', *, *, #30631, .T. ) ;
#7696 = CIRCLE ( 'NONE', #5586, 12.62506659569710266 ) ;
#7697 = ORIENTED_EDGE ( 'NONE', *, *, #24913, .F. ) ;
#7698 = CARTESIAN_POINT ( 'NONE',  ( 47.09785597605719687, 23.12036939723557083, 47.04930799450080059 ) ) ;
#7699 = CIRCLE ( 'NONE', #27063, 0.1250000000000001110 ) ;
#7700 = VERTEX_POINT ( 'NONE', #18690 ) ;
#7701 = LINE ( 'NONE', #20317, #20372 ) ;
#7702 = CARTESIAN_POINT ( 'NONE',  ( 49.59034552300744281, 29.16454579224780019, 47.24294646780535345 ) ) ;
#7703 = DIRECTION ( 'NONE',  ( 0.000000000000000000, 0.000000000000000000, -1.000000000000000000 ) ) ;
#7704 = CARTESIAN_POINT ( 'NONE',  ( 46.00908685603034343, 26.14624452788249087, 44.91496614357595263 ) ) ;
#7705 = ORIENTED_EDGE ( 'NONE', *, *, #12356, .T. ) ;
#7706 = ORIENTED_EDGE ( 'NONE', *, *, #6439, .T. ) ;
#7707 = DIRECTION ( 'NONE',  ( 0.000000000000000000, 0.000000000000000000, -1.000000000000000000 ) ) ;
#7708 = ORIENTED_EDGE ( 'NONE', *, *, #8413, .T. ) ;
#7709 = DIRECTION ( 'NONE',  ( -1.000000000000000000, 0.000000000000000000, 0.000000000000000000 ) ) ;
#7710 = CARTESIAN_POINT ( 'NONE',  ( 47.09785597605719687, 23.12036939723557083, 47.04930799450080059 ) ) ;
#7711 = CARTESIAN_POINT ( 'NONE',  ( -40.69230700880733309, 6.792718999258627655, 34.69881571428543765 ) ) ;
#7712 = DIRECTION ( 'NONE',  ( -1.000000000000000000, 0.000000000000000000, 0.000000000000000000 ) ) ;
#7713 = DIRECTION ( 'NONE',  ( 1.000000000000000000, 0.000000000000000000, 0.000000000000000000 ) ) ;
#7714 = PRODUCT_CONTEXT ( 'NONE', #8664, 'mechanical' ) ;
#7715 = ORIENTED_EDGE ( 'NONE', *, *, #7258, .F. ) ;
#7716 = ORIENTED_EDGE ( 'NONE', *, *, #6713, .F. ) ;
#7717 = DIRECTION ( 'NONE',  ( 0.000000000000000000, 1.000000000000000000, 0.000000000000000000 ) ) ;
#7718 = CIRCLE ( 'NONE', #26046, 12.73401709983438401 ) ;
#7719 = DIRECTION ( 'NONE',  ( -1.000000000000000000, 0.000000000000000000, 0.000000000000000000 ) ) ;
#7720 = ADVANCED_FACE ( 'NONE', ( #26088, #3768 ), #11479, .F. ) ;
#7721 = EDGE_CURVE ( 'NONE', #30017, #16381, #4493, .T. ) ;
#7722 = DIRECTION ( 'NONE',  ( -0.000000000000000000, -1.000000000000000000, 0.000000000000000000 ) ) ;
#7723 = EDGE_CURVE ( 'NONE', #29858, #15854, #14476, .T. ) ;
#7724 = ORIENTED_EDGE ( 'NONE', *, *, #23018, .F. ) ;
#7725 = CARTESIAN_POINT ( 'NONE',  ( 52.08014736722963534, -5.935653941159263702, 107.5318010694234374 ) ) ;
#7726 = ORIENTED_EDGE ( 'NONE', *, *, #1538, .T. ) ;
#7727 = DIRECTION ( 'NONE',  ( -0.000000000000000000, -1.000000000000000000, 0.000000000000000000 ) ) ;
#7728 = CARTESIAN_POINT ( 'NONE',  ( 2.097855976057206195, 14.86454579224779948, 47.04930799450052348 ) ) ;
#7729 = FACE_OUTER_BOUND ( 'NONE', #17064, .T. ) ;
#7730 = ORIENTED_EDGE ( 'NONE', *, *, #24983, .F. ) ;
#7731 = VECTOR ( 'NONE', #25305, 1000.000000000000000 ) ;
#7732 = CIRCLE ( 'NONE', #3522, 1.000000000000000888 ) ;
#7733 = ORIENTED_EDGE ( 'NONE', *, *, #1016, .T. ) ;
#7734 = DIRECTION ( 'NONE',  ( 8.659560562354932858E-17, -0.7071067811865474617, 0.7071067811865474617 ) ) ;
#7735 = AXIS2_PLACEMENT_3D ( 'NONE', #23973, #7069, #17071 ) ;
#7736 = DIRECTION ( 'NONE',  ( -1.000000000000000000, -1.101824276508909887E-16, 0.000000000000000000 ) ) ;
#7737 = CARTESIAN_POINT ( 'NONE',  ( 48.18662509608405031, 26.58284706826093213, 49.18364984542562013 ) ) ;
#7738 = EDGE_LOOP ( 'NONE', ( #22970, #3313, #12139, #13491 ) ) ;
#7739 = CARTESIAN_POINT ( 'NONE',  ( -29.27613032885505007, -0.7885532610349046401, 80.71350123316483405 ) ) ;
#7740 = VECTOR ( 'NONE', #2012, 1000.000000000000000 ) ;
#7741 = CARTESIAN_POINT ( 'NONE',  ( 8.823509210239574685, 31.34164230456639544, 47.04930799450051637 ) ) ;
#7742 = DIRECTION ( 'NONE',  ( 1.000000000000000000, 0.000000000000000000, -1.224646799147353207E-16 ) ) ;
#7743 = CARTESIAN_POINT ( 'NONE',  ( 48.23388202445966044, 26.25087065737812253, 49.27628909396054979 ) ) ;
#7744 = FACE_BOUND ( 'NONE', #1449, .T. ) ;
#7745 = AXIS2_PLACEMENT_3D ( 'NONE', #7780, #17781, #22870 ) ;
#7746 = PLANE ( 'NONE',  #31704 ) ;
#7747 = DIRECTION ( 'NONE',  ( 0.2756373558169974980, -0.9612616959383193382, 9.694974607321218218E-33 ) ) ;
#7748 = DIRECTION ( 'NONE',  ( 0.6797146636928694807, 0.1949050434465297021, 0.7071067811865444641 ) ) ;
#7749 = FACE_OUTER_BOUND ( 'NONE', #2547, .T. ) ;
#7750 = DIRECTION ( 'NONE',  ( 0.000000000000000000, 0.000000000000000000, 1.000000000000000000 ) ) ;
#7751 = CARTESIAN_POINT ( 'NONE',  ( 44.77625694075214824, 29.51454579807170120, 48.23360063142255427 ) ) ;
#7752 = SURFACE_STYLE_USAGE ( .BOTH. , #10219 ) ;
#7753 = VERTEX_POINT ( 'NONE', #6562 ) ;
#7754 = ORIENTED_EDGE ( 'NONE', *, *, #18245, .F. ) ;
#7755 = DIRECTION ( 'NONE',  ( -1.224646799147353207E-16, -1.349345573449484691E-32, 1.000000000000000000 ) ) ;
#7756 = CARTESIAN_POINT ( 'NONE',  ( -36.90670693849242667, -5.935454207752202116, 16.07118271501078510 ) ) ;
#7757 = EDGE_CURVE ( 'NONE', #3066, #30310, #19015, .T. ) ;
#7758 = CARTESIAN_POINT ( 'NONE',  ( 21.09785597605719687, 24.56454579224780232, 7.349896848133565364 ) ) ;
#7759 = EDGE_CURVE ( 'NONE', #14556, #18455, #1142, .T. ) ;
#7760 = EDGE_CURVE ( 'NONE', #20587, #1157, #11326, .T. ) ;
#7761 = ORIENTED_EDGE ( 'NONE', *, *, #1138, .F. ) ;
#7762 = CARTESIAN_POINT ( 'NONE',  ( -39.46303006544686554, -5.935456067349330844, 77.98454154827626894 ) ) ;
#7763 = CARTESIAN_POINT ( 'NONE',  ( -4.402144023942796025, -5.098646251524523443, 47.04930799450052348 ) ) ;
#7764 = CARTESIAN_POINT ( 'NONE',  ( -43.90780810587784089, -0.03953120679776488122, 61.94930799450052206 ) ) ;
#7765 = VERTEX_POINT ( 'NONE', #3937 ) ;
#7766 = ORIENTED_EDGE ( 'NONE', *, *, #13580, .T. ) ;
#7767 = CARTESIAN_POINT ( 'NONE',  ( -10.40214402394279425, -5.098646251524523443, 47.04930799450052348 ) ) ;
#7768 = EDGE_CURVE ( 'NONE', #19572, #1158, #26576, .T. ) ;
#7769 = CARTESIAN_POINT ( 'NONE',  ( 48.18662509608405031, 25.88284706826093284, 49.18364984542562013 ) ) ;
#7770 = CARTESIAN_POINT ( 'NONE',  ( -5.602943079677954685, 9.702389020015065313, -12.62465409255485582 ) ) ;
#7771 = CIRCLE ( 'NONE', #26090, 0.1250000000000001110 ) ;
#7772 = DIRECTION ( 'NONE',  ( -0.000000000000000000, -1.000000000000000000, 0.000000000000000000 ) ) ;
#7773 = DIRECTION ( 'NONE',  ( -1.000000000000000000, 0.000000000000000000, 0.000000000000000000 ) ) ;
#7774 = TOROIDAL_SURFACE ( 'NONE', #4613, 29.50000000000000355, 1.500000000000001332 ) ;
#7775 = AXIS2_PLACEMENT_3D ( 'NONE', #20885, #28450, #25974 ) ;
#7776 = EDGE_LOOP ( 'NONE', ( #13833, #10102, #266, #341 ) ) ;
#7777 = DIRECTION ( 'NONE',  ( 0.4544104193609903586, 0.000000000000000000, 0.8907924397839087627 ) ) ;
#7778 = ORIENTED_EDGE ( 'NONE', *, *, #3227, .F. ) ;
#7779 = FACE_OUTER_BOUND ( 'NONE', #14924, .T. ) ;
#7780 = CARTESIAN_POINT ( 'NONE',  ( 21.09785597605720042, -13.87844638871996850, 47.04930799450051637 ) ) ;
#7781 = EDGE_CURVE ( 'NONE', #27701, #2178, #5556, .T. ) ;
#7782 = CIRCLE ( 'NONE', #26119, 12.36707279061065279 ) ;
#7783 = EDGE_CURVE ( 'NONE', #18205, #1215, #17201, .T. ) ;
#7784 = AXIS2_PLACEMENT_3D ( 'NONE', #25935, #29544, #14446 ) ;
#7785 = VECTOR ( 'NONE', #4288, 1000.000000000000000 ) ;
#7786 = ORIENTED_EDGE ( 'NONE', *, *, #16965, .T. ) ;
#7787 = CARTESIAN_POINT ( 'NONE',  ( -39.59300248568538194, 7.744584186742829779, 32.14930799450051779 ) ) ;
#7788 = ORIENTED_EDGE ( 'NONE', *, *, #4826, .T. ) ;
#7789 = TOROIDAL_SURFACE ( 'NONE', #19294, 12.40141737965281266, 0.1249999999999994865 ) ;
#7790 = CARTESIAN_POINT ( 'NONE',  ( 33.46699938050304013, 24.71183152705960140, 47.04930799450051637 ) ) ;
#7791 = DIRECTION ( 'NONE',  ( -1.000000000000000000, 0.000000000000000000, 0.000000000000000000 ) ) ;
#7792 = DIRECTION ( 'NONE',  ( 1.234978253042719660E-16, -1.000000000000000000, -1.109335647967047851E-31 ) ) ;
#7793 = EDGE_LOOP ( 'NONE', ( #22041, #4773, #15470, #31336 ) ) ;
#7794 = DIRECTION ( 'NONE',  ( 0.000000000000000000, 1.000000000000000000, -0.000000000000000000 ) ) ;
#7795 = DIRECTION ( 'NONE',  ( -1.101824276508909887E-16, 1.000000000000000000, -0.000000000000000000 ) ) ;
#7796 = CARTESIAN_POINT ( 'NONE',  ( 81.60546541303523327, -5.936248947737075454, 77.89911125597754449 ) ) ;
#7797 = DIRECTION ( 'NONE',  ( -0.000000000000000000, -1.000000000000000000, 0.000000000000000000 ) ) ;
#7798 = AXIS2_PLACEMENT_3D ( 'NONE', #3468, #15309, #2979 ) ;
#7799 = DIRECTION ( 'NONE',  ( -0.000000000000000000, -1.000000000000000000, 0.000000000000000000 ) ) ;
#7800 = EDGE_LOOP ( 'NONE', ( #9294, #14881 ) ) ;
#7801 = DIRECTION ( 'NONE',  ( 0.000000000000000000, 1.000000000000000000, 0.000000000000000000 ) ) ;
#7802 = CARTESIAN_POINT ( 'NONE',  ( 8.482002859293395147, 23.96664230456639899, 47.04930799450051637 ) ) ;
#7803 = ORIENTED_EDGE ( 'NONE', *, *, #583, .F. ) ;
#7804 = DIRECTION ( 'NONE',  ( -1.000000000000000000, 0.000000000000000000, 0.000000000000000000 ) ) ;
#7805 = EDGE_CURVE ( 'NONE', #14564, #15480, #5034, .T. ) ;
#7806 = CARTESIAN_POINT ( 'NONE',  ( 21.09992658989239089, 29.21183152705961206, 47.04930799450051637 ) ) ;
#7807 = DIRECTION ( 'NONE',  ( 0.000000000000000000, 0.000000000000000000, -1.000000000000000000 ) ) ;
#7808 = ORIENTED_EDGE ( 'NONE', *, *, #28579, .F. ) ;
#7809 = CARTESIAN_POINT ( 'NONE',  ( 21.09785597605719332, -16.43545420775217281, -37.95069200549950494 ) ) ;
#7810 = EDGE_LOOP ( 'NONE', ( #1497, #26885, #7199, #15683 ) ) ;
#7811 = AXIS2_PLACEMENT_3D ( 'NONE', #26579, #11484, #7207 ) ;
#7812 = AXIS2_PLACEMENT_3D ( 'NONE', #28158, #895, #30780 ) ;
#7813 = ORIENTED_EDGE ( 'NONE', *, *, #25850, .T. ) ;
#7814 = CONICAL_SURFACE ( 'NONE', #10413, 1.003191532947550701, 0.7853981633974447263 ) ;
#7815 = EDGE_CURVE ( 'NONE', #20995, #13496, #14596, .T. ) ;
#7816 = ADVANCED_FACE ( 'NONE', ( #2448 ), #15609, .F. ) ;
#7817 = CIRCLE ( 'NONE', #4669, 2.000000000000001776 ) ;
#7818 = CARTESIAN_POINT ( 'NONE',  ( -9.732691057006816138, -5.935709855254034828, 107.7169399001122230 ) ) ;
#7819 = CARTESIAN_POINT ( 'NONE',  ( 36.33160203359362583, 14.46497581658974063, 47.04930799450052348 ) ) ;
#7820 = EDGE_CURVE ( 'NONE', #19596, #25250, #18647, .T. ) ;
#7821 = EDGE_CURVE ( 'NONE', #2064, #13790, #23875, .T. ) ;
#7822 = VERTEX_POINT ( 'NONE', #12468 ) ;
#7823 = ORIENTED_EDGE ( 'NONE', *, *, #29046, .F. ) ;
#7824 = ADVANCED_FACE ( 'NONE', ( #7042 ), #26503, .T. ) ;
#7825 = CARTESIAN_POINT ( 'NONE',  ( 46.84924186968671478, 10.40182650318958224, -4.367473334732002499 ) ) ;
#7826 = CARTESIAN_POINT ( 'NONE',  ( 21.09785597605719332, 25.56454579224779877, 47.04930799450051637 ) ) ;
#7827 = CARTESIAN_POINT ( 'NONE',  ( -31.75494777190924367, 11.92558985988973319, 67.46350265493038023 ) ) ;
#7828 = DIRECTION ( 'NONE',  ( -0.000000000000000000, -1.000000000000000000, -0.000000000000000000 ) ) ;
#7829 = ORIENTED_EDGE ( 'NONE', *, *, #30550, .T. ) ;
#7830 = CARTESIAN_POINT ( 'NONE',  ( -9.728297238921268075, -5.935454207752198563, 105.1347781458764103 ) ) ;
#7831 = VERTEX_POINT ( 'NONE', #1794 ) ;
#7832 = CARTESIAN_POINT ( 'NONE',  ( -32.76246291686640433, -0.03437377967876181079, 13.81659845049603597 ) ) ;
#7833 = DIRECTION ( 'NONE',  ( -1.000000000000000000, 0.000000000000000000, 0.000000000000000000 ) ) ;
#7834 = AXIS2_PLACEMENT_3D ( 'NONE', #18466, #28494, #18142 ) ;
#7835 = VERTEX_POINT ( 'NONE', #10446 ) ;
#7836 = CARTESIAN_POINT ( 'NONE',  ( 46.84209603737756566, 23.10527845304106620, 46.54793520446708044 ) ) ;
#7837 = CIRCLE ( 'NONE', #24068, 12.36707279061065101 ) ;
#7838 = CARTESIAN_POINT ( 'NONE',  ( 81.66333222936422942, -5.936209625872264972, 15.95776322560501015 ) ) ;
#7839 = DIRECTION ( 'NONE',  ( 0.4848096202463636484, 0.8746197071393810862, 0.000000000000000000 ) ) ;
#7840 = DIRECTION ( 'NONE',  ( -1.101824276508909887E-16, 1.000000000000000000, -0.000000000000000000 ) ) ;
#7841 = CARTESIAN_POINT ( 'NONE',  ( 47.20547626766766314, 27.48791119454915233, 44.97710074790751378 ) ) ;
#7842 =( BOUNDED_CURVE ( )  B_SPLINE_CURVE ( 3, ( #27120, #14658, #26473, #21860 ),
 .UNSPECIFIED., .F., .F. ) 
 B_SPLINE_CURVE_WITH_KNOTS ( ( 4, 4 ),
 ( 4.712388980384679016, 4.772243325917784773 ),
 .UNSPECIFIED. ) 
 CURVE ( )  GEOMETRIC_REPRESENTATION_ITEM ( )  RATIONAL_B_SPLINE_CURVE ( ( 1.000000000000000000, 0.9997014770583808607, 0.9997014770583808607, 1.000000000000000000 ) ) 
 REPRESENTATION_ITEM ( '' )  );
#7843 = DIRECTION ( 'NONE',  ( -0.4848096202463371696, -0.8746197071393958522, 0.000000000000000000 ) ) ;
#7844 = DIRECTION ( 'NONE',  ( -1.000000000000000000, 0.000000000000000000, 0.000000000000000000 ) ) ;
#7845 = VERTEX_POINT ( 'NONE', #27220 ) ;
#7846 = EDGE_CURVE ( 'NONE', #6409, #23264, #3448, .T. ) ;
#7847 = DIRECTION ( 'NONE',  ( 1.234978253042719660E-16, -1.000000000000000000, -1.109335647967047851E-31 ) ) ;
#7848 = VERTEX_POINT ( 'NONE', #26908 ) ;
#7849 = CIRCLE ( 'NONE', #27779, 0.2999999999999947153 ) ;
#7850 = PLANE ( 'NONE',  #2213 ) ;
#7851 = ORIENTED_EDGE ( 'NONE', *, *, #2591, .F. ) ;
#7852 = CIRCLE ( 'NONE', #26171, 1.000000000000000888 ) ;
#7853 = ORIENTED_EDGE ( 'NONE', *, *, #20924, .T. ) ;
#7854 = FACE_OUTER_BOUND ( 'NONE', #6092, .T. ) ;
#7855 = ORIENTED_EDGE ( 'NONE', *, *, #31795, .T. ) ;
#7856 = EDGE_CURVE ( 'NONE', #893, #31932, #31229, .T. ) ;
#7857 = AXIS2_PLACEMENT_3D ( 'NONE', #23523, #555, #21048 ) ;
#7858 = AXIS2_PLACEMENT_3D ( 'NONE', #29893, #4118, #4606 ) ;
#7859 = EDGE_CURVE ( 'NONE', #22567, #11560, #16420, .T. ) ;
#7860 = VERTEX_POINT ( 'NONE', #19668 ) ;
#7861 = CARTESIAN_POINT ( 'NONE',  ( 46.35959775518843173, 23.04411657098542676, 47.91207660486297470 ) ) ;
#7862 = ADVANCED_FACE ( 'NONE', ( #29699 ), #25459, .T. ) ;
#7863 = AXIS2_PLACEMENT_3D ( 'NONE', #14505, #9084, #24498 ) ;
#7864 = AXIS2_PLACEMENT_3D ( 'NONE', #21001, #31674, #8858 ) ;
#7865 = ORIENTED_EDGE ( 'NONE', *, *, #7768, .F. ) ;
#7866 = ADVANCED_FACE ( 'NONE', ( #29863 ), #12380, .T. ) ;
#7867 =( NAMED_UNIT ( * ) SI_UNIT ( $, .STERADIAN. ) SOLID_ANGLE_UNIT ( ) );
#7868 = AXIS2_PLACEMENT_3D ( 'NONE', #21355, #26308, #11214 ) ;
#7869 = LINE ( 'NONE', #20653, #30674 ) ;
#7870 = CARTESIAN_POINT ( 'NONE',  ( 8.823509210239549816, 28.34164230456639544, 47.04930799450051637 ) ) ;
#7871 = CARTESIAN_POINT ( 'NONE',  ( 48.37829923888483563, 29.55122849631042570, 45.07556196625585443 ) ) ;
#7872 = CIRCLE ( 'NONE', #11536, 12.36707279061065101 ) ;
#7873 = VECTOR ( 'NONE', #250, 1000.000000000000227 ) ;
#7874 = VERTEX_POINT ( 'NONE', #13076 ) ;
#7875 = ORIENTED_EDGE ( 'NONE', *, *, #9157, .T. ) ;
#7876 = FACE_OUTER_BOUND ( 'NONE', #7482, .T. ) ;
#7877 = ORIENTED_EDGE ( 'NONE', *, *, #407, .F. ) ;
#7878 = CARTESIAN_POINT ( 'NONE',  ( -43.73393778030726509, 1.305471833569777695, 53.64930799450051779 ) ) ;
#7879 = DIRECTION ( 'NONE',  ( -1.101824276508909887E-16, 1.000000000000000000, -0.000000000000000000 ) ) ;
#7880 = LINE ( 'NONE', #2620, #12748 ) ;
#7881 = LINE ( 'NONE', #20332, #29397 ) ;
#7882 = DIRECTION ( 'NONE',  ( -1.101824276508909887E-16, 1.000000000000000000, -0.000000000000000000 ) ) ;
#7883 = APPLICATION_PROTOCOL_DEFINITION ( 'draft international standard', 'automotive_design', 1998, #22499 ) ;
#7884 = ORIENTED_EDGE ( 'NONE', *, *, #24255, .T. ) ;
#7885 = DIRECTION ( 'NONE',  ( 0.000000000000000000, 1.000000000000000000, 0.000000000000000000 ) ) ;
#7886 = AXIS2_PLACEMENT_3D ( 'NONE', #1190, #13842, #11370 ) ;
#7887 = CARTESIAN_POINT ( 'NONE',  ( 45.96182992765472619, 28.70087065737811827, 44.82232689504103007 ) ) ;
#7888 = FACE_OUTER_BOUND ( 'NONE', #30860, .T. ) ;
#7889 = CARTESIAN_POINT ( 'NONE',  ( 48.40186567930497574, 27.51618040159426570, 45.03923535223907493 ) ) ;
#7890 = EDGE_LOOP ( 'NONE', ( #19502, #2252, #30965, #22226 ) ) ;
#7891 = DIRECTION ( 'NONE',  ( -1.000000000000000000, 0.000000000000000000, 0.000000000000000000 ) ) ;
#7892 = CARTESIAN_POINT ( 'NONE',  ( 21.09785597605719332, -8.535454207752287914, -20.95069200549947652 ) ) ;
#7893 = AXIS2_PLACEMENT_3D ( 'NONE', #8200, #28218, #16056 ) ;
#7894 = AXIS2_PLACEMENT_3D ( 'NONE', #23473, #10361, #8544 ) ;
#7895 = CARTESIAN_POINT ( 'NONE',  ( -31.36119014644065572, 11.88414354777924942, 25.57570259114776690 ) ) ;
#7896 = VECTOR ( 'NONE', #17711, 1000.000000000000114 ) ;
#7897 = AXIS2_PLACEMENT_3D ( 'NONE', #6600, #28597, #6437 ) ;
#7898 = AXIS2_PLACEMENT_3D ( 'NONE', #25163, #17769, #27788 ) ;
#7899 = CIRCLE ( 'NONE', #20998, 21.49999999999999645 ) ;
#7900 = VERTEX_POINT ( 'NONE', #30633 ) ;
#7901 = ORIENTED_EDGE ( 'NONE', *, *, #1927, .F. ) ;
#7902 = FACE_OUTER_BOUND ( 'NONE', #18385, .T. ) ;
#7903 = DIRECTION ( 'NONE',  ( 0.000000000000000000, -0.7880107536067239016, -0.6156614753256557382 ) ) ;
#7904 = CARTESIAN_POINT ( 'NONE',  ( 21.09992658989239089, 27.59143805560860940, 47.04930799450051637 ) ) ;
#7905 = EDGE_CURVE ( 'NONE', #3283, #7173, #31270, .T. ) ;
#7906 = EDGE_LOOP ( 'NONE', ( #30339, #18008, #15921, #16017 ) ) ;
#7907 = ADVANCED_FACE ( 'NONE', ( #5676 ), #11245, .T. ) ;
#7908 = ADVANCED_FACE ( 'NONE', ( #13243 ), #28639, .F. ) ;
#7909 = LINE ( 'NONE', #30557, #27702 ) ;
#7910 = CARTESIAN_POINT ( 'NONE',  ( -40.65487266620045403, 9.475231293617264683, 39.43717596014455040 ) ) ;
#7911 = CARTESIAN_POINT ( 'NONE',  ( 33.37634396954524618, 26.84164230456639899, 47.04930799450051637 ) ) ;
#7912 = CARTESIAN_POINT ( 'NONE',  ( 45.36511207810798396, 25.93213139976340997, 45.12672418911605376 ) ) ;
#7913 = AXIS2_PLACEMENT_3D ( 'NONE', #26027, #6497, #1236 ) ;
#7914 = CARTESIAN_POINT ( 'NONE',  ( -41.96544240928614755, 13.75880317176705603, 59.54930799450050927 ) ) ;
#7915 = DIRECTION ( 'NONE',  ( -2.779292025043186357E-18, 1.288349127009862211E-17, -1.000000000000000000 ) ) ;
#7916 = DIRECTION ( 'NONE',  ( 0.000000000000000000, 0.000000000000000000, -1.000000000000000000 ) ) ;
#7917 = CARTESIAN_POINT ( 'NONE',  ( 45.13079246587579973, 22.86454579224779948, 47.59453030015130537 ) ) ;
#7918 = AXIS2_PLACEMENT_3D ( 'NONE', #22275, #32305, #9815 ) ;
#7919 = AXIS2_PLACEMENT_3D ( 'NONE', #18067, #30076, #676 ) ;
#7920 = DIRECTION ( 'NONE',  ( 0.4848096202463430537, 0.8746197071393926326, -1.125439520643636483E-16 ) ) ;
#7921 = CARTESIAN_POINT ( 'NONE',  ( 47.23302798462060537, 29.28121246473837047, 44.44659793406428605 ) ) ;
#7922 = CIRCLE ( 'NONE', #11594, 1.500000000000001332 ) ;
#7923 = ORIENTED_EDGE ( 'NONE', *, *, #24392, .F. ) ;
#7924 = ORIENTED_EDGE ( 'NONE', *, *, #6901, .T. ) ;
#7925 = DIRECTION ( 'NONE',  ( -1.101824276508909887E-16, 1.000000000000000000, -0.000000000000000000 ) ) ;
#7926 = AXIS2_PLACEMENT_3D ( 'NONE', #17140, #9611, #7146 ) ;
#7927 = CARTESIAN_POINT ( 'NONE',  ( 49.40052002316441104, 24.99301497605546629, 45.93418205075561644 ) ) ;
#7928 = CARTESIAN_POINT ( 'NONE',  ( -31.11772464322190856, 1.828802932772627399, 14.64222532548598465 ) ) ;
#7929 = CARTESIAN_POINT ( 'NONE',  ( 54.36124578179943967, -0.1676091211930509361, 100.0347991987680984 ) ) ;
#7930 = ORIENTED_EDGE ( 'NONE', *, *, #15431, .T. ) ;
#7931 = CARTESIAN_POINT ( 'NONE',  ( 21.09785597605720753, 13.86454579224779948, 47.04930799450052348 ) ) ;
#7932 = CARTESIAN_POINT ( 'NONE',  ( 47.66856441440319969, 23.10527865767145528, 46.91233790229156853 ) ) ;
#7933 = DIRECTION ( 'NONE',  ( 0.8746197071393926326, -0.4848096202463430537, -8.676864087101709653E-18 ) ) ;
#7934 = ORIENTED_EDGE ( 'NONE', *, *, #30543, .F. ) ;
#7935 = ORIENTED_EDGE ( 'NONE', *, *, #27267, .T. ) ;
#7936 = DIRECTION ( 'NONE',  ( -0.000000000000000000, -1.000000000000000000, 0.000000000000000000 ) ) ;
#7937 = CARTESIAN_POINT ( 'NONE',  ( 48.94625023931840957, 25.35784706826093426, 46.10640627770150246 ) ) ;
#7938 = VECTOR ( 'NONE', #17287, 1000.000000000000000 ) ;
#7939 = CARTESIAN_POINT ( 'NONE',  ( 46.00908685603034343, 29.64624452788248021, 44.91496614357595263 ) ) ;
#7940 = CARTESIAN_POINT ( 'NONE',  ( -39.39844553691329310, -5.936069987316967556, 77.94679389045192863 ) ) ;
#7941 = CARTESIAN_POINT ( 'NONE',  ( 8.698509210239507183, 24.09164230456639544, 47.04930799450051637 ) ) ;
#7942 = ORIENTED_EDGE ( 'NONE', *, *, #25758, .F. ) ;
#7943 = CONICAL_SURFACE ( 'NONE', #7424, 55.69429210806286079, 1.269872874662818729 ) ;
#7944 = AXIS2_PLACEMENT_3D ( 'NONE', #15650, #3007, #7791 ) ;
#7945 = DIRECTION ( 'NONE',  ( -1.101824276508909887E-16, 1.000000000000000000, -0.000000000000000000 ) ) ;
#7946 = TOROIDAL_SURFACE ( 'NONE', #26280, 12.40141737965280022, 0.1249999999999992228 ) ;
#7947 = EDGE_CURVE ( 'NONE', #2831, #3387, #22312, .T. ) ;
#7948 = VERTEX_POINT ( 'NONE', #23067 ) ;
#7949 = EDGE_CURVE ( 'NONE', #14608, #17110, #20768, .T. ) ;
#7950 = EDGE_CURVE ( 'NONE', #20619, #24757, #13435, .T. ) ;
#7951 = EDGE_CURVE ( 'NONE', #14963, #13965, #7659, .T. ) ;
#7952 = ADVANCED_FACE ( 'NONE', ( #25852 ), #32311, .T. ) ;
#7953 = DIRECTION ( 'NONE',  ( 1.188208965918165239E-16, 1.880121038077813132E-16, 1.000000000000000000 ) ) ;
#7954 = ADVANCED_FACE ( 'NONE', ( #23714 ), #11868, .T. ) ;
#7955 = AXIS2_PLACEMENT_3D ( 'NONE', #32135, #31963, #4389 ) ;
#7956 = ORIENTED_EDGE ( 'NONE', *, *, #16284, .T. ) ;
#7957 = DIRECTION ( 'NONE',  ( -1.000000000000000000, 0.000000000000000000, 0.000000000000000000 ) ) ;
#7958 = DIRECTION ( 'NONE',  ( -1.000000000000000000, 0.000000000000000000, 0.000000000000000000 ) ) ;
#7959 = CARTESIAN_POINT ( 'NONE',  ( 21.09992658989239089, 23.59164230456639544, 47.04930799450051637 ) ) ;
#7960 = CARTESIAN_POINT ( 'NONE',  ( 21.09785597605720042, -14.04221034894631615, -11.81388374861560386 ) ) ;
#7961 = CARTESIAN_POINT ( 'NONE',  ( -40.69349378885117119, 6.789343923716915974, 39.46053429011656988 ) ) ;
#7962 = ORIENTED_EDGE ( 'NONE', *, *, #32323, .T. ) ;
#7963 = CARTESIAN_POINT ( 'NONE',  ( 72.35058027291680105, 5.005525289648620202, 77.65196428233004156 ) ) ;
#7964 = CARTESIAN_POINT ( 'NONE',  ( 47.17209261226641104, 29.58954579224849368, 44.97563639035409011 ) ) ;
#7965 = CARTESIAN_POINT ( 'NONE',  ( -41.23380787120766655, 11.23768311167744294, 37.04930799450052348 ) ) ;
#7966 = DIRECTION ( 'NONE',  ( -1.101824276508909887E-16, 1.000000000000000000, -0.000000000000000000 ) ) ;
#7967 = AXIS2_PLACEMENT_3D ( 'NONE', #25669, #3012, #21053 ) ;
#7968 = CARTESIAN_POINT ( 'NONE',  ( 21.09785597605720042, -52.14605111273580462, -31.45069200549948363 ) ) ;
#7969 = ORIENTED_EDGE ( 'NONE', *, *, #31621, .T. ) ;
#7970 = CIRCLE ( 'NONE', #16874, 0.1250000000000001110 ) ;
#7971 = DIRECTION ( 'NONE',  ( -0.2756373558169932236, 0.9612616959383205595, 2.536267806945839542E-31 ) ) ;
#7972 = DIRECTION ( 'NONE',  ( 1.000000000000000000, 0.000000000000000000, 0.000000000000000000 ) ) ;
#7973 = ORIENTED_EDGE ( 'NONE', *, *, #6236, .F. ) ;
#7974 = CARTESIAN_POINT ( 'NONE',  ( 21.09785597605720042, -6.704410789454799513, 114.3782204971654721 ) ) ;
#7975 = CARTESIAN_POINT ( 'NONE',  ( 21.09992658989239089, 26.34184655352419213, 47.04930799450051637 ) ) ;
#7976 = DIRECTION ( 'NONE',  ( -1.101824276508909887E-16, 1.000000000000000000, -0.000000000000000000 ) ) ;
#7977 = CARTESIAN_POINT ( 'NONE',  ( 21.09785597605719332, 6.717634499306958773, 47.04930799450051637 ) ) ;
#7978 = VERTEX_POINT ( 'NONE', #586 ) ;
#7979 = DIRECTION ( 'NONE',  ( -0.2756373558169938898, 0.9612616959383203374, 0.000000000000000000 ) ) ;
#7980 = ORIENTED_EDGE ( 'NONE', *, *, #18729, .T. ) ;
#7981 = EDGE_CURVE ( 'NONE', #25543, #19007, #6295, .T. ) ;
#7982 = AXIS2_PLACEMENT_3D ( 'NONE', #27367, #24742, #17175 ) ;
#7983 = ORIENTED_EDGE ( 'NONE', *, *, #15361, .F. ) ;
#7984 = TOROIDAL_SURFACE ( 'NONE', #2757, 12.61792373059897621, 0.1249999999999970163 ) ;
#7985 = VECTOR ( 'NONE', #6874, 1000.000000000000114 ) ;
#7986 = CARTESIAN_POINT ( 'NONE',  ( 51.92911259730841067, -5.935667572904989697, -13.50884708582312754 ) ) ;
#7987 = FACE_OUTER_BOUND ( 'NONE', #27315, .T. ) ;
#7988 = CARTESIAN_POINT ( 'NONE',  ( -40.59581018552366061, 9.375516295340281303, 34.64930799450051779 ) ) ;
#7989 = ADVANCED_FACE ( 'NONE', ( #28486 ), #13450, .F. ) ;
#7990 = VERTEX_POINT ( 'NONE', #3523 ) ;
#7991 = ORIENTED_EDGE ( 'NONE', *, *, #15495, .T. ) ;
#7992 = CARTESIAN_POINT ( 'NONE',  ( 48.05211795450447454, 25.13954579807170120, 48.91997206816282784 ) ) ;
#7993 = DIRECTION ( 'NONE',  ( 0.7141240004913222972, -0.3958453973320028019, -0.5773502691896303940 ) ) ;
#7994 = CARTESIAN_POINT ( 'NONE',  ( -40.08841711228579641, 7.575633567407562552, 60.54930799450051637 ) ) ;
#7995 = DIRECTION ( 'NONE',  ( 0.8718554444429661432, -0.4832773644130859969, 0.07944226231105885883 ) ) ;
#7996 = ORIENTED_EDGE ( 'NONE', *, *, #30719, .F. ) ;
#7997 = DIRECTION ( 'NONE',  ( -1.000000000000000000, 0.000000000000000000, 0.000000000000000000 ) ) ;
#7998 = ORIENTED_EDGE ( 'NONE', *, *, #16622, .T. ) ;
#7999 = FACE_OUTER_BOUND ( 'NONE', #15040, .T. ) ;
#8000 = PLANE ( 'NONE',  #15804 ) ;
#8001 = ORIENTED_EDGE ( 'NONE', *, *, #20077, .T. ) ;
#8002 = DIRECTION ( 'NONE',  ( -1.000000000000000000, 0.000000000000000000, 0.000000000000000000 ) ) ;
#8003 = DIRECTION ( 'NONE',  ( -1.224646799147353207E-16, 0.000000000000000000, -1.000000000000000000 ) ) ;
#8004 = CARTESIAN_POINT ( 'NONE',  ( -42.39006672483308336, 15.27003693862973854, 38.54111136810265492 ) ) ;
#8005 = DIRECTION ( 'NONE',  ( -1.000000000000000000, 0.000000000000000000, 0.000000000000000000 ) ) ;
#8006 = TOROIDAL_SURFACE ( 'NONE', #660, 13.48414152717812797, 1.000000000001010525 ) ;
#8007 = CARTESIAN_POINT ( 'NONE',  ( 34.39950969015404780, 17.36474115922713324, 47.04930799450052348 ) ) ;
#8008 = DIRECTION ( 'NONE',  ( -1.000000000000000000, 0.000000000000000000, 0.000000000000000000 ) ) ;
#8009 = CARTESIAN_POINT ( 'NONE',  ( 21.09992658989239089, 30.59164230456639544, 47.04930799450051637 ) ) ;
#8010 = ADVANCED_FACE ( 'NONE', ( #18136 ), #12392, .T. ) ;
#8011 = AXIS2_PLACEMENT_3D ( 'NONE', #23643, #28571, #16084 ) ;
#8012 = EDGE_LOOP ( 'NONE', ( #22770, #5356, #27666, #7485, #21329 ) ) ;
#8013 = LINE ( 'NONE', #20471, #32416 ) ;
#8015 = ADVANCED_FACE ( 'NONE', ( #1067 ), #4343, .F. ) ;
#8014 = AXIS2_PLACEMENT_3D ( 'NONE', #10302, #30163, #12603 ) ;
#8016 = DIRECTION ( 'NONE',  ( 0.000000000000000000, -0.000000000000000000, -1.000000000000000000 ) ) ;
#8017 = ORIENTED_EDGE ( 'NONE', *, *, #31304, .F. ) ;
#8018 = AXIS2_PLACEMENT_3D ( 'NONE', #14101, #17188, #16542 ) ;
#8019 = ORIENTED_EDGE ( 'NONE', *, *, #4418, .F. ) ;
#8020 = DIRECTION ( 'NONE',  ( -1.000000000000000000, 0.000000000000000000, 0.000000000000000000 ) ) ;
#8021 = EDGE_CURVE ( 'NONE', #13639, #29498, #30222, .T. ) ;
#8022 = B_SPLINE_CURVE_WITH_KNOTS ( 'NONE', 3,
 ( #30211, #7406, #5097, #9, #30054, #10028, #17889, #19694, #17563, #7725, #2313, #7565 ),
 .UNSPECIFIED., .F., .F.,
 ( 4, 2, 2, 2, 2, 4 ),
 ( 0.0003078418816934655748, 0.0003848023521168218177, 0.0004232825873285107812, 0.0004617628225401997446, 0.0005387232929635631974, 0.0006156837633869265960 ),
 .UNSPECIFIED. ) ;
#8023 = EDGE_CURVE ( 'NONE', #27032, #13059, #28724, .T. ) ;
#8024 = ORIENTED_EDGE ( 'NONE', *, *, #9156, .T. ) ;
#8025 = CIRCLE ( 'NONE', #17969, 12.36707279061065101 ) ;
#8026 = B_SPLINE_SURFACE_WITH_KNOTS ( 'NONE', 3, 1, ( 
 ( #7770, #10077 ),
 ( #22039, #19580 ),
 ( #24677, #15317 ),
 ( #20074, #30103 ),
 ( #32068, #17771 ),
 ( #2195, #27791 ) ),
 .UNSPECIFIED., .F., .F., .F.,
 ( 4, 1, 1, 4 ),
 ( 2, 2 ),
 ( 0.1800733115436725096, 0.4989925988945991819, 0.7849997004460342875, 1.000000000000000000 ),
 ( 0.000000000000000000, 1.000000000000000000 ),
 .UNSPECIFIED. ) ;
#8027 = ORIENTED_EDGE ( 'NONE', *, *, #17297, .F. ) ;
#8028 = AXIS2_PLACEMENT_3D ( 'NONE', #17543, #14928, #17379 ) ;
#8029 = CARTESIAN_POINT ( 'NONE',  ( 80.77181806311267565, -5.935454207752202116, 16.07118271501079576 ) ) ;
#8030 = EDGE_CURVE ( 'NONE', #17109, #8696, #8184, .T. ) ;
#8031 = EDGE_LOOP ( 'NONE', ( #19966, #10291 ) ) ;
#8032 = CARTESIAN_POINT ( 'NONE',  ( 33.46699938050303302, 38.56284415653841791, 47.04930799450051637 ) ) ;
#8033 = AXIS2_PLACEMENT_3D ( 'NONE', #18959, #21911, #11425 ) ;
#8034 =( BOUNDED_CURVE ( )  B_SPLINE_CURVE ( 3, ( #7473, #27323, #10262, #22222 ),
 .UNSPECIFIED., .F., .F. ) 
 B_SPLINE_CURVE_WITH_KNOTS ( ( 4, 4 ),
 ( 5.766788280868928140, 6.283185307179586232 ),
 .UNSPECIFIED. ) 
 CURVE ( )  GEOMETRIC_REPRESENTATION_ITEM ( )  RATIONAL_B_SPLINE_CURVE ( ( 1.000000000000000000, 0.9779010246516586236, 0.9779010246516586236, 1.000000000000000000 ) ) 
 REPRESENTATION_ITEM ( '' )  );
#8035 = CIRCLE ( 'NONE', #2264, 0.1249999999999966416 ) ;
#8036 = CARTESIAN_POINT ( 'NONE',  ( 48.64577015523532566, 29.40030387703340864, 45.36886888450657551 ) ) ;
#8037 = CARTESIAN_POINT ( 'NONE',  ( -42.92070284191122909, 15.66940288633442790, 37.04930799450052348 ) ) ;
#8038 = CARTESIAN_POINT ( 'NONE',  ( 48.80717017713595141, 27.97622849631043351, 48.15820438821415195 ) ) ;
#8039 = VERTEX_POINT ( 'NONE', #2038 ) ;
#8040 = ORIENTED_EDGE ( 'NONE', *, *, #29353, .T. ) ;
#8041 = DIRECTION ( 'NONE',  ( 0.000000000000000000, -0.000000000000000000, -1.000000000000000000 ) ) ;
#8042 = ORIENTED_EDGE ( 'NONE', *, *, #26257, .F. ) ;
#8043 = DIRECTION ( 'NONE',  ( -0.4544104193609908027, -5.611869858668450607E-17, -0.8907924397839086517 ) ) ;
#8044 = CARTESIAN_POINT ( 'NONE',  ( 54.68827974814350767, -3.654479441960587049, 103.0408807978937347 ) ) ;
#8045 = DIRECTION ( 'NONE',  ( -1.101824276508909887E-16, 1.000000000000000000, -0.000000000000000000 ) ) ;
#8046 = LINE ( 'NONE', #4927, #30977 ) ;
#8047 = DIRECTION ( 'NONE',  ( -0.9612616959383206705, -0.2756373558169931681, 1.660411357259282445E-16 ) ) ;
#8048 = ADVANCED_FACE ( 'NONE', ( #21724 ), #9765, .T. ) ;
#8049 = ORIENTED_EDGE ( 'NONE', *, *, #24115, .T. ) ;
#8050 = FACE_OUTER_BOUND ( 'NONE', #27214, .T. ) ;
#8051 = CARTESIAN_POINT ( 'NONE',  ( 9.016997203727585841, 15.24673779880127356, 46.73295957419995261 ) ) ;
#8052 = ADVANCED_FACE ( 'NONE', ( #21562 ), #30746, .T. ) ;
#8053 = CARTESIAN_POINT ( 'NONE',  ( -41.52218637998914375, 11.15499190493234849, 35.90717268343339441 ) ) ;
#8054 = TOROIDAL_SURFACE ( 'NONE', #11182, 32.50000000000000000, 1.000000000000000888 ) ;
#8055 = DIRECTION ( 'NONE',  ( -2.946248497964555786E-19, -3.001156285468303092E-19, -1.000000000000000000 ) ) ;
#8056 = AXIS2_PLACEMENT_3D ( 'NONE', #20654, #10975, #20969 ) ;
#8057 = ORIENTED_EDGE ( 'NONE', *, *, #1626, .F. ) ;
#8058 = FACE_OUTER_BOUND ( 'NONE', #20804, .T. ) ;
#8059 = CARTESIAN_POINT ( 'NONE',  ( -40.50726676055796105, 7.559560307024983494, 53.80788663826320573 ) ) ;
#8060 = EDGE_CURVE ( 'NONE', #4648, #31644, #858, .T. ) ;
#8061 = CARTESIAN_POINT ( 'NONE',  ( -40.90015969217747482, 8.955334253785164123, 56.14611646155296398 ) ) ;
#8062 = EDGE_CURVE ( 'NONE', #28626, #21972, #26986, .T. ) ;
#8063 = ORIENTED_EDGE ( 'NONE', *, *, #6595, .T. ) ;
#8064 = AXIS2_PLACEMENT_3D ( 'NONE', #28959, #11879, #3838 ) ;
#8065 = AXIS2_PLACEMENT_3D ( 'NONE', #25555, #9816, #25073 ) ;
#8066 = EDGE_LOOP ( 'NONE', ( #17641, #9786, #28569, #31788 ) ) ;
#8067 = ORIENTED_EDGE ( 'NONE', *, *, #19664, .T. ) ;
#8068 = CARTESIAN_POINT ( 'NONE',  ( -41.13156850465621517, 9.429949956619452678, 38.44930799450052916 ) ) ;
#8069 = CARTESIAN_POINT ( 'NONE',  ( 21.09992658989239089, 26.46664230456639899, 47.04930799450051637 ) ) ;
#8070 = ORIENTED_EDGE ( 'NONE', *, *, #27616, .T. ) ;
#8071 = AXIS2_PLACEMENT_3D ( 'NONE', #25652, #13199, #3323 ) ;
#8072 = CARTESIAN_POINT ( 'NONE',  ( -38.65545646816406133, 2.267353962593735339, 79.30155859000750240 ) ) ;
#8073 = DIRECTION ( 'NONE',  ( -1.101824276508909887E-16, 1.000000000000000000, -0.000000000000000000 ) ) ;
#8074 = CARTESIAN_POINT ( 'NONE',  ( 8.474859994195286461, 27.34184655352419568, 47.04930799450051637 ) ) ;
#8075 = CARTESIAN_POINT ( 'NONE',  ( -40.59689739711614465, 7.533859135569301202, 53.64930799450051779 ) ) ;
#8076 = CARTESIAN_POINT ( 'NONE',  ( -37.21204910874186567, -5.721341737285086992, 78.89649703355408406 ) ) ;
#8077 = DIRECTION ( 'NONE',  ( 0.9612616959383205595, 0.2756373558169931681, -1.660411357259282445E-16 ) ) ;
#8079 = AXIS2_PLACEMENT_3D ( 'NONE', #29640, #24052, #11909 ) ;
#8078 = FACE_OUTER_BOUND ( 'NONE', #31960, .T. ) ;
#8080 = FACE_OUTER_BOUND ( 'NONE', #24110, .T. ) ;
#8081 = CYLINDRICAL_SURFACE ( 'NONE', #16807, 10.00000000000000178 ) ;
#8082 = CARTESIAN_POINT ( 'NONE',  ( -40.11286833322907341, 2.887657226147507306, 38.94930799450052206 ) ) ;
#8083 = EDGE_CURVE ( 'NONE', #16663, #11145, #28638, .T. ) ;
#8084 = DIRECTION ( 'NONE',  ( -1.101824276508909887E-16, 1.000000000000000000, -0.000000000000000000 ) ) ;
#8085 = ORIENTED_EDGE ( 'NONE', *, *, #16987, .F. ) ;
#8086 = ORIENTED_EDGE ( 'NONE', *, *, #23084, .T. ) ;
#8087 = CARTESIAN_POINT ( 'NONE',  ( 55.14312657641617221, -13.30632128221581389, 91.42653303877501969 ) ) ;
#8088 = FACE_OUTER_BOUND ( 'NONE', #23912, .T. ) ;
#8089 = ADVANCED_FACE ( 'NONE', ( #4172 ), #28803, .T. ) ;
#8090 = CARTESIAN_POINT ( 'NONE',  ( 21.09992658989238734, 31.71664230456639544, 47.04930799450051637 ) ) ;
#8091 = ORIENTED_EDGE ( 'NONE', *, *, #26981, .F. ) ;
#8092 = FACE_OUTER_BOUND ( 'NONE', #6759, .T. ) ;
#8093 = DIRECTION ( 'NONE',  ( 1.234978253042719660E-16, -1.000000000000000000, -1.170965406187439618E-31 ) ) ;
#8094 = ORIENTED_EDGE ( 'NONE', *, *, #26409, .T. ) ;
#8095 = VERTEX_POINT ( 'NONE', #6966 ) ;
#8096 = LINE ( 'NONE', #12863, #11042 ) ;
#8097 = CARTESIAN_POINT ( 'NONE',  ( 48.18662509608405031, 27.98284706826092716, 49.18364984542562013 ) ) ;
#8098 = DIRECTION ( 'NONE',  ( -0.4848096202463645921, -0.8746197071393805311, 0.000000000000000000 ) ) ;
#8099 = EDGE_CURVE ( 'NONE', #5841, #28361, #11328, .T. ) ;
#8100 = CARTESIAN_POINT ( 'NONE',  ( -39.40864382708623737, -5.936121150865079521, 77.92057279823603722 ) ) ;
#8101 = CIRCLE ( 'NONE', #22301, 0.6999999999999992895 ) ;
#8102 = AXIS2_PLACEMENT_3D ( 'NONE', #2480, #30066, #25133 ) ;
#8103 = VERTEX_POINT ( 'NONE', #21392 ) ;
#8104 = DIRECTION ( 'NONE',  ( 0.8746197071393925215, -0.4848096202463429982, -8.676864087101708112E-18 ) ) ;
#8105 = DIRECTION ( 'NONE',  ( -1.000000000000000000, 0.000000000000000000, 0.000000000000000000 ) ) ;
#8106 = ORIENTED_EDGE ( 'NONE', *, *, #30902, .F. ) ;
#8107 = CARTESIAN_POINT ( 'NONE',  ( 45.52675994804781112, 26.83420399681022772, 49.47108226228596806 ) ) ;
#8108 = PRODUCT_DEFINITION ( 'UNKNOWN', '', #16576, #2878 ) ;
#8109 = DIRECTION ( 'NONE',  ( 0.000000000000000000, -1.000000000000000000, 0.000000000000000000 ) ) ;
#8110 = ORIENTED_EDGE ( 'NONE', *, *, #1214, .F. ) ;
#8111 = CARTESIAN_POINT ( 'NONE',  ( -41.94956971822180947, 3.905757428664828890, 47.04930799450051637 ) ) ;
#8112 = DIRECTION ( 'NONE',  ( -1.000000000000000000, 0.000000000000000000, 0.000000000000000000 ) ) ;
#8113 = CARTESIAN_POINT ( 'NONE',  ( -43.38408989745150990, 1.111547985471240008, 53.64930799450051779 ) ) ;
#8114 = VECTOR ( 'NONE', #18217, 1000.000000000000000 ) ;
#8115 = AXIS2_PLACEMENT_3D ( 'NONE', #4467, #3531, #8472 ) ;
#8116 = FACE_OUTER_BOUND ( 'NONE', #20740, .T. ) ;
#8117 = ORIENTED_EDGE ( 'NONE', *, *, #7494, .T. ) ;
#8118 = CARTESIAN_POINT ( 'NONE',  ( 21.09785597605720397, -15.93545420775219945, -24.25069200549945947 ) ) ;
#8119 = CYLINDRICAL_SURFACE ( 'NONE', #4292, 0.1000000000000007272 ) ;
#8120 = CONICAL_SURFACE ( 'NONE', #4984, 55.68770647617149905, 0.3009234521320683364 ) ;
#8121 = AXIS2_PLACEMENT_3D ( 'NONE', #32131, #5376, #14896 ) ;
#8122 = CARTESIAN_POINT ( 'NONE',  ( 21.09785597605719687, 40.56454579224779877, 14.54930799450051460 ) ) ;
#8123 = DIRECTION ( 'NONE',  ( -1.000000000000000000, 0.000000000000000000, 0.000000000000000000 ) ) ;
#8124 = CIRCLE ( 'NONE', #8659, 12.27641737965282687 ) ;
#8125 = CARTESIAN_POINT ( 'NONE',  ( 48.83059987400640267, 26.15948166895303473, 48.97189179988551899 ) ) ;
#8126 = ORIENTED_EDGE ( 'NONE', *, *, #28038, .F. ) ;
#8127 = CARTESIAN_POINT ( 'NONE',  ( 72.46310410352278097, 9.702389020015065313, 73.75010705023584023 ) ) ;
#8128 = CARTESIAN_POINT ( 'NONE',  ( -40.54770213959439218, 7.393765961829922517, 38.67976136800678688 ) ) ;
#8129 = DIRECTION ( 'NONE',  ( -0.2756373558169932236, 0.9612616959383204485, -1.479773560108267395E-16 ) ) ;
#8130 = ORIENTED_EDGE ( 'NONE', *, *, #11685, .T. ) ;
#8131 = DIRECTION ( 'NONE',  ( -0.000000000000000000, -1.000000000000000000, -0.000000000000000000 ) ) ;
#8132 = DIRECTION ( 'NONE',  ( 0.4848096202463317295, 0.8746197071393987388, 0.000000000000000000 ) ) ;
#8133 = DIRECTION ( 'NONE',  ( -0.000000000000000000, -1.000000000000000000, 0.000000000000000000 ) ) ;
#8134 = EDGE_CURVE ( 'NONE', #19940, #23798, #23872, .T. ) ;
#8135 = DIRECTION ( 'NONE',  ( -1.000000000000000000, 0.000000000000000000, 0.000000000000000000 ) ) ;
#8136 = EDGE_CURVE ( 'NONE', #2286, #30366, #2935, .T. ) ;
#8137 = ADVANCED_FACE ( 'NONE', ( #9102 ), #24029, .T. ) ;
#8138 = VERTEX_POINT ( 'NONE', #24195 ) ;
#8139 = EDGE_CURVE ( 'NONE', #22591, #6106, #11731, .T. ) ;
#8140 = CARTESIAN_POINT ( 'NONE',  ( -38.36853489569023168, 7.065850718397949315, 32.14930799450051779 ) ) ;
#8141 = ORIENTED_EDGE ( 'NONE', *, *, #1070, .T. ) ;
#8142 = ORIENTED_EDGE ( 'NONE', *, *, #2432, .F. ) ;
#8143 = CONICAL_SURFACE ( 'NONE', #2881, 20.38082872909741994, 1.021642509542357802 ) ;
#8144 = AXIS2_PLACEMENT_3D ( 'NONE', #31126, #31281, #25867 ) ;
#8145 = CIRCLE ( 'NONE', #12338, 2.499999999999999112 ) ;
#8146 = CIRCLE ( 'NONE', #25451, 69.99901951359278485 ) ;
#8147 = CARTESIAN_POINT ( 'NONE',  ( -9.774954067741020936, -5.936747322758278322, 107.7512220956005820 ) ) ;
#8148 = CARTESIAN_POINT ( 'NONE',  ( 8.474859994195286461, 27.84184655352419568, 47.04930799450051637 ) ) ;
#8149 = ORIENTED_EDGE ( 'NONE', *, *, #28320, .F. ) ;
#8150 = CARTESIAN_POINT ( 'NONE',  ( 37.10355168477130405, 14.99513937955032716, 47.04930799450052348 ) ) ;
#8151 = ORIENTED_EDGE ( 'NONE', *, *, #30902, .T. ) ;
#8152 = DIRECTION ( 'NONE',  ( -1.000000000000000000, 0.000000000000000000, 0.000000000000000000 ) ) ;
#8153 = DIRECTION ( 'NONE',  ( 0.000000000000000000, -1.000000000000000000, 0.000000000000000000 ) ) ;
#8154 = CARTESIAN_POINT ( 'NONE',  ( -35.94335002548523050, -4.770075702498624892, 80.07727748070902862 ) ) ;
#8155 = DIRECTION ( 'NONE',  ( 0.000000000000000000, 0.000000000000000000, 1.000000000000000000 ) ) ;
#8156 = ORIENTED_EDGE ( 'NONE', *, *, #12456, .T. ) ;
#8157 = CARTESIAN_POINT ( 'NONE',  ( -10.16734060525942951, 3.903925281081630505, 98.61598880062605588 ) ) ;
#8158 = ORIENTED_EDGE ( 'NONE', *, *, #12700, .F. ) ;
#8159 = SPHERICAL_SURFACE ( 'NONE', #12837, 0.1000000000000000056 ) ;
#8160 = DIRECTION ( 'NONE',  ( 0.000000000000000000, 1.000000000000000000, 0.000000000000000000 ) ) ;
#8161 = ORIENTED_EDGE ( 'NONE', *, *, #19565, .F. ) ;
#8162 = DIRECTION ( 'NONE',  ( 0.02617694830786587712, 1.759793992609925531E-18, 0.9996573249755574819 ) ) ;
#8163 = CARTESIAN_POINT ( 'NONE',  ( -12.90214402394279603, -5.098646251524523443, 47.04930799450052348 ) ) ;
#8164 = DIRECTION ( 'NONE',  ( -1.000000000000000000, 0.000000000000000000, 0.000000000000000000 ) ) ;
#8165 = DIRECTION ( 'NONE',  ( -1.000000000000000000, 0.000000000000000000, 0.000000000000000000 ) ) ;
#8166 = AXIS2_PLACEMENT_3D ( 'NONE', #23755, #26052, #16361 ) ;
#8167 = DIRECTION ( 'NONE',  ( -1.101824276508909887E-16, 1.000000000000000000, -0.000000000000000000 ) ) ;
#8168 = CARTESIAN_POINT ( 'NONE',  ( 21.09785597605720042, 17.56454579224779877, 96.02477317163219084 ) ) ;
#8169 = EDGE_LOOP ( 'NONE', ( #19802, #6687, #4968, #28670 ) ) ;
#8170 = CARTESIAN_POINT ( 'NONE',  ( -40.57832940339291383, 7.446916344587776848, 53.64930799450051779 ) ) ;
#8171 = ORIENTED_EDGE ( 'NONE', *, *, #18599, .F. ) ;
#8172 = AXIS2_PLACEMENT_3D ( 'NONE', #6286, #1354, #5977 ) ;
#8173 = CIRCLE ( 'NONE', #22776, 0.1250000000000001110 ) ;
#8174 = DIRECTION ( 'NONE',  ( -0.000000000000000000, -1.000000000000000000, 0.000000000000000000 ) ) ;
#8175 = EDGE_CURVE ( 'NONE', #29193, #29823, #2436, .T. ) ;
#8176 = ADVANCED_FACE ( 'NONE', ( #68 ), #22215, .F. ) ;
#8177 = ORIENTED_EDGE ( 'NONE', *, *, #13597, .T. ) ;
#8178 = EDGE_CURVE ( 'NONE', #24565, #12553, #21811, .T. ) ;
#8179 = ORIENTED_EDGE ( 'NONE', *, *, #2718, .F. ) ;
#8180 = CARTESIAN_POINT ( 'NONE',  ( -11.66034778524429782, 1.102830191789060388, 100.4616804541535515 ) ) ;
#8181 = ADVANCED_FACE ( 'NONE', ( #7779 ), #4505, .T. ) ;
#8182 = AXIS2_PLACEMENT_3D ( 'NONE', #1949, #14280, #11968 ) ;
#8183 = ORIENTED_EDGE ( 'NONE', *, *, #1991, .T. ) ;
#8184 = B_SPLINE_CURVE_WITH_KNOTS ( 'NONE', 3,
 ( #26335, #12057, #29457, #16481 ),
 .UNSPECIFIED., .F., .F.,
 ( 4, 4 ),
 ( 0.000000000000000000, 1.000000000000000000 ),
 .UNSPECIFIED. ) ;
#8185 = VERTEX_POINT ( 'NONE', #25341 ) ;
#8186 = CARTESIAN_POINT ( 'NONE',  ( 21.09785597605720753, 14.86454579224779948, 47.04930799450052348 ) ) ;
#8187 = AXIS2_PLACEMENT_3D ( 'NONE', #18230, #26109, #20705 ) ;
#8188 = ORIENTED_EDGE ( 'NONE', *, *, #11756, .F. ) ;
#8189 = CARTESIAN_POINT ( 'NONE',  ( -43.90780810587784089, -0.03953120679776488122, 61.94930799450052206 ) ) ;
#8190 = CARTESIAN_POINT ( 'NONE',  ( 49.07982864979221205, 29.33081545780508392, 45.80760694353075735 ) ) ;
#8191 = DIRECTION ( 'NONE',  ( -1.101824276508909887E-16, 1.000000000000000000, -0.000000000000000000 ) ) ;
#8192 = CARTESIAN_POINT ( 'NONE',  ( 47.20353132263855400, 26.80956182964376566, 45.01455027646041174 ) ) ;
#8193 = EDGE_CURVE ( 'NONE', #2479, #29694, #12722, .T. ) ;
#8194 = VERTEX_POINT ( 'NONE', #17780 ) ;
#8195 = ORIENTED_EDGE ( 'NONE', *, *, #19559, .F. ) ;
#8196 = SURFACE_SIDE_STYLE ('',( #26057 ) ) ;
#8197 = ADVANCED_FACE ( 'NONE', ( #19752 ), #22859, .F. ) ;
#8198 = EDGE_LOOP ( 'NONE', ( #30412, #20913, #9673, #26979 ) ) ;
#8199 = AXIS2_PLACEMENT_3D ( 'NONE', #9267, #28967, #16633 ) ;
#8200 = CARTESIAN_POINT ( 'NONE',  ( 33.50134396954523908, 27.84164230456639544, 47.04930799450051637 ) ) ;
#8201 = DIRECTION ( 'NONE',  ( -0.000000000000000000, -1.000000000000000000, -0.000000000000000000 ) ) ;
#8202 = LINE ( 'NONE', #10506, #168 ) ;
#8203 = CARTESIAN_POINT ( 'NONE',  ( 67.37777719198106752, 14.81645899701909563, 47.04930799450051637 ) ) ;
#8204 = CYLINDRICAL_SURFACE ( 'NONE', #18435, 0.1000000000000006301 ) ;
#8205 = VERTEX_POINT ( 'NONE', #9595 ) ;
#8206 = DIRECTION ( 'NONE',  ( -0.000000000000000000, -1.000000000000000000, 0.000000000000000000 ) ) ;
#8207 = DIRECTION ( 'NONE',  ( 1.000000000000000000, 0.000000000000000000, 0.000000000000000000 ) ) ;
#8208 = FACE_OUTER_BOUND ( 'NONE', #17964, .T. ) ;
#8209 = CARTESIAN_POINT ( 'NONE',  ( 44.70507715278255034, 25.64951373492759856, 46.92503878583767118 ) ) ;
#8210 = EDGE_LOOP ( 'NONE', ( #29395, #11555, #5777, #16565, #485, #28106, #8240 ) ) ;
#8211 = LINE ( 'NONE', #22966, #30901 ) ;
#8212 = DIRECTION ( 'NONE',  ( 0.000000000000000000, -0.000000000000000000, -1.000000000000000000 ) ) ;
#8213 = EDGE_CURVE ( 'NONE', #2756, #23081, #10828, .T. ) ;
#8214 = CIRCLE ( 'NONE', #12413, 1.000000000000000888 ) ;
#8215 = ORIENTED_EDGE ( 'NONE', *, *, #5746, .F. ) ;
#8216 = AXIS2_PLACEMENT_3D ( 'NONE', #4617, #30067, #23 ) ;
#8217 = ORIENTED_EDGE ( 'NONE', *, *, #13239, .T. ) ;
#8218 =( BOUNDED_CURVE ( )  B_SPLINE_CURVE ( 2, ( #31006, #22951, #10504, #3262, #20327 ),
 .UNSPECIFIED., .F., .F. ) 
 B_SPLINE_CURVE_WITH_KNOTS ( ( 3, 2, 3 ),
 ( 0.7671007452297479157, 0.8333333333333333703, 1.000000000000000000 ),
 .UNSPECIFIED. ) 
 CURVE ( )  GEOMETRIC_REPRESENTATION_ITEM ( )  RATIONAL_B_SPLINE_CURVE ( ( 0.9358335845890755067, 0.9467590945150633486, 1.000000000000000000, 0.8660254037844387076, 1.000000000000000000 ) ) 
 REPRESENTATION_ITEM ( '' )  );
#8219 = ORIENTED_EDGE ( 'NONE', *, *, #18335, .T. ) ;
#8220 = EDGE_CURVE ( 'NONE', #14804, #28351, #8702, .T. ) ;
#8221 = CARTESIAN_POINT ( 'NONE',  ( -25.65214402394279247, 13.61454579224779771, 47.04930799450052348 ) ) ;
#8222 = FACE_OUTER_BOUND ( 'NONE', #13117, .T. ) ;
#8223 = CARTESIAN_POINT ( 'NONE',  ( 49.19517401419062708, 27.70920399681022772, 48.40991706654173754 ) ) ;
#8224 = EDGE_CURVE ( 'NONE', #14081, #4732, #2692, .T. ) ;
#8225 = ORIENTED_EDGE ( 'NONE', *, *, #7820, .F. ) ;
#8226 = CARTESIAN_POINT ( 'NONE',  ( -31.86441722936940479, -13.30632128221581212, 65.03308317646940395 ) ) ;
#8227 = DIRECTION ( 'NONE',  ( 2.946248497964555786E-19, 3.001156285468303092E-19, 1.000000000000000000 ) ) ;
#8228 = DIRECTION ( 'NONE',  ( 0.8746197071393925215, -0.4848096202463429982, -8.676864087101708112E-18 ) ) ;
#8229 = EDGE_CURVE ( 'NONE', #12341, #15078, #12915, .T. ) ;
#8230 = CIRCLE ( 'NONE', #3508, 12.36707279061065101 ) ;
#8231 = CARTESIAN_POINT ( 'NONE',  ( 48.43931949325730812, 22.91889071986277671, 48.25583407606420394 ) ) ;
#8232 = ADVANCED_FACE ( 'NONE', ( #227 ), #7690, .F. ) ;
#8233 = DIRECTION ( 'NONE',  ( 0.000000000000000000, 0.000000000000000000, 1.000000000000000000 ) ) ;
#8234 = EDGE_CURVE ( 'NONE', #10451, #30053, #19705, .T. ) ;
#8235 = DIRECTION ( 'NONE',  ( -1.000000000000000000, -1.101824276508909887E-16, 0.000000000000000000 ) ) ;
#8236 = CARTESIAN_POINT ( 'NONE',  ( -43.90780810587784089, -0.03953120679776488122, 62.04930799450052348 ) ) ;
#8237 = CARTESIAN_POINT ( 'NONE',  ( 8.732853799281732776, 32.47145308207317527, 47.04930799450051637 ) ) ;
#8238 = CARTESIAN_POINT ( 'NONE',  ( -40.60251150970604073, 6.748447833883065350, 53.54930799450051637 ) ) ;
#8239 = CARTESIAN_POINT ( 'NONE',  ( 48.73570333863616355, 29.22287913140504045, 44.52463952959527660 ) ) ;
#8240 = ORIENTED_EDGE ( 'NONE', *, *, #5359, .F. ) ;
#8241 = ORIENTED_EDGE ( 'NONE', *, *, #13066, .T. ) ;
#8242 = CARTESIAN_POINT ( 'NONE',  ( -43.95628906790246759, -0.1269931775117038586, 32.14930799450051779 ) ) ;
#8243 = CARTESIAN_POINT ( 'NONE',  ( 21.09992658989238734, 38.56284415653841791, 47.04930799450051637 ) ) ;
#8244 = CIRCLE ( 'NONE', #30782, 12.62506659569710266 ) ;
#8245 = DIRECTION ( 'NONE',  ( -1.000000000000000000, -1.101824276508910010E-16, 0.000000000000000000 ) ) ;
#8246 = ORIENTED_EDGE ( 'NONE', *, *, #5594, .T. ) ;
#8247 = FACE_OUTER_BOUND ( 'NONE', #26863, .T. ) ;
#8248 = CARTESIAN_POINT ( 'NONE',  ( -40.11036131418491379, 6.815955993705610894, 39.36132530173779287 ) ) ;
#8249 = ORIENTED_EDGE ( 'NONE', *, *, #7457, .F. ) ;
#8250 = FACE_OUTER_BOUND ( 'NONE', #21328, .T. ) ;
#8251 = CARTESIAN_POINT ( 'NONE',  ( 49.49063479933183629, 25.99951373492759643, 47.17357720316391578 ) ) ;
#8252 = EDGE_CURVE ( 'NONE', #26196, #17663, #23908, .T. ) ;
#8253 = CARTESIAN_POINT ( 'NONE',  ( 45.35708200440645044, 29.00457786121581805, 45.92000246470679770 ) ) ;
#8254 = CARTESIAN_POINT ( 'NONE',  ( -35.09106279755485502, 10.89041806307759686, 52.27948292994979340 ) ) ;
#8255 = CIRCLE ( 'NONE', #19786, 2.000000000000001776 ) ;
#8256 = ORIENTED_EDGE ( 'NONE', *, *, #19061, .T. ) ;
#8257 = CIRCLE ( 'NONE', #28705, 0.1250000000000001110 ) ;
#8258 = EDGE_CURVE ( 'NONE', #10938, #26186, #3990, .T. ) ;
#8259 = CARTESIAN_POINT ( 'NONE',  ( 51.97066601985542178, -5.936747322758275658, -13.65260610659960250 ) ) ;
#8260 = CARTESIAN_POINT ( 'NONE',  ( 21.09785597605720753, -5.098646251524523443, 47.04930799450052348 ) ) ;
#8261 = ADVANCED_FACE ( 'NONE', ( #27479 ), #29158, .T. ) ;
#8262 = EDGE_LOOP ( 'NONE', ( #10849, #4103, #17155, #22691, #17438, #10528, #4192 ) ) ;
#8263 = CARTESIAN_POINT ( 'NONE',  ( 46.96819297411687444, 26.89253733014356129, 49.54594323136014822 ) ) ;
#8264 = CARTESIAN_POINT ( 'NONE',  ( 46.79153437246152691, 23.10527845304106265, 47.52148899368456370 ) ) ;
#8265 = CARTESIAN_POINT ( 'NONE',  ( -43.37834615508418068, 1.121909970995875971, 34.64930799450052490 ) ) ;
#8266 = ADVANCED_FACE ( 'NONE', ( #12390 ), #15010, .T. ) ;
#8267 = ORIENTED_EDGE ( 'NONE', *, *, #5396, .T. ) ;
#8268 = CARTESIAN_POINT ( 'NONE',  ( -63.90214402394282445, 11.92558985988973497, 67.46350265493038023 ) ) ;
#8269 = EDGE_CURVE ( 'NONE', #16793, #3554, #23393, .T. ) ;
#8270 = B_SPLINE_CURVE_WITH_KNOTS ( 'NONE', 3,
 ( #20122, #27180, #27355, #22092, #12265, #29659, #30154, #7664, #19957, #5639, #15642, #7166, #17163, #22256, #32286, #22414, #14886, #9959, #29986, #15048, #7502, #25054, #2565, #12595, #18422, #31077, #9065, #15963, #16447, #21352, #13838, #11211, #3651, #13516, #8736, #6445 ),
 .UNSPECIFIED., .F., .F.,
 ( 4, 2, 2, 2, 2, 2, 2, 2, 2, 2, 2, 2, 2, 2, 2, 2, 2, 4 ),
 ( 0.000000000000000000, 0.0006656200208596524523, 0.001331240041719304905, 0.002662480083438613712, 0.003993720125157922303, 0.004659340146017577032, 0.005324960166877230894, 0.005990580187736883888, 0.006656200208596539485, 0.007987440250315827259, 0.009318680292035115900, 0.01064992033375440454, 0.01331240041719298182, 0.01464364045891227914, 0.01597488050063157472, 0.01863736058407016241, 0.01996860062578946146, 0.02129984066750875704 ),
 .UNSPECIFIED. ) ;
#8271 = CARTESIAN_POINT ( 'NONE',  ( 8.732853799281738105, 28.21183152705961206, 47.04930799450051637 ) ) ;
#8272 = DIRECTION ( 'NONE',  ( 0.000000000000000000, -0.000000000000000000, -1.000000000000000000 ) ) ;
#8273 = LINE ( 'NONE', #28297, #29416 ) ;
#8274 = ORIENTED_EDGE ( 'NONE', *, *, #21152, .T. ) ;
#8275 = CARTESIAN_POINT ( 'NONE',  ( 46.58637386172244277, 23.04411619146718238, 46.04663644226216945 ) ) ;
#8276 = FACE_OUTER_BOUND ( 'NONE', #29547, .T. ) ;
#8277 = CARTESIAN_POINT ( 'NONE',  ( 21.09785597605720753, 14.56454579224780232, 47.04930799450052348 ) ) ;
#8278 = DIRECTION ( 'NONE',  ( 0.000000000000000000, 1.000000000000000000, 0.000000000000000000 ) ) ;
#8279 = DIRECTION ( 'NONE',  ( -0.000000000000000000, -1.000000000000000000, -0.000000000000000000 ) ) ;
#8280 = VERTEX_POINT ( 'NONE', #30112 ) ;
#8281 = DIRECTION ( 'NONE',  ( 0.000000000000000000, -1.000000000000000000, 0.000000000000000000 ) ) ;
#8282 = AXIS2_PLACEMENT_3D ( 'NONE', #31660, #9167, #9986 ) ;
#8283 = EDGE_LOOP ( 'NONE', ( #19216, #3017, #23475, #14545 ) ) ;
#8284 = CARTESIAN_POINT ( 'NONE',  ( 9.016997203727582288, 34.59164230456639899, 46.73295957419995261 ) ) ;
#8285 = DIRECTION ( 'NONE',  ( 0.000000000000000000, 0.000000000000000000, -1.000000000000000000 ) ) ;
#8286 = CARTESIAN_POINT ( 'NONE',  ( -39.85048242108726413, 2.742214340073605428, 48.54930799450051637 ) ) ;
#8287 = AXIS2_PLACEMENT_3D ( 'NONE', #2693, #2845, #22714 ) ;
#8288 = DIRECTION ( 'NONE',  ( 0.000000000000000000, 0.000000000000000000, 1.000000000000000000 ) ) ;
#8289 = VERTEX_POINT ( 'NONE', #18574 ) ;
#8290 = PRODUCT_DEFINITION_SHAPE ( 'NONE', 'NONE',  #25954 ) ;
#8291 = DIRECTION ( 'NONE',  ( -1.224646799147353207E-16, 0.000000000000000000, -1.000000000000000000 ) ) ;
#8292 = EDGE_LOOP ( 'NONE', ( #18475, #25919, #28695, #14084 ) ) ;
#8293 = ORIENTED_EDGE ( 'NONE', *, *, #5463, .F. ) ;
#8294 = TOROIDAL_SURFACE ( 'NONE', #8820, 12.40141737965287838, 0.1249999999999998335 ) ;
#8295 = CIRCLE ( 'NONE', #4610, 16.99999999999999289 ) ;
#8296 = AXIS2_PLACEMENT_3D ( 'NONE', #18745, #23692, #1360 ) ;
#8297 = AXIS2_PLACEMENT_3D ( 'NONE', #20636, #30658, #28189 ) ;
#8298 = DIRECTION ( 'NONE',  ( -0.000000000000000000, -1.000000000000000000, 0.000000000000000000 ) ) ;
#8299 = LINE ( 'NONE', #10448, #6186 ) ;
#8300 = EDGE_CURVE ( 'NONE', #19861, #10177, #11763, .T. ) ;
#8301 = ORIENTED_EDGE ( 'NONE', *, *, #4000, .F. ) ;
#8302 = CIRCLE ( 'NONE', #25595, 0.1999999999999987899 ) ;
#8303 = DIRECTION ( 'NONE',  ( 0.000000000000000000, -0.000000000000000000, -1.000000000000000000 ) ) ;
#8304 = ORIENTED_EDGE ( 'NONE', *, *, #3394, .F. ) ;
#8305 = EDGE_CURVE ( 'NONE', #18206, #26412, #18101, .T. ) ;
#8306 = LINE ( 'NONE', #25861, #9940 ) ;
#8307 = DIRECTION ( 'NONE',  ( 7.588956326749211550E-18, -4.206627182996912454E-18, 1.000000000000000000 ) ) ;
#8308 = CARTESIAN_POINT ( 'NONE',  ( -35.39203252561370761, -4.222325579252183658, 80.41835680688559762 ) ) ;
#8309 = CARTESIAN_POINT ( 'NONE',  ( 48.04075769285628894, 25.18284706826092645, 48.89770225776209145 ) ) ;
#8310 = ORIENTED_EDGE ( 'NONE', *, *, #9477, .T. ) ;
#8311 = DIRECTION ( 'NONE',  ( -0.000000000000000000, -1.000000000000000000, -0.000000000000000000 ) ) ;
#8312 = ORIENTED_EDGE ( 'NONE', *, *, #31100, .F. ) ;
#8313 = DIRECTION ( 'NONE',  ( -1.224646799147353207E-16, -1.349345573449484691E-32, 1.000000000000000000 ) ) ;
#8314 = CARTESIAN_POINT ( 'NONE',  ( 21.09785597605719332, 30.56454579224779522, 47.04930799450051637 ) ) ;
#8315 = VERTEX_POINT ( 'NONE', #21040 ) ;
#8316 = CARTESIAN_POINT ( 'NONE',  ( 47.11751843720308841, 23.11533908250407165, 46.67071160955749320 ) ) ;
#8317 = CARTESIAN_POINT ( 'NONE',  ( -35.41180783471520499, 11.63092686814241539, 52.99606787449828715 ) ) ;
#8318 = DIRECTION ( 'NONE',  ( -0.4848096202463636484, -0.8746197071393810862, 0.000000000000000000 ) ) ;
#8319 = CARTESIAN_POINT ( 'NONE',  ( 21.09785597605720753, 15.70210863493540288, 47.04930799450052348 ) ) ;
#8320 = CARTESIAN_POINT ( 'NONE',  ( 46.99023568444673060, 25.73791119454915588, 49.12151524109405898 ) ) ;
#8321 = ORIENTED_EDGE ( 'NONE', *, *, #5169, .T. ) ;
#8322 = DIRECTION ( 'NONE',  ( 0.8746197071393960742, -0.4848096202463368365, -1.277302113040972115E-17 ) ) ;
#8323 = FACE_OUTER_BOUND ( 'NONE', #8012, .T. ) ;
#8324 = ORIENTED_EDGE ( 'NONE', *, *, #17254, .F. ) ;
#8325 = CARTESIAN_POINT ( 'NONE',  ( 33.71785032049130137, 31.71664230456639544, 47.04930799450051637 ) ) ;
#8326 = CIRCLE ( 'NONE', #14599, 12.36707279061065279 ) ;
#8327 = CONICAL_SURFACE ( 'NONE', #11971, 13.20165371409683708, 1.570144820418440945 ) ;
#8328 = CARTESIAN_POINT ( 'NONE',  ( -9.970446611220443955, -5.937394852768786535, -13.57859485750651629 ) ) ;
#8329 = AXIS2_PLACEMENT_3D ( 'NONE', #32185, #31694, #27083 ) ;
#8330 = ORIENTED_EDGE ( 'NONE', *, *, #17614, .T. ) ;
#8331 = AXIS2_PLACEMENT_3D ( 'NONE', #27338, #29974, #8285 ) ;
#8332 = ORIENTED_EDGE ( 'NONE', *, *, #24151, .T. ) ;
#8333 = CARTESIAN_POINT ( 'NONE',  ( -8.652076904411645231, 6.325917197325520824, 98.88062770172314231 ) ) ;
#8334 = AXIS2_PLACEMENT_3D ( 'NONE', #21020, #18875, #13813 ) ;
#8335 = VERTEX_POINT ( 'NONE', #5637 ) ;
#8336 = ORIENTED_EDGE ( 'NONE', *, *, #18045, .T. ) ;
#8337 = CARTESIAN_POINT ( 'NONE',  ( 71.49893360114315044, 8.310461108307681144, 18.62663443640233041 ) ) ;
#8338 = AXIS2_PLACEMENT_3D ( 'NONE', #18760, #31588, #24021 ) ;
#8339 = ORIENTED_EDGE ( 'NONE', *, *, #16699, .F. ) ;
#8340 = ADVANCED_FACE ( 'NONE', ( #25656 ), #3160, .T. ) ;
#8341 = DIRECTION ( 'NONE',  ( 1.000000000000000000, 0.000000000000000000, 0.000000000000000000 ) ) ;
#8342 = ADVANCED_FACE ( 'NONE', ( #13360 ), #30120, .T. ) ;
#8343 = CARTESIAN_POINT ( 'NONE',  ( 48.37591806664303107, 29.43873978692154481, 45.20163774776087706 ) ) ;
#8344 = DIRECTION ( 'NONE',  ( -1.000000000000000000, 0.000000000000000000, 0.000000000000000000 ) ) ;
#8345 = EDGE_CURVE ( 'NONE', #8315, #8733, #11244, .T. ) ;
#8346 = ADVANCED_FACE ( 'NONE', ( #30913 ), #20400, .F. ) ;
#8347 = CARTESIAN_POINT ( 'NONE',  ( 46.99218062947583974, 26.45956182964376424, 49.08406571254116102 ) ) ;
#8348 = ORIENTED_EDGE ( 'NONE', *, *, #5537, .T. ) ;
#8349 = VERTEX_POINT ( 'NONE', #11056 ) ;
#8350 = FILL_AREA_STYLE ('',( #18184 ) ) ;
#8351 = ORIENTED_EDGE ( 'NONE', *, *, #22484, .T. ) ;
#8352 = CIRCLE ( 'NONE', #24585, 0.1000000000000018235 ) ;
#8353 = CARTESIAN_POINT ( 'NONE',  ( 8.474859994195286461, 28.59184655352419213, 47.04930799450051637 ) ) ;
#8354 = DIRECTION ( 'NONE',  ( 1.188208965918165239E-16, 1.880121038077813132E-16, 1.000000000000000000 ) ) ;
#8355 = CARTESIAN_POINT ( 'NONE',  ( 21.09992658989238734, 32.22145308207317527, 47.04930799450051637 ) ) ;
#8356 = CIRCLE ( 'NONE', #13149, 71.99999999999998579 ) ;
#8357 = DIRECTION ( 'NONE',  ( -1.000000000000000000, 0.000000000000000000, 0.000000000000000000 ) ) ;
#8358 = LINE ( 'NONE', #13935, #28998 ) ;
#8359 = ORIENTED_EDGE ( 'NONE', *, *, #23039, .T. ) ;
#8360 = CARTESIAN_POINT ( 'NONE',  ( 21.09992658989238734, 31.34143805560860585, 47.04930799450051637 ) ) ;
#8361 = DIRECTION ( 'NONE',  ( 0.000000000000000000, 1.000000000000000000, -0.000000000000000000 ) ) ;
#8362 = CARTESIAN_POINT ( 'NONE',  ( -9.751947285419857891, -5.936248947737087889, 107.5569174314780838 ) ) ;
#8363 = CARTESIAN_POINT ( 'NONE',  ( 48.83862994770795041, 25.94118040159426641, 48.17861352429476085 ) ) ;
#8364 = VERTEX_POINT ( 'NONE', #30433 ) ;
#8365 = DIRECTION ( 'NONE',  ( 0.000000000000000000, 0.000000000000000000, -1.000000000000000000 ) ) ;
#8366 = CARTESIAN_POINT ( 'NONE',  ( 21.09785597605720753, 13.86454579224779948, 47.04930799450052348 ) ) ;
#8367 = AXIS2_PLACEMENT_3D ( 'NONE', #7992, #3044, #758 ) ;
#8368 = CIRCLE ( 'NONE', #26695, 0.1250000000000001110 ) ;
#8369 = VERTEX_POINT ( 'NONE', #5966 ) ;
#8370 = ADVANCED_FACE ( 'NONE', ( #8425 ), #31677, .T. ) ;
#8371 = EDGE_CURVE ( 'NONE', #1586, #19917, #4947, .T. ) ;
#8372 = CONICAL_SURFACE ( 'NONE', #1540, 55.68770647617149905, 0.3009234521320683364 ) ;
#8373 = CIRCLE ( 'NONE', #26170, 48.63405236513555963 ) ;
#8374 = ORIENTED_EDGE ( 'NONE', *, *, #5422, .F. ) ;
#8375 = AXIS2_PLACEMENT_3D ( 'NONE', #32153, #9664, #17194 ) ;
#8376 = ORIENTED_EDGE ( 'NONE', *, *, #1110, .F. ) ;
#8377 = LINE ( 'NONE', #18377, #23300 ) ;
#8378 = AXIS2_PLACEMENT_3D ( 'NONE', #9004, #29030, #6546 ) ;
#8379 = FACE_OUTER_BOUND ( 'NONE', #9291, .T. ) ;
#8380 = CARTESIAN_POINT ( 'NONE',  ( 48.23388202445966044, 27.65087065737811756, 49.27628909396056400 ) ) ;
#8381 = ORIENTED_EDGE ( 'NONE', *, *, #27873, .T. ) ;
#8382 = CARTESIAN_POINT ( 'NONE',  ( 21.09785597605719332, 15.56454579224779877, -1.926157182631158093 ) ) ;
#8383 = CARTESIAN_POINT ( 'NONE',  ( -40.13606231985500017, 7.635531802539802015, 60.44930799450051495 ) ) ;
#8384 = DIRECTION ( 'NONE',  ( -1.101824276508909887E-16, 1.000000000000000000, -0.000000000000000000 ) ) ;
#8385 = EDGE_CURVE ( 'NONE', #13254, #5658, #17945, .T. ) ;
#8386 = EDGE_LOOP ( 'NONE', ( #32476, #23442, #3540, #3009 ) ) ;
#8387 = DIRECTION ( 'NONE',  ( -0.9612616959383205595, -0.2756373558169931681, 1.660411357259282445E-16 ) ) ;
#8388 = TOROIDAL_SURFACE ( 'NONE', #4700, 12.40141737965288726, 0.1250000000000003331 ) ;
#8389 = VECTOR ( 'NONE', #6278, 1000.000000000000000 ) ;
#8390 = VERTEX_POINT ( 'NONE', #13514 ) ;
#8391 = FACE_OUTER_BOUND ( 'NONE', #17282, .T. ) ;
#8392 = DIRECTION ( 'NONE',  ( 0.1949050434465251225, -0.6797146636928670382, 0.7071067811865481278 ) ) ;
#8393 = CARTESIAN_POINT ( 'NONE',  ( -30.89605511857140741, 11.92558985988973497, 26.63511333407100423 ) ) ;
#8394 = DIRECTION ( 'NONE',  ( -0.000000000000000000, -0.000000000000000000, -1.000000000000000000 ) ) ;
#8395 = LINE ( 'NONE', #8238, #9474 ) ;
#8396 = ORIENTED_EDGE ( 'NONE', *, *, #21513, .F. ) ;
#8397 = ORIENTED_EDGE ( 'NONE', *, *, #23276, .T. ) ;
#8398 = DIRECTION ( 'NONE',  ( 0.7141240004913198547, -0.3958453973320100738, 0.5773502691896283956 ) ) ;
#8399 = CARTESIAN_POINT ( 'NONE',  ( 33.72499318558949000, 38.56284415653841791, 47.04930799450051637 ) ) ;
#8400 = CIRCLE ( 'NONE', #26214, 58.66319174311612272 ) ;
#8401 = CIRCLE ( 'NONE', #12055, 12.36707279061065101 ) ;
#8402 = CARTESIAN_POINT ( 'NONE',  ( 21.09992658989239089, 29.09164230456639899, 47.04930799450051637 ) ) ;
#8403 = ORIENTED_EDGE ( 'NONE', *, *, #24893, .T. ) ;
#8404 = CARTESIAN_POINT ( 'NONE',  ( 21.09992658989238734, 31.34164230456639544, 47.04930799450051637 ) ) ;
#8405 = CIRCLE ( 'NONE', #26738, 0.1000000000000004774 ) ;
#8406 = FACE_OUTER_BOUND ( 'NONE', #2472, .T. ) ;
#8407 = EDGE_CURVE ( 'NONE', #16381, #8613, #15486, .T. ) ;
#8408 = ORIENTED_EDGE ( 'NONE', *, *, #13860, .T. ) ;
#8409 = CARTESIAN_POINT ( 'NONE',  ( -40.51002469154155250, 7.586466571548067250, 60.22268384422984155 ) ) ;
#8410 = AXIS2_PLACEMENT_3D ( 'NONE', #1403, #13892, #11586 ) ;
#8411 = CARTESIAN_POINT ( 'NONE',  ( 49.41945501136223839, 29.16454579807170688, 45.86501535757901848 ) ) ;
#8412 = CIRCLE ( 'NONE', #6837, 1.500000000000001332 ) ;
#8413 = EDGE_CURVE ( 'NONE', #12114, #21033, #16459, .T. ) ;
#8414 = PLANE ( 'NONE',  #4909 ) ;
#8415 =( BOUNDED_CURVE ( )  B_SPLINE_CURVE ( 3, ( #28709, #6227, #30859, #16228 ),
 .UNSPECIFIED., .F., .F. ) 
 B_SPLINE_CURVE_WITH_KNOTS ( ( 4, 4 ),
 ( 5.497787143782109531, 6.283185307179586232 ),
 .UNSPECIFIED. ) 
 CURVE ( )  GEOMETRIC_REPRESENTATION_ITEM ( )  RATIONAL_B_SPLINE_CURVE ( ( 1.000000000000000000, 0.9492530216741874582, 0.9492530216741874582, 1.000000000000000000 ) ) 
 REPRESENTATION_ITEM ( '' )  );
#8416 = EDGE_CURVE ( 'NONE', #25372, #19042, #9662, .T. ) ;
#8417 = VECTOR ( 'NONE', #1352, 1000.000000000000114 ) ;
#8418 = EDGE_CURVE ( 'NONE', #3515, #17291, #12828, .T. ) ;
#8419 = EDGE_LOOP ( 'NONE', ( #1071, #20201, #2505, #13175 ) ) ;
#8420 = CARTESIAN_POINT ( 'NONE',  ( 51.95647403453392599, -5.936463533621009425, -13.64747408757448000 ) ) ;
#8421 = CARTESIAN_POINT ( 'NONE',  ( 21.09785597605719332, 25.56454579224779877, 35.24930799450054053 ) ) ;
#8422 = TOROIDAL_SURFACE ( 'NONE', #3156, 1.899999999999999467, 0.1000000000000000056 ) ;
#8423 = ORIENTED_EDGE ( 'NONE', *, *, #16443, .F. ) ;
#8424 = AXIS2_PLACEMENT_3D ( 'NONE', #3781, #16252, #31365 ) ;
#8425 = FACE_OUTER_BOUND ( 'NONE', #2759, .T. ) ;
#8426 = VECTOR ( 'NONE', #14368, 1000.000000000000000 ) ;
#8427 = EDGE_CURVE ( 'NONE', #8280, #2451, #15811, .T. ) ;
#8428 = CIRCLE ( 'NONE', #15679, 12.36707279061065101 ) ;
#8429 = CARTESIAN_POINT ( 'NONE',  ( -40.69193635511749108, 9.347952559758583746, 39.44930799450052206 ) ) ;
#8430 = AXIS2_PLACEMENT_3D ( 'NONE', #11906, #24049, #21905 ) ;
#8431 = ORIENTED_EDGE ( 'NONE', *, *, #2408, .F. ) ;
#8432 = DIRECTION ( 'NONE',  ( -1.000000000000000000, -1.101824276508910010E-16, 0.000000000000000000 ) ) ;
#8433 = CARTESIAN_POINT ( 'NONE',  ( -41.02113223168485234, 7.230835263863472306, 39.54930799450052348 ) ) ;
#8434 = DIRECTION ( 'NONE',  ( -0.9275012328650849014, -0.3738200944756011057, 0.000000000000000000 ) ) ;
#8435 = CARTESIAN_POINT ( 'NONE',  ( 21.09785597605719332, 17.36451738380053555, 59.73344952167762756 ) ) ;
#8436 = ORIENTED_EDGE ( 'NONE', *, *, #23389, .F. ) ;
#8437 = CARTESIAN_POINT ( 'NONE',  ( 46.53577443378190281, 23.10527845304106620, 47.02011620365084354 ) ) ;
#8438 = DIRECTION ( 'NONE',  ( -0.4848096202463430537, -0.8746197071393926326, -9.920727850371701658E-18 ) ) ;
#8439 = CONICAL_SURFACE ( 'NONE', #22037, 58.09216821878680292, 1.269872874662833384 ) ;
#8440 = DIRECTION ( 'NONE',  ( -0.000000000000000000, -1.000000000000000000, 0.000000000000000000 ) ) ;
#8441 = DIRECTION ( 'NONE',  ( -1.000000000000000000, 0.000000000000000000, 0.000000000000000000 ) ) ;
#8442 = DIRECTION ( 'NONE',  ( -1.000000000000000000, -0.000000000000000000, -0.000000000000000000 ) ) ;
#8443 = ORIENTED_EDGE ( 'NONE', *, *, #29864, .F. ) ;
#8444 = CARTESIAN_POINT ( 'NONE',  ( 47.14013642192045239, 29.60499367036002738, 44.99018544319649493 ) ) ;
#8445 = CARTESIAN_POINT ( 'NONE',  ( 49.66977585544405827, 24.86874180309281712, 46.07579470028509405 ) ) ;
#8446 = FACE_OUTER_BOUND ( 'NONE', #29279, .T. ) ;
#8447 = EDGE_CURVE ( 'NONE', #4649, #3283, #1182, .T. ) ;
#8448 = ORIENTED_EDGE ( 'NONE', *, *, #8586, .T. ) ;
#8449 = DIRECTION ( 'NONE',  ( 1.000000000000000000, 0.000000000000000000, 0.000000000000000000 ) ) ;
#8450 = FACE_OUTER_BOUND ( 'NONE', #29835, .T. ) ;
#8451 = EDGE_CURVE ( 'NONE', #9995, #25118, #28001, .T. ) ;
#8452 = CARTESIAN_POINT ( 'NONE',  ( 54.53781794026635055, -0.7249253372050199484, -7.132871347344132751 ) ) ;
#8453 = ORIENTED_EDGE ( 'NONE', *, *, #4545, .F. ) ;
#8454 = CARTESIAN_POINT ( 'NONE',  ( 48.76626135000090301, 22.93328494799376216, 47.45974698848920781 ) ) ;
#8455 = AXIS2_PLACEMENT_3D ( 'NONE', #5736, #23613, #26398 ) ;
#8456 = ORIENTED_EDGE ( 'NONE', *, *, #27085, .F. ) ;
#8457 =( GEOMETRIC_REPRESENTATION_CONTEXT ( 3 ) GLOBAL_UNCERTAINTY_ASSIGNED_CONTEXT ( ( #9465 ) ) GLOBAL_UNIT_ASSIGNED_CONTEXT ( ( #11738, #29629, #2536 ) ) REPRESENTATION_CONTEXT ( 'NONE', 'WORKASPACE' ) );
#8458 = AXIS2_PLACEMENT_3D ( 'NONE', #11710, #16612, #21703 ) ;
#8459 = EDGE_CURVE ( 'NONE', #27336, #27995, #14389, .T. ) ;
#8460 = VERTEX_POINT ( 'NONE', #23990 ) ;
#8461 = ADVANCED_FACE ( 'NONE', ( #11363 ), #18564, .T. ) ;
#8462 = ADVANCED_BREP_SHAPE_REPRESENTATION ( '', ( #12396, #8172 ), #824 ) ;
#8463 = AXIS2_PLACEMENT_3D ( 'NONE', #29919, #7433, #509 ) ;
#8464 = CARTESIAN_POINT ( 'NONE',  ( -35.20269728567959078, -4.936580443452697864, 79.94253044896541383 ) ) ;
#8465 = CARTESIAN_POINT ( 'NONE',  ( 41.59785597605720397, 13.86454579224779948, 47.04930799450052348 ) ) ;
#8466 = ORIENTED_EDGE ( 'NONE', *, *, #26036, .F. ) ;
#8467 = CARTESIAN_POINT ( 'NONE',  ( -40.58268305512095964, 6.836408824202115042, 34.54930799450052348 ) ) ;
#8468 = ORIENTED_EDGE ( 'NONE', *, *, #25650, .F. ) ;
#8469 = CIRCLE ( 'NONE', #16838, 0.1250000000000001110 ) ;
#8470 = CARTESIAN_POINT ( 'NONE',  ( -7.324817582041172948, 8.310461108307681144, 97.43646483284780402 ) ) ;
#8471 = AXIS2_PLACEMENT_3D ( 'NONE', #29639, #29970, #2545 ) ;
#8472 = DIRECTION ( 'NONE',  ( 0.000000000000000000, 0.000000000000000000, -1.000000000000000000 ) ) ;
#8473 = CARTESIAN_POINT ( 'NONE',  ( -37.21204910874186567, -5.721341737285086992, 78.89649703355408406 ) ) ;
#8474 = CARTESIAN_POINT ( 'NONE',  ( 21.09785597605719332, 25.76454579224776964, 78.54930799450052348 ) ) ;
#8475=STYLED_ITEM('',(#32529),#12176);
#8476 = ORIENTED_EDGE ( 'NONE', *, *, #26462, .T. ) ;
#8477 = CARTESIAN_POINT ( 'NONE',  ( 47.09785597605719687, 25.56454579224779877, 49.54930799450042400 ) ) ;
#8478 = DIRECTION ( 'NONE',  ( -1.101824276508909887E-16, 1.000000000000000000, -0.000000000000000000 ) ) ;
#8479 = LINE ( 'NONE', #3219, #1828 ) ;
#8480 = DIRECTION ( 'NONE',  ( -0.000000000000000000, -1.000000000000000000, 0.000000000000000000 ) ) ;
#8481 = EDGE_LOOP ( 'NONE', ( #2771, #30404, #12044, #21320 ) ) ;
#8482 = DIRECTION ( 'NONE',  ( -1.000000000000000000, 0.000000000000000000, 0.000000000000000000 ) ) ;
#8483 = DIRECTION ( 'NONE',  ( 0.8746197071393926326, -0.4848096202463430537, -8.676864087101709653E-18 ) ) ;
#8484 = CARTESIAN_POINT ( 'NONE',  ( 33.37634396954523197, 28.34164230456639544, 47.04930799450051637 ) ) ;
#8485 = FACE_OUTER_BOUND ( 'NONE', #11900, .T. ) ;
#8486 = DIRECTION ( 'NONE',  ( -1.101824276508909887E-16, 1.000000000000000000, -0.000000000000000000 ) ) ;
#8487 = EDGE_LOOP ( 'NONE', ( #19293, #20432, #2394, #11194 ) ) ;
#8488 = CARTESIAN_POINT ( 'NONE',  ( 21.09785597605719332, 48.06454579224779877, 47.04930799450051637 ) ) ;
#8489 = CARTESIAN_POINT ( 'NONE',  ( -40.68074350590972443, 6.811995273158242270, 34.67891654026473702 ) ) ;
#8490 = EDGE_CURVE ( 'NONE', #12822, #19635, #19072, .T. ) ;
#8491 = ORIENTED_EDGE ( 'NONE', *, *, #18488, .F. ) ;
#8492 = DIRECTION ( 'NONE',  ( -1.000000000000000000, 0.000000000000000000, 0.000000000000000000 ) ) ;
#8493 = AXIS2_PLACEMENT_3D ( 'NONE', #31322, #4234, #25626 ) ;
#8494 = DIRECTION ( 'NONE',  ( 0.8746197071393925215, -0.4848096202463429982, -8.676864087101708112E-18 ) ) ;
#8495 = EDGE_LOOP ( 'NONE', ( #24135, #11001, #30540, #10185, #7715 ) ) ;
#8496 = ORIENTED_EDGE ( 'NONE', *, *, #22667, .F. ) ;
#8497 = CARTESIAN_POINT ( 'NONE',  ( -11.05776695470940041, -5.581242224120388506, 105.1022689614296723 ) ) ;
#8498 = UNCERTAINTY_MEASURE_WITH_UNIT (LENGTH_MEASURE( 1.000000000000000082E-05 ), #19687, 'distance_accuracy_value', 'NONE');
#8499 = ADVANCED_FACE ( 'NONE', ( #1503 ), #10726, .T. ) ;
#8500 = ORIENTED_EDGE ( 'NONE', *, *, #707, .T. ) ;
#8501 = CIRCLE ( 'NONE', #7454, 2.749999999999998224 ) ;
#8502 = ADVANCED_BREP_SHAPE_REPRESENTATION ( '', ( #12176, #8172 ), #26498 ) ;
#8503 = ORIENTED_EDGE ( 'NONE', *, *, #15415, .F. ) ;
#8504 = CARTESIAN_POINT ( 'NONE',  ( 21.09992658989239089, 28.59143805560861296, 47.04930799450051637 ) ) ;
#8505 = CIRCLE ( 'NONE', #18958, 33.50000000000000000 ) ;
#8506 = ORIENTED_EDGE ( 'NONE', *, *, #28574, .F. ) ;
#8507 = AXIS2_PLACEMENT_3D ( 'NONE', #4468, #14491, #32046 ) ;
#8508 = CARTESIAN_POINT ( 'NONE',  ( -40.16174044770769314, 7.468546898574135895, 60.44930799450051495 ) ) ;
#8509 = CARTESIAN_POINT ( 'NONE',  ( 21.09992658989239089, 28.96664230456639899, 47.04930799450051637 ) ) ;
#8510 = FACE_OUTER_BOUND ( 'NONE', #22203, .T. ) ;
#8511 = PRODUCT_DEFINITION ( 'UNKNOWN', '', #29164, #32435 ) ;
#8512 = CARTESIAN_POINT ( 'NONE',  ( 47.20353132263855400, 26.10956182964376637, 45.01455027646041174 ) ) ;
#8513 = VERTEX_POINT ( 'NONE', #11209 ) ;
#8514 = ORIENTED_EDGE ( 'NONE', *, *, #31895, .F. ) ;
#8515 =( NAMED_UNIT ( * ) SI_UNIT ( $, .STERADIAN. ) SOLID_ANGLE_UNIT ( ) );
#8516 = ORIENTED_EDGE ( 'NONE', *, *, #27659, .F. ) ;
#8517 = CARTESIAN_POINT ( 'NONE',  ( -41.08785830660041682, 9.277514380576528552, 39.44930799450052206 ) ) ;
#8518 = CARTESIAN_POINT ( 'NONE',  ( 54.81458501433218800, -2.123693335316776842, 101.9715971512124497 ) ) ;
#8519 = CARTESIAN_POINT ( 'NONE',  ( -25.65214402394279247, 13.61454579224779771, 47.04930799450052348 ) ) ;
#8520 = CARTESIAN_POINT ( 'NONE',  ( -9.880269303432738681, -5.935454207752202116, -10.95525492004900769 ) ) ;
#8521 = CARTESIAN_POINT ( 'NONE',  ( 21.09785597605720042, 14.77459629858661572, -7.250692005499486115 ) ) ;
#8522 = VERTEX_POINT ( 'NONE', #31715 ) ;
#8523 = CARTESIAN_POINT ( 'NONE',  ( 21.09785597605719332, 25.56454579224780232, 126.2593585008393831 ) ) ;
#8524 = CARTESIAN_POINT ( 'NONE',  ( -30.95419617802911105, 2.325935182154316827, 14.90144108804482492 ) ) ;
#8525 = DIRECTION ( 'NONE',  ( -0.9612616959383221138, -0.2756373558169876170, 0.000000000000000000 ) ) ;
#8526 = CARTESIAN_POINT ( 'NONE',  ( 48.51114023551905063, 22.99884124225578574, 46.96613737717972725 ) ) ;
#8527 = LINE ( 'NONE', #14752, #7298 ) ;
#8528 = LINE ( 'NONE', #23302, #30300 ) ;
#8529 = ORIENTED_EDGE ( 'NONE', *, *, #4755, .T. ) ;
#8530 = DIRECTION ( 'NONE',  ( 0.000000000000000000, 0.000000000000000000, -1.000000000000000000 ) ) ;
#8531 = DIRECTION ( 'NONE',  ( -1.224646799147353207E-16, 0.000000000000000000, -1.000000000000000000 ) ) ;
#8532 = EDGE_CURVE ( 'NONE', #3549, #29624, #3885, .T. ) ;
#8533 = ORIENTED_EDGE ( 'NONE', *, *, #17749, .T. ) ;
#8534 = EDGE_CURVE ( 'NONE', #11505, #14982, #31165, .T. ) ;
#8535 = EDGE_CURVE ( 'NONE', #8289, #3738, #15420, .T. ) ;
#8536 = CIRCLE ( 'NONE', #2231, 0.2000000000000012601 ) ;
#8537 = EDGE_CURVE ( 'NONE', #3738, #8289, #22773, .T. ) ;
#8538 = ADVANCED_FACE ( 'NONE', ( #26300 ), #9387, .T. ) ;
#8539 = AXIS2_PLACEMENT_3D ( 'NONE', #6404, #16406, #29212 ) ;
#8540 = AXIS2_PLACEMENT_3D ( 'NONE', #28190, #18489, #6344 ) ;
#8541 = ORIENTED_EDGE ( 'NONE', *, *, #11781, .F. ) ;
#8542 = DIRECTION ( 'NONE',  ( 0.000000000000000000, 0.000000000000000000, -1.000000000000000000 ) ) ;
#8543 = CARTESIAN_POINT ( 'NONE',  ( 21.09785597605719332, 40.56454579224779877, 47.04930799450051637 ) ) ;
#8544 = DIRECTION ( 'NONE',  ( -1.000000000000000000, 0.000000000000000000, 0.000000000000000000 ) ) ;
#8545 = ORIENTED_EDGE ( 'NONE', *, *, #20529, .T. ) ;
#8546 = DIRECTION ( 'NONE',  ( 1.000000000000000000, -0.000000000000000000, -0.000000000000000000 ) ) ;
#8547 = CARTESIAN_POINT ( 'NONE',  ( 81.53175786463043551, -5.936215030417564265, 16.05158970249792105 ) ) ;
#8548 = CARTESIAN_POINT ( 'NONE',  ( 33.46699938050304013, 27.22145308207318593, 47.04930799450050927 ) ) ;
#8549 = ORIENTED_EDGE ( 'NONE', *, *, #31907, .T. ) ;
#8550 = CARTESIAN_POINT ( 'NONE',  ( 46.09785597605720397, 13.86454579224779948, 47.04930799450052348 ) ) ;
#8551 = ORIENTED_EDGE ( 'NONE', *, *, #23594, .T. ) ;
#8552 = CYLINDRICAL_SURFACE ( 'NONE', #4952, 71.99999999999998579 ) ;
#8553 = DIRECTION ( 'NONE',  ( -0.000000000000000000, -1.000000000000000000, -0.000000000000000000 ) ) ;
#8554 = DIRECTION ( 'NONE',  ( -0.2756373558170082672, 0.9612616959383162296, 6.938893903907184201E-14 ) ) ;
#8555 = AXIS2_PLACEMENT_3D ( 'NONE', #8519, #15739, #18512 ) ;
#8556 = DIRECTION ( 'NONE',  ( -1.101824276508909887E-16, 1.000000000000000000, -0.000000000000000000 ) ) ;
#8557 = AXIS2_PLACEMENT_3D ( 'NONE', #19795, #14560, #32125 ) ;
#8558 = ORIENTED_EDGE ( 'NONE', *, *, #26902, .T. ) ;
#8559 = ORIENTED_EDGE ( 'NONE', *, *, #30471, .T. ) ;
#8560 = EDGE_CURVE ( 'NONE', #12904, #10473, #21182, .T. ) ;
#8561 = CARTESIAN_POINT ( 'NONE',  ( -40.98902310965377183, 10.38401719860223160, 36.52712545380572351 ) ) ;
#8562 = CARTESIAN_POINT ( 'NONE',  ( -43.68921302925062378, 1.179890886355839275, 34.64930799450052490 ) ) ;
#8563 = DIRECTION ( 'NONE',  ( 0.4544104193609905806, 5.611869858668446909E-17, 0.8907924397839086517 ) ) ;
#8564 = ORIENTED_EDGE ( 'NONE', *, *, #17938, .F. ) ;
#8565 = CIRCLE ( 'NONE', #27428, 84.50000000000002842 ) ;
#8566 = CARTESIAN_POINT ( 'NONE',  ( 33.46699938050304013, 26.47145308207318593, 47.04930799450050927 ) ) ;
#8567 = CIRCLE ( 'NONE', #15388, 12.62506659569710266 ) ;
#8568 = VERTEX_POINT ( 'NONE', #3811 ) ;
#8569 = DIRECTION ( 'NONE',  ( 0.9612616959383207815, 0.2756373558169927240, 8.795445018804291370E-19 ) ) ;
#8570 = CARTESIAN_POINT ( 'NONE',  ( 44.77625694075214824, 30.21454579807170049, 48.23360063142255427 ) ) ;
#8571 = CARTESIAN_POINT ( 'NONE',  ( -9.880269303432744010, -5.935454207751966749, -37.95069200549950494 ) ) ;
#8572 = ADVANCED_FACE ( 'NONE', ( #16282 ), #26959, .F. ) ;
#8573 = EDGE_CURVE ( 'NONE', #14753, #14877, #5475, .T. ) ;
#8574 = EDGE_CURVE ( 'NONE', #16617, #22868, #6442, .T. ) ;
#8575 = ORIENTED_EDGE ( 'NONE', *, *, #4213, .T. ) ;
#8576 = AXIS2_PLACEMENT_3D ( 'NONE', #14904, #19643, #14571 ) ;
#8577 = DIRECTION ( 'NONE',  ( -1.101824276508909887E-16, 1.000000000000000000, -0.000000000000000000 ) ) ;
#8578 = CARTESIAN_POINT ( 'NONE',  ( 21.09992658989239089, 30.34143805560860585, 47.04930799450051637 ) ) ;
#8579 = CARTESIAN_POINT ( 'NONE',  ( 21.09785597605719332, -5.721341737285094098, 47.04930799450051637 ) ) ;
#8580 = ORIENTED_EDGE ( 'NONE', *, *, #4107, .F. ) ;
#8581 = CIRCLE ( 'NONE', #12251, 12.36707279061065101 ) ;
#8582 = AXIS2_PLACEMENT_3D ( 'NONE', #12713, #24679, #17450 ) ;
#8583 = CARTESIAN_POINT ( 'NONE',  ( 21.09785597605719332, -16.43545420775217281, 47.04930799450051637 ) ) ;
#8584 = DIRECTION ( 'NONE',  ( 0.4848096202463645921, 0.8746197071393805311, 0.000000000000000000 ) ) ;
#8585 = CARTESIAN_POINT ( 'NONE',  ( 21.09992658989239089, 23.84164230456639544, 47.04930799450051637 ) ) ;
#8586 = EDGE_CURVE ( 'NONE', #14081, #20995, #13849, .T. ) ;
#8587 = ORIENTED_EDGE ( 'NONE', *, *, #30401, .F. ) ;
#8588 = CARTESIAN_POINT ( 'NONE',  ( 21.09992658989239089, 29.09164230456639899, 47.04930799450051637 ) ) ;
#8589 = CARTESIAN_POINT ( 'NONE',  ( -40.51045226066063520, 7.589116544599139758, 53.87859731638185679 ) ) ;
#8590 = CARTESIAN_POINT ( 'NONE',  ( 21.09785597605719332, -16.63545420775219696, -29.66074251183834676 ) ) ;
#8591 = DIRECTION ( 'NONE',  ( -2.779292025043186357E-18, 1.288349127009862211E-17, -1.000000000000000000 ) ) ;
#8592 = FILL_AREA_STYLE ('',( #31085 ) ) ;
#8593 = ORIENTED_EDGE ( 'NONE', *, *, #23785, .T. ) ;
#8594 = ADVANCED_FACE ( 'NONE', ( #1672 ), #2320, .T. ) ;
#8595 = CARTESIAN_POINT ( 'NONE',  ( 21.09992658989239089, 24.71183152705960140, 47.04930799450051637 ) ) ;
#8596 = DIRECTION ( 'NONE',  ( -1.101824276508909887E-16, 1.000000000000000000, -0.000000000000000000 ) ) ;
#8597 = ADVANCED_FACE ( 'NONE', ( #28 ), #6512, .T. ) ;
#8598 = CARTESIAN_POINT ( 'NONE',  ( 8.732853799281734553, 29.72145308207318237, 47.04930799450051637 ) ) ;
#8599 = LINE ( 'NONE', #16132, #10365 ) ;
#8600 = FACE_OUTER_BOUND ( 'NONE', #1313, .T. ) ;
#8601 = CIRCLE ( 'NONE', #28078, 12.27641737965282687 ) ;
#8602 = VERTEX_POINT ( 'NONE', #7741 ) ;
#8603 = CARTESIAN_POINT ( 'NONE',  ( 21.09785597605719332, 7.237299147902269247, 47.04930799450051637 ) ) ;
#8604 = CARTESIAN_POINT ( 'NONE',  ( -40.67014616567487195, 6.832698218566653381, 39.23645843885594786 ) ) ;
#8605 = DIRECTION ( 'NONE',  ( -0.000000000000000000, -1.000000000000000000, -0.000000000000000000 ) ) ;
#8606 = VERTEX_POINT ( 'NONE', #12182 ) ;
#8607 = DIRECTION ( 'NONE',  ( -0.8746197071393926326, 0.4848096202463430537, 8.676864087101709653E-18 ) ) ;
#8608 = DIRECTION ( 'NONE',  ( -1.000000000000000000, 0.000000000000000000, 0.000000000000000000 ) ) ;
#8609 = CARTESIAN_POINT ( 'NONE',  ( 21.09785597605719332, 40.56454579224780588, 47.04930799450051637 ) ) ;
#8610 = DIRECTION ( 'NONE',  ( -1.101824276508909887E-16, 1.000000000000000000, -0.000000000000000000 ) ) ;
#8611 = ORIENTED_EDGE ( 'NONE', *, *, #14163, .F. ) ;
#8612 = CARTESIAN_POINT ( 'NONE',  ( 21.09785597605719332, 44.06454579224779877, 46.04930799450054479 ) ) ;
#8613 = VERTEX_POINT ( 'NONE', #17582 ) ;
#8614 = EDGE_CURVE ( 'NONE', #28505, #5195, #14915, .T. ) ;
#8615 = ORIENTED_EDGE ( 'NONE', *, *, #18335, .F. ) ;
#8616 = AXIS2_PLACEMENT_3D ( 'NONE', #13997, #18898, #16445 ) ;
#8617 = PRESENTATION_LAYER_ASSIGNMENT (  '', '', ( #22245 ) ) ;
#8618 = EDGE_CURVE ( 'NONE', #8369, #31649, #9134, .T. ) ;
#8619 = DIRECTION ( 'NONE',  ( 1.188208965918165239E-16, 1.880121038077813132E-16, 1.000000000000000000 ) ) ;
#8620 = DIRECTION ( 'NONE',  ( 0.000000000000000000, 1.000000000000000000, 0.000000000000000000 ) ) ;
#8621 = CIRCLE ( 'NONE', #28037, 0.1000000000000004774 ) ;
#8622 = LINE ( 'NONE', #24031, #28747 ) ;
#8623 = AXIS2_PLACEMENT_3D ( 'NONE', #16123, #28136, #31079 ) ;
#8624 = AXIS2_PLACEMENT_3D ( 'NONE', #28075, #658, #2950 ) ;
#8625 = ADVANCED_FACE ( 'NONE', ( #22497 ), #17251, .F. ) ;
#8626 = ORIENTED_EDGE ( 'NONE', *, *, #123, .F. ) ;
#8627 = CARTESIAN_POINT ( 'NONE',  ( -40.64500813507293486, 6.819128862114091305, 34.57932936825760351 ) ) ;
#8628 = ORIENTED_EDGE ( 'NONE', *, *, #11440, .F. ) ;
#8629 = CIRCLE ( 'NONE', #20152, 2.500000000000002220 ) ;
#8630 = DIRECTION ( 'NONE',  ( -1.101824276508909887E-16, 1.000000000000000000, -0.000000000000000000 ) ) ;
#8631 = FACE_OUTER_BOUND ( 'NONE', #20778, .T. ) ;
#8632 = CARTESIAN_POINT ( 'NONE',  ( -18.90214402394280313, -5.098646251524523443, 47.04930799450052348 ) ) ;
#8633 = EDGE_LOOP ( 'NONE', ( #25859, #14377 ) ) ;
#8634 = ADVANCED_FACE ( 'NONE', ( #10049 ), #7572, .T. ) ;
#8635 = CARTESIAN_POINT ( 'NONE',  ( 21.09785597605720042, -16.03545420775220265, 47.04930799450051637 ) ) ;
#8636 = ORIENTED_EDGE ( 'NONE', *, *, #19465, .F. ) ;
#8637 = FACE_OUTER_BOUND ( 'NONE', #14352, .T. ) ;
#8638 = CARTESIAN_POINT ( 'NONE',  ( -37.21204910874186567, -5.721341737285086992, 78.89649703355408406 ) ) ;
#8639 = EDGE_CURVE ( 'NONE', #26708, #529, #17017, .T. ) ;
#8640 = VERTEX_POINT ( 'NONE', #29580 ) ;
#8641 = FACE_OUTER_BOUND ( 'NONE', #2466, .T. ) ;
#8642 = DIRECTION ( 'NONE',  ( -1.000000000000000000, 0.000000000000000000, 0.000000000000000000 ) ) ;
#8643 = CARTESIAN_POINT ( 'NONE',  ( 21.09785597605719332, -16.93042895458276575, 47.04930799450051637 ) ) ;
#8644 = DIRECTION ( 'NONE',  ( -1.101824276508909887E-16, 1.000000000000000000, -0.000000000000000000 ) ) ;
#8645 = ADVANCED_FACE ( 'NONE', ( #7425 ), #22339, .T. ) ;
#8646 = CARTESIAN_POINT ( 'NONE',  ( 48.83862994770794330, 25.15457786121582373, 48.17861352429476796 ) ) ;
#8647 = ORIENTED_EDGE ( 'NONE', *, *, #19142, .F. ) ;
#8648 = DIRECTION ( 'NONE',  ( -0.000000000000000000, -1.000000000000000000, -0.000000000000000000 ) ) ;
#8649 = CARTESIAN_POINT ( 'NONE',  ( 52.07598125554711999, -5.935454207752202116, 107.5832303370038403 ) ) ;
#8650 = ORIENTED_EDGE ( 'NONE', *, *, #1582, .F. ) ;
#8651 = CARTESIAN_POINT ( 'NONE',  ( 33.72499318558949710, 30.09184655352422411, 47.04930799450051637 ) ) ;
#8652 = DIRECTION ( 'NONE',  ( 0.1949050434465267878, -0.6797146636928667052, 0.7071067811865480168 ) ) ;
#8653 = ORIENTED_EDGE ( 'NONE', *, *, #11275, .F. ) ;
#8654 = AXIS2_PLACEMENT_3D ( 'NONE', #23952, #3612, #21483 ) ;
#8655 = VERTEX_POINT ( 'NONE', #7088 ) ;
#8656 = ADVANCED_FACE ( 'NONE', ( #32367 ), #27439, .F. ) ;
#8657 = AXIS2_PLACEMENT_3D ( 'NONE', #26873, #29172, #22099 ) ;
#8658 = AXIS2_PLACEMENT_3D ( 'NONE', #26665, #4843, #21736 ) ;
#8659 = AXIS2_PLACEMENT_3D ( 'NONE', #21963, #24112, #9512 ) ;
#8660 = VERTEX_POINT ( 'NONE', #9877 ) ;
#8661 = ORIENTED_EDGE ( 'NONE', *, *, #27387, .F. ) ;
#8662 = EDGE_CURVE ( 'NONE', #21925, #3138, #15465, .T. ) ;
#8663 = FACE_OUTER_BOUND ( 'NONE', #8292, .T. ) ;
#8664 = APPLICATION_CONTEXT ( 'automotive_design' ) ;
#8665 = EDGE_CURVE ( 'NONE', #27949, #20946, #5486, .T. ) ;
#8666 = ORIENTED_EDGE ( 'NONE', *, *, #28439, .T. ) ;
#8667 = CIRCLE ( 'NONE', #20709, 13.50178401536290806 ) ;
#8668 = CARTESIAN_POINT ( 'NONE',  ( 48.50303063523655567, 22.99884124225578574, 47.12228595530052644 ) ) ;
#8669 = DIRECTION ( 'NONE',  ( -1.000000000000000000, -1.101824276508909764E-16, 0.000000000000000000 ) ) ;
#8670 = DIRECTION ( 'NONE',  ( 0.000000000000000000, -0.7880107536067239016, -0.6156614753256557382 ) ) ;
#8671 = AXIS2_PLACEMENT_3D ( 'NONE', #17881, #12967, #10675 ) ;
#8672 = CARTESIAN_POINT ( 'NONE',  ( 48.91284552371730143, 26.69289516297710563, 46.12344667017377020 ) ) ;
#8673 = ORIENTED_EDGE ( 'NONE', *, *, #201, .F. ) ;
#8674 = ORIENTED_EDGE ( 'NONE', *, *, #5445, .F. ) ;
#8675 = VECTOR ( 'NONE', #1724, 1000.000000000000114 ) ;
#8676 = ADVANCED_FACE ( 'NONE', ( #25138 ), #4622, .T. ) ;
#8677 = EDGE_LOOP ( 'NONE', ( #13508, #16878, #13030, #10456 ) ) ;
#8678 = CARTESIAN_POINT ( 'NONE',  ( 8.732853799281738105, 23.71183152705959429, 47.04930799450051637 ) ) ;
#8679 = CARTESIAN_POINT ( 'NONE',  ( -40.47576471041815438, 7.229986682741244230, 38.88540264398079671 ) ) ;
#8680 = CIRCLE ( 'NONE', #27018, 0.1249999999999983763 ) ;
#8681 = CARTESIAN_POINT ( 'NONE',  ( -40.69230700880735441, 6.792718999258594792, 39.39980027471584378 ) ) ;
#8682 = DIRECTION ( 'NONE',  ( -1.101824276508909887E-16, 1.000000000000000000, -0.000000000000000000 ) ) ;
#8683 = CARTESIAN_POINT ( 'NONE',  ( -0.6900943036979535483, 11.83469976691315217, -5.307522563224908119 ) ) ;
#8684 = DIRECTION ( 'NONE',  ( 0.000000000000000000, 0.000000000000000000, -1.000000000000000000 ) ) ;
#8685 = ORIENTED_EDGE ( 'NONE', *, *, #30357, .F. ) ;
#8686 = DIRECTION ( 'NONE',  ( -1.101824276508909887E-16, 1.000000000000000000, -0.000000000000000000 ) ) ;
#8687 = CARTESIAN_POINT ( 'NONE',  ( -38.88086318059457369, 4.491453754352391137, 47.04930799450051637 ) ) ;
#8688 = DIRECTION ( 'NONE',  ( -1.000000000000000000, 0.000000000000000000, 0.000000000000000000 ) ) ;
#8689 = AXIS2_PLACEMENT_3D ( 'NONE', #4573, #9345, #19342 ) ;
#8690 = CARTESIAN_POINT ( 'NONE',  ( 49.19517401419062708, 25.48655426599986384, 48.40991706654173754 ) ) ;
#8691 = ORIENTED_EDGE ( 'NONE', *, *, #14464, .T. ) ;
#8692 = FACE_OUTER_BOUND ( 'NONE', #5255, .T. ) ;
#8693 = EDGE_LOOP ( 'NONE', ( #8466, #19708, #22170, #28356 ) ) ;
#8694 = CARTESIAN_POINT ( 'NONE',  ( 48.23388202445966755, 26.12822092656774586, 49.27628909396054979 ) ) ;
#8695 = DIRECTION ( 'NONE',  ( -1.101824276508909887E-16, 1.000000000000000000, -0.000000000000000000 ) ) ;
#8696 = VERTEX_POINT ( 'NONE', #32039 ) ;
#8697 = CIRCLE ( 'NONE', #2401, 12.36707279061065101 ) ;
#8698 = VECTOR ( 'NONE', #76, 1000.000000000000114 ) ;
#8699 = ORIENTED_EDGE ( 'NONE', *, *, #29493, .F. ) ;
#8700 = DIRECTION ( 'NONE',  ( 0.000000000000000000, 0.000000000000000000, 1.000000000000000000 ) ) ;
#8701 = DIRECTION ( 'NONE',  ( -1.101824276508909887E-16, 1.000000000000000000, -0.000000000000000000 ) ) ;
#8702 = CIRCLE ( 'NONE', #27051, 0.8928932188134572900 ) ;
#8703 = ORIENTED_EDGE ( 'NONE', *, *, #11132, .T. ) ;
#8704 = CARTESIAN_POINT ( 'NONE',  ( 8.482002859293478636, 32.46664230456639899, 47.04930799450051637 ) ) ;
#8705 = FACE_OUTER_BOUND ( 'NONE', #20148, .T. ) ;
#8706 = CARTESIAN_POINT ( 'NONE',  ( 47.57707823921868595, 22.93807716476589320, 48.70033069891094613 ) ) ;
#8707 = ORIENTED_EDGE ( 'NONE', *, *, #9342, .F. ) ;
#8708 = DIRECTION ( 'NONE',  ( -1.000000000000000000, 0.000000000000000000, 0.000000000000000000 ) ) ;
#8709 = EDGE_CURVE ( 'NONE', #32275, #7848, #19091, .T. ) ;
#8710 = ORIENTED_EDGE ( 'NONE', *, *, #5908, .F. ) ;
#8711 = CARTESIAN_POINT ( 'NONE',  ( 73.95065972402362320, 11.92558985988973497, 67.46350265493038023 ) ) ;
#8712 = FACE_OUTER_BOUND ( 'NONE', #8481, .T. ) ;
#8713 = CARTESIAN_POINT ( 'NONE',  ( 21.09992658989238734, 38.56284415653841791, 47.04930799450051637 ) ) ;
#8714 = SURFACE_STYLE_FILL_AREA ( #3783 ) ;
#8715 = ORIENTED_EDGE ( 'NONE', *, *, #12798, .F. ) ;
#8716 = ORIENTED_EDGE ( 'NONE', *, *, #5274, .F. ) ;
#8717 = CARTESIAN_POINT ( 'NONE',  ( 35.56915586375613003, -13.30632128221580857, 101.0770789316965903 ) ) ;
#8718 = AXIS2_PLACEMENT_3D ( 'NONE', #28108, #15614, #15462 ) ;
#8719 = LINE ( 'NONE', #13976, #12005 ) ;
#8720 = CARTESIAN_POINT ( 'NONE',  ( -42.30123736278718383, 13.66041317296246937, 59.53596428539564300 ) ) ;
#8721 = VERTEX_POINT ( 'NONE', #9720 ) ;
#8722 = CARTESIAN_POINT ( 'NONE',  ( 21.09992658989239089, 30.59164230456639544, 47.04930799450051637 ) ) ;
#8723 = SPHERICAL_SURFACE ( 'NONE', #491, 0.1000000000000000056 ) ;
#8724 = ORIENTED_EDGE ( 'NONE', *, *, #11673, .T. ) ;
#8725 = CARTESIAN_POINT ( 'NONE',  ( -40.50934420915148593, 7.581602792840986815, 60.22845019481307105 ) ) ;
#8726 = CARTESIAN_POINT ( 'NONE',  ( 48.46535932150934656, 28.28954579807170688, 49.73005965046827015 ) ) ;
#8727 = TOROIDAL_SURFACE ( 'NONE', #10848, 12.40141737965279667, 0.1249999999999991951 ) ;
#8728 = CARTESIAN_POINT ( 'NONE',  ( -40.65093765668705572, 9.567768634527945792, 38.44930799450052916 ) ) ;
#8729 = ORIENTED_EDGE ( 'NONE', *, *, #16184, .T. ) ;
#8730 = FACE_OUTER_BOUND ( 'NONE', #13903, .T. ) ;
#8731 = AXIS2_PLACEMENT_3D ( 'NONE', #21458, #23769, #4400 ) ;
#8732 = CARTESIAN_POINT ( 'NONE',  ( 45.35708200440645044, 29.79118040159425718, 45.92000246470679770 ) ) ;
#8733 = VERTEX_POINT ( 'NONE', #19713 ) ;
#8734 = DIRECTION ( 'NONE',  ( -0.000000000000000000, -1.000000000000000000, -0.000000000000000000 ) ) ;
#8735 = FACE_OUTER_BOUND ( 'NONE', #12525, .T. ) ;
#8736 = CARTESIAN_POINT ( 'NONE',  ( 71.55170771239784244, 9.423225080673425680, 20.00317117731350791 ) ) ;
#8737 = AXIS2_PLACEMENT_3D ( 'NONE', #7941, #30260, #7773 ) ;
#8738 = VERTEX_POINT ( 'NONE', #7254 ) ;
#8739 = DIRECTION ( 'NONE',  ( -1.101824276508909887E-16, 1.000000000000000000, -0.000000000000000000 ) ) ;
#8740 = EDGE_CURVE ( 'NONE', #7606, #8522, #9675, .T. ) ;
#8741 = CARTESIAN_POINT ( 'NONE',  ( 21.09785597605719687, 48.06454579224779877, 28.18735555590595609 ) ) ;
#8743 = EDGE_CURVE ( 'NONE', #9356, #28978, #24813, .T. ) ;
#8742 = DIRECTION ( 'NONE',  ( -1.000000000000000000, 0.000000000000000000, 0.000000000000000000 ) ) ;
#8744 = EDGE_CURVE ( 'NONE', #23397, #23989, #23817, .T. ) ;
#8745 = CARTESIAN_POINT ( 'NONE',  ( 45.52675994804781112, 28.11155426599984963, 49.47108226228597516 ) ) ;
#8746 = EDGE_CURVE ( 'NONE', #13651, #11753, #10704, .T. ) ;
#8747 = ORIENTED_EDGE ( 'NONE', *, *, #998, .F. ) ;
#8748 = DIRECTION ( 'NONE',  ( -1.000000000000000000, 0.000000000000000000, 0.000000000000000000 ) ) ;
#8749 = CARTESIAN_POINT ( 'NONE',  ( 46.00908685603033632, 26.84624452788248661, 44.91496614357595263 ) ) ;
#8750 = CYLINDRICAL_SURFACE ( 'NONE', #65, 4.200000000000000178 ) ;
#8751 = ORIENTED_EDGE ( 'NONE', *, *, #28914, .T. ) ;
#8752 = CARTESIAN_POINT ( 'NONE',  ( 21.09785597605720753, 14.86454579224779948, 47.04930799450052348 ) ) ;
#8753 = CARTESIAN_POINT ( 'NONE',  ( 41.51205063648687599, 11.92558985988973497, 132.0493079945005377 ) ) ;
#8754 = DIRECTION ( 'NONE',  ( 0.4544104193609912468, 5.611869858668455538E-17, 0.8907924397839084296 ) ) ;
#8755 = ORIENTED_EDGE ( 'NONE', *, *, #25817, .T. ) ;
#8756 = DIRECTION ( 'NONE',  ( -1.101824276508909887E-16, 1.000000000000000000, -0.000000000000000000 ) ) ;
#8757 = DIRECTION ( 'NONE',  ( -1.000000000000000000, 0.000000000000000000, 0.000000000000000000 ) ) ;
#8758 = CIRCLE ( 'NONE', #5093, 0.1000000000000006301 ) ;
#8759 = CARTESIAN_POINT ( 'NONE',  ( 21.09785597605720042, 13.06454579224779877, -7.950692005499485404 ) ) ;
#8760 = CARTESIAN_POINT ( 'NONE',  ( 54.17610357928707998, 0.3723237022605491719, -6.641372042216689309 ) ) ;
#8761 = PRODUCT_DEFINITION_SHAPE ( 'NONE', 'NONE',  #32501 ) ;
#8762 = ORIENTED_EDGE ( 'NONE', *, *, #25202, .F. ) ;
#8763 = CARTESIAN_POINT ( 'NONE',  ( -40.28779227465695811, 2.984619150196779369, 58.54930799450051637 ) ) ;
#8764 = VERTEX_POINT ( 'NONE', #15927 ) ;
#8765 = VERTEX_POINT ( 'NONE', #20359 ) ;
#8766 = EDGE_CURVE ( 'NONE', #6406, #21115, #20163, .T. ) ;
#8767 = EDGE_CURVE ( 'NONE', #382, #31093, #17540, .T. ) ;
#8768 = CARTESIAN_POINT ( 'NONE',  ( 49.19517401419062708, 27.58655426599985816, 48.40991706654173754 ) ) ;
#8769 = DIRECTION ( 'NONE',  ( -1.000000000000000000, 0.000000000000000000, 0.000000000000000000 ) ) ;
#8770 = CARTESIAN_POINT ( 'NONE',  ( 21.09785597605720753, -13.37218737171702543, 102.7370144706720225 ) ) ;
#8771 = CIRCLE ( 'NONE', #11919, 0.1000000000000018235 ) ;
#8772 = AXIS2_PLACEMENT_3D ( 'NONE', #25438, #2944, #12975 ) ;
#8773 = VERTEX_POINT ( 'NONE', #18383 ) ;
#8774 = CARTESIAN_POINT ( 'NONE',  ( -34.31970563170438737, 11.92558985988973674, 40.04930799450050216 ) ) ;
#8775 = ORIENTED_EDGE ( 'NONE', *, *, #7721, .T. ) ;
#8776 = CARTESIAN_POINT ( 'NONE',  ( 21.09785597605720753, -5.098646251524523443, 47.04930799450052348 ) ) ;
#8777 = CYLINDRICAL_SURFACE ( 'NONE', #31681, 2.499999999999997335 ) ;
#8778 = CIRCLE ( 'NONE', #20311, 12.62506659569710266 ) ;
#8779 = CARTESIAN_POINT ( 'NONE',  ( -1.498743213250539608, 11.70027025134008625, 98.27232293105659267 ) ) ;
#8780 = ADVANCED_FACE ( 'NONE', ( #2962 ), #32226, .T. ) ;
#8781 = ORIENTED_EDGE ( 'NONE', *, *, #28030, .F. ) ;
#8782 = CARTESIAN_POINT ( 'NONE',  ( 34.41272994418231690, 15.23835801850285776, 47.04930799450052348 ) ) ;
#8783 = DIRECTION ( 'NONE',  ( -1.101824276508909887E-16, 1.000000000000000000, -0.000000000000000000 ) ) ;
#8784 = CARTESIAN_POINT ( 'NONE',  ( 33.46699938050303302, 38.56284415653841791, 47.04930799450051637 ) ) ;
#8785 = CYLINDRICAL_SURFACE ( 'NONE', #31550, 12.62506659569710266 ) ;
#8786 = ORIENTED_EDGE ( 'NONE', *, *, #25047, .F. ) ;
#8787 = DIRECTION ( 'NONE',  ( 1.000000000000000000, 0.000000000000000000, 0.000000000000000000 ) ) ;
#8788 = DIRECTION ( 'NONE',  ( 1.000000000000000000, 0.000000000000000000, 0.000000000000000000 ) ) ;
#8789 = AXIS2_PLACEMENT_3D ( 'NONE', #4574, #22579, #7660 ) ;
#8790 = CARTESIAN_POINT ( 'NONE',  ( 33.71785032049139375, 23.71664230456639899, 47.04930799450051637 ) ) ;
#8791 = DIRECTION ( 'NONE',  ( -1.313185983435984691E-29, 1.000000000000000000, 3.761114140369702165E-15 ) ) ;
#8792 = EDGE_LOOP ( 'NONE', ( #30864, #13839, #24698, #12962 ) ) ;
#8793 = CARTESIAN_POINT ( 'NONE',  ( -40.02667234278197839, 7.000595883235172678, 34.67240784960148403 ) ) ;
#8794 = CARTESIAN_POINT ( 'NONE',  ( -40.68283709841080054, 6.807248601135447608, 34.79766250843303510 ) ) ;
#8795 = ORIENTED_EDGE ( 'NONE', *, *, #17375, .T. ) ;
#8796 = CARTESIAN_POINT ( 'NONE',  ( -40.76967387488526384, 8.530668925462078889, 39.54930799450052348 ) ) ;
#8797 = CYLINDRICAL_SURFACE ( 'NONE', #8540, 12.62506659569710443 ) ;
#8798 = ORIENTED_EDGE ( 'NONE', *, *, #15128, .T. ) ;
#8799 = EDGE_CURVE ( 'NONE', #631, #5527, #31298, .T. ) ;
#8800 = ORIENTED_EDGE ( 'NONE', *, *, #27255, .T. ) ;
#8801 = CIRCLE ( 'NONE', #24002, 0.1250000000000001110 ) ;
#8802 = VECTOR ( 'NONE', #28844, 1000.000000000000000 ) ;
#8803 = EDGE_CURVE ( 'NONE', #13599, #22237, #4452, .T. ) ;
#8804 = EDGE_LOOP ( 'NONE', ( #28884, #13302, #11609, #798 ) ) ;
#8805 = VECTOR ( 'NONE', #16456, 1000.000000000000000 ) ;
#8806 = VECTOR ( 'NONE', #17436, 1000.000000000000000 ) ;
#8807 = EDGE_CURVE ( 'NONE', #10919, #110, #32089, .T. ) ;
#8808 = EDGE_CURVE ( 'NONE', #24330, #9903, #26447, .T. ) ;
#8809 = AXIS2_PLACEMENT_3D ( 'NONE', #16761, #19057, #7089 ) ;
#8810 = ADVANCED_FACE ( 'NONE', ( #2809 ), #20532, .T. ) ;
#8811 = ORIENTED_EDGE ( 'NONE', *, *, #30815, .F. ) ;
#8812 = DIRECTION ( 'NONE',  ( -0.3428121700606640565, -0.6184495258776567805, -0.7071067811865474617 ) ) ;
#8813 = ORIENTED_EDGE ( 'NONE', *, *, #26793, .T. ) ;
#8814 = CARTESIAN_POINT ( 'NONE',  ( 48.24187697582666345, 23.03451764446790051, 47.44084013591611892 ) ) ;
#8815 = CARTESIAN_POINT ( 'NONE',  ( 21.09785597605720753, -5.098646251524523443, 47.04930799450052348 ) ) ;
#8816 = LINE ( 'NONE', #18977, #30055 ) ;
#8817 = CARTESIAN_POINT ( 'NONE',  ( 49.44739180854976013, 28.07786309983298523, 47.17133137409169308 ) ) ;
#8818 = ADVANCED_FACE ( 'NONE', ( #12840 ), #30387, .T. ) ;
#8819 = VERTEX_POINT ( 'NONE', #8383 ) ;
#8820 = AXIS2_PLACEMENT_3D ( 'NONE', #10402, #7945, #16275 ) ;
#8821 = EDGE_LOOP ( 'NONE', ( #1523, #11736, #5553, #31302 ) ) ;
#8822 = LINE ( 'NONE', #31320, #4908 ) ;
#8823 = CIRCLE ( 'NONE', #4119, 12.27641737965285706 ) ;
#8824 = ORIENTED_EDGE ( 'NONE', *, *, #18068, .F. ) ;
#8825 = CARTESIAN_POINT ( 'NONE',  ( 49.23380989124830620, 29.53436827284168231, 47.10497933316898411 ) ) ;
#8826 = AXIS2_PLACEMENT_3D ( 'NONE', #31821, #27665, #7655 ) ;
#8827 = CARTESIAN_POINT ( 'NONE',  ( -40.62190982258952943, 6.851786633712847241, 39.32876805848002277 ) ) ;
#8828 = FACE_OUTER_BOUND ( 'NONE', #16582, .T. ) ;
#8829 = FACE_BOUND ( 'NONE', #23192, .T. ) ;
#8830 = AXIS2_PLACEMENT_3D ( 'NONE', #13653, #6096, #6419 ) ;
#8831 = DIRECTION ( 'NONE',  ( -0.000000000000000000, -1.000000000000000000, -0.000000000000000000 ) ) ;
#8832 = TOROIDAL_SURFACE ( 'NONE', #16157, 12.40141737965284108, 0.1249999999999997918 ) ;
#8833 = DIRECTION ( 'NONE',  ( -0.000000000000000000, -1.000000000000000000, 0.000000000000000000 ) ) ;
#8834 = CYLINDRICAL_SURFACE ( 'NONE', #29536, 31.00000000000000000 ) ;
#8835 = EDGE_LOOP ( 'NONE', ( #246, #30647, #29242, #30986 ) ) ;
#8836 = DIRECTION ( 'NONE',  ( -1.000000000000000000, 0.000000000000000000, 0.000000000000000000 ) ) ;
#8837 = CARTESIAN_POINT ( 'NONE',  ( 33.60959714501833417, 23.65414230456639544, 47.04930799450051637 ) ) ;
#8838 = CARTESIAN_POINT ( 'NONE',  ( 21.09785597605719332, 7.264443105416139801, 47.04930799450051637 ) ) ;
#8839 = AXIS2_PLACEMENT_3D ( 'NONE', #22847, #25794, #5783 ) ;
#8840 = FACE_OUTER_BOUND ( 'NONE', #464, .T. ) ;
#8841 = CARTESIAN_POINT ( 'NONE',  ( 21.09992658989239089, 29.34143805560861296, 47.04930799450051637 ) ) ;
#8842 = EDGE_LOOP ( 'NONE', ( #5592, #17706, #4279, #8091 ) ) ;
#8843 = DIRECTION ( 'NONE',  ( -1.101824276508909887E-16, 1.000000000000000000, -0.000000000000000000 ) ) ;
#8844 = EDGE_CURVE ( 'NONE', #29763, #24923, #27925, .T. ) ;
#8845 = EDGE_LOOP ( 'NONE', ( #15856, #24222, #10962, #355 ) ) ;
#8846 = DIRECTION ( 'NONE',  ( 0.000000000000000000, -0.000000000000000000, -1.000000000000000000 ) ) ;
#8847 = DIRECTION ( 'NONE',  ( -1.101824276508909887E-16, 1.000000000000000000, -0.000000000000000000 ) ) ;
#8848 = EDGE_CURVE ( 'NONE', #22400, #15153, #6032, .T. ) ;
#8849 = ORIENTED_EDGE ( 'NONE', *, *, #24563, .F. ) ;
#8850 = VECTOR ( 'NONE', #19472, 1000.000000000000114 ) ;
#8851 = EDGE_CURVE ( 'NONE', #460, #4474, #10534, .T. ) ;
#8852 = AXIS2_PLACEMENT_3D ( 'NONE', #20431, #20270, #30463 ) ;
#8853 = EDGE_CURVE ( 'NONE', #11099, #11910, #5600, .T. ) ;
#8854 = AXIS2_PLACEMENT_3D ( 'NONE', #10681, #3430, #26070 ) ;
#8855 = VERTEX_POINT ( 'NONE', #1635 ) ;
#8856 = DIRECTION ( 'NONE',  ( 1.234978253042719660E-16, -1.000000000000000000, -1.109335647967047851E-31 ) ) ;
#8857 = FACE_OUTER_BOUND ( 'NONE', #3996, .T. ) ;
#8858 = DIRECTION ( 'NONE',  ( 1.000000000000000000, 0.000000000000000000, 0.000000000000000000 ) ) ;
#8859 = AXIS2_PLACEMENT_3D ( 'NONE', #9173, #4074, #18679 ) ;
#8860 = ORIENTED_EDGE ( 'NONE', *, *, #2780, .T. ) ;
#8861 = DIRECTION ( 'NONE',  ( -1.000000000000000000, 0.000000000000000000, 0.000000000000000000 ) ) ;
#8862 = CARTESIAN_POINT ( 'NONE',  ( -35.76304971539452993, 11.10515806797928207, 41.68537764472188201 ) ) ;
#8863 = CARTESIAN_POINT ( 'NONE',  ( 74.36943655370107820, 1.504766047489258574, 14.48817316672491806 ) ) ;
#8864 = ORIENTED_EDGE ( 'NONE', *, *, #14005, .F. ) ;
#8865 = CARTESIAN_POINT ( 'NONE',  ( 21.09992658989239089, 29.21183152705961206, 47.04930799450051637 ) ) ;
#8866 = ORIENTED_EDGE ( 'NONE', *, *, #16245, .F. ) ;
#8867 = DIRECTION ( 'NONE',  ( 0.000000000000000000, -1.000000000000000000, 0.000000000000000000 ) ) ;
#8868 = CARTESIAN_POINT ( 'NONE',  ( 21.09785597605719332, 77.37245976740706510, 47.04930799450051637 ) ) ;
#8869 = CARTESIAN_POINT ( 'NONE',  ( 45.96182992765471909, 15.77906836436399374, 44.82232689504101586 ) ) ;
#8870 =( NAMED_UNIT ( * ) PLANE_ANGLE_UNIT ( ) SI_UNIT ( $, .RADIAN. ) );
#8871 = ORIENTED_EDGE ( 'NONE', *, *, #18612, .T. ) ;
#8872 = ORIENTED_EDGE ( 'NONE', *, *, #10655, .T. ) ;
#8873 = DIRECTION ( 'NONE',  ( -1.101824276508909887E-16, 1.000000000000000000, -0.000000000000000000 ) ) ;
#8874 = AXIS2_PLACEMENT_3D ( 'NONE', #18623, #26177, #20929 ) ;
#8875 = DIRECTION ( 'NONE',  ( 0.8746197071393927436, -0.4848096202463423876, -1.277302113040827440E-17 ) ) ;
#8876 = CIRCLE ( 'NONE', #3103, 0.1000000000000018235 ) ;
#8877 = DIRECTION ( 'NONE',  ( 0.000000000000000000, 0.000000000000000000, -1.000000000000000000 ) ) ;
#8878 = ORIENTED_EDGE ( 'NONE', *, *, #9003, .F. ) ;
#8879 =( BOUNDED_CURVE ( )  B_SPLINE_CURVE ( 3, ( #6951, #2679, #17932, #3314 ),
 .UNSPECIFIED., .F., .F. ) 
 B_SPLINE_CURVE_WITH_KNOTS ( ( 4, 4 ),
 ( 4.712388980384692339, 6.283185307179584456 ),
 .UNSPECIFIED. ) 
 CURVE ( )  GEOMETRIC_REPRESENTATION_ITEM ( )  RATIONAL_B_SPLINE_CURVE ( ( 1.000000000000000000, 0.8047378541243654926, 0.8047378541243654926, 1.000000000000000000 ) ) 
 REPRESENTATION_ITEM ( '' )  );
#8880 = DIRECTION ( 'NONE',  ( -1.101824276508909887E-16, 1.000000000000000000, -0.000000000000000000 ) ) ;
#8881 = CARTESIAN_POINT ( 'NONE',  ( -40.12089182904525586, 6.795442088152956472, 39.54930799450052348 ) ) ;
#8882 = ORIENTED_EDGE ( 'NONE', *, *, #3589, .F. ) ;
#8883 = DIRECTION ( 'NONE',  ( -0.000000000000000000, -1.000000000000000000, -0.000000000000000000 ) ) ;
#8884 = CARTESIAN_POINT ( 'NONE',  ( 44.77625694075214824, 26.71454579807170759, 48.23360063142255427 ) ) ;
#8885 = AXIS2_PLACEMENT_3D ( 'NONE', #5307, #19575, #12535 ) ;
#8886 = VECTOR ( 'NONE', #25997, 1000.000000000000000 ) ;
#8887 = CARTESIAN_POINT ( 'NONE',  ( 8.474859994195286461, 29.09143805560861296, 47.04930799450051637 ) ) ;
#8888 = CIRCLE ( 'NONE', #13109, 0.09999999999999795164 ) ;
#8889 = AXIS2_PLACEMENT_3D ( 'NONE', #6466, #25995, #31098 ) ;
#8890 = EDGE_CURVE ( 'NONE', #4682, #10687, #12301, .T. ) ;
#8891 = ORIENTED_EDGE ( 'NONE', *, *, #8799, .F. ) ;
#8892 = ADVANCED_FACE ( 'NONE', ( #8705 ), #31834, .T. ) ;
#8893 = CARTESIAN_POINT ( 'NONE',  ( 33.72499318558949710, 23.84143805560861296, 47.04930799450050927 ) ) ;
#8894 = DIRECTION ( 'NONE',  ( -1.000000000000000000, -1.101824276508910010E-16, 0.000000000000000000 ) ) ;
#8895 = CARTESIAN_POINT ( 'NONE',  ( 49.98072202819530219, 28.46753733014355703, 47.19902993264913960 ) ) ;
#8896 = CARTESIAN_POINT ( 'NONE',  ( 46.99023568444673060, 28.62451373492759643, 49.12151524109405898 ) ) ;
#8897 = CIRCLE ( 'NONE', #30957, 0.1250000000000001110 ) ;
#8898 = ORIENTED_EDGE ( 'NONE', *, *, #13583, .F. ) ;
#8899 = CARTESIAN_POINT ( 'NONE',  ( -41.74033427429298371, 15.41509661078533355, 35.54930799450051637 ) ) ;
#8900 = LINE ( 'NONE', #31396, #28314 ) ;
#8901 = CARTESIAN_POINT ( 'NONE',  ( 47.16432553341419975, 22.86454579224779948, 45.05006465737218235 ) ) ;
#8902 = CARTESIAN_POINT ( 'NONE',  ( -40.59290689585612455, 7.518854022824584149, 53.97121529040492760 ) ) ;
#8903 = CARTESIAN_POINT ( 'NONE',  ( 21.09992658989239089, 28.59164230456639544, 47.04930799450051637 ) ) ;
#8904 = AXIS2_PLACEMENT_3D ( 'NONE', #13006, #7750, #23168 ) ;
#8905 = PRODUCT_DEFINITION ( 'UNKNOWN', '', #2422, #11126 ) ;
#8906 = CARTESIAN_POINT ( 'NONE',  ( 21.09785597605720042, -13.88867167006704939, 47.04930799450051637 ) ) ;
#8907 = CIRCLE ( 'NONE', #28912, 2.000000000000001776 ) ;
#8908 = EDGE_LOOP ( 'NONE', ( #7111, #10199, #25674, #30798 ) ) ;
#8909 = CIRCLE ( 'NONE', #22022, 54.21005050633881694 ) ;
#8910 = DIRECTION ( 'NONE',  ( 0.000000000000000000, 0.000000000000000000, -1.000000000000000000 ) ) ;
#8911 = CARTESIAN_POINT ( 'NONE',  ( 45.79384627280941089, 27.07957786121582444, 49.05938063676250493 ) ) ;
#8912 = CARTESIAN_POINT ( 'NONE',  ( 21.09785597605719332, 25.76454579224781227, 47.04930799450051637 ) ) ;
#8913 = CARTESIAN_POINT ( 'NONE',  ( 8.698509210239558698, 29.09164230456639899, 47.04930799450051637 ) ) ;
#8914 = DIRECTION ( 'NONE',  ( 0.000000000000000000, -1.000000000000000000, 0.000000000000000000 ) ) ;
#8915 = ORIENTED_EDGE ( 'NONE', *, *, #24392, .T. ) ;
#8916 = DIRECTION ( 'NONE',  ( 0.000000000000000000, 1.000000000000000000, -0.000000000000000000 ) ) ;
#8917 = CARTESIAN_POINT ( 'NONE',  ( -44.97967447175503253, -5.519741149642646505, 41.28481392491793400 ) ) ;
#8918 = DIRECTION ( 'NONE',  ( -0.5442436726714893203, -1.289618226626749726E-16, 0.8389271868029124501 ) ) ;
#8919 = EDGE_LOOP ( 'NONE', ( #447, #3215, #6310, #14193 ) ) ;
#8920 = DIRECTION ( 'NONE',  ( 0.9612616959383194493, 0.2756373558169974980, 8.795445018804946186E-19 ) ) ;
#8921 = DIRECTION ( 'NONE',  ( 0.000000000000000000, 0.000000000000000000, -1.000000000000000000 ) ) ;
#8922 = DIRECTION ( 'NONE',  ( 0.8746197071393925215, -0.4848096202463429982, -8.676864087101708112E-18 ) ) ;
#8923 = LINE ( 'NONE', #14511, #692 ) ;
#8924 = ORIENTED_EDGE ( 'NONE', *, *, #16040, .T. ) ;
#8925 = CARTESIAN_POINT ( 'NONE',  ( -41.08785830660042393, 9.277514380576532105, 39.40788663826320715 ) ) ;
#8926 = ORIENTED_EDGE ( 'NONE', *, *, #2404, .F. ) ;
#8927 = ADVANCED_FACE ( 'NONE', ( #31679 ), #11278, .T. ) ;
#8928 = CIRCLE ( 'NONE', #2144, 0.2000000000000057288 ) ;
#8929 = ORIENTED_EDGE ( 'NONE', *, *, #16516, .T. ) ;
#8930 = ADVANCED_FACE ( 'NONE', ( #26264 ), #23312, .F. ) ;
#8931 = ADVANCED_FACE ( 'NONE', ( #9353 ), #16480, .T. ) ;
#8932 = TOROIDAL_SURFACE ( 'NONE', #20996, 12.61792373059895311, 0.1249999999999983485 ) ;
#8933 = ADVANCED_FACE ( 'NONE', ( #6084 ), #1297, .T. ) ;
#8934 = EDGE_CURVE ( 'NONE', #19861, #18077, #9159, .T. ) ;
#8935 = VECTOR ( 'NONE', #7828, 1000.000000000000000 ) ;
#8936 = TOROIDAL_SURFACE ( 'NONE', #31478, 1.899999999999999467, 0.1000000000000000056 ) ;
#8937 = AXIS2_PLACEMENT_3D ( 'NONE', #30975, #18004, #30809 ) ;
#8938 = CARTESIAN_POINT ( 'NONE',  ( -40.11286833322907341, 2.887657226147507306, 37.04930799450052348 ) ) ;
#8939 = CARTESIAN_POINT ( 'NONE',  ( 21.09992658989239089, 25.09164230456639899, 47.04930799450051637 ) ) ;
#8940 = DIRECTION ( 'NONE',  ( -1.224646799147353207E-16, -1.349345573449484691E-32, 1.000000000000000000 ) ) ;
#8941 = TOROIDAL_SURFACE ( 'NONE', #10531, 12.40141737965285174, 0.1249999999999993200 ) ;
#8942 = ORIENTED_EDGE ( 'NONE', *, *, #15824, .T. ) ;
#8943 = DIRECTION ( 'NONE',  ( 0.000000000000000000, -0.000000000000000000, -1.000000000000000000 ) ) ;
#8944 = ORIENTED_EDGE ( 'NONE', *, *, #22002, .F. ) ;
#8945 = DIRECTION ( 'NONE',  ( -1.224646799147353207E-16, -1.349345573449484691E-32, 1.000000000000000000 ) ) ;
#8946 = ADVANCED_FACE ( 'NONE', ( #26095 ), #13962, .F. ) ;
#8947 = CARTESIAN_POINT ( 'NONE',  ( -2.052507373444707017, 11.56063108660457495, 98.10909670732513632 ) ) ;
#8948 = ORIENTED_EDGE ( 'NONE', *, *, #23615, .F. ) ;
#8949 = DIRECTION ( 'NONE',  ( -1.101824276508909887E-16, 1.000000000000000000, -0.000000000000000000 ) ) ;
#8950 = DIRECTION ( 'NONE',  ( -1.000000000000000000, 0.000000000000000000, 0.000000000000000000 ) ) ;
#8951 = DIRECTION ( 'NONE',  ( 0.2756373558170082672, -0.9612616959383162296, 1.387778780781436840E-13 ) ) ;
#8952 = CARTESIAN_POINT ( 'NONE',  ( 48.23388202445966755, 25.55087065737811969, 49.27628909396054979 ) ) ;
#8953 = ORIENTED_EDGE ( 'NONE', *, *, #31910, .F. ) ;
#8954 = CARTESIAN_POINT ( 'NONE',  ( 46.47461290750400309, 22.93807716476589675, 45.47175308309371644 ) ) ;
#8955 = DIRECTION ( 'NONE',  ( -1.000000000000000000, 0.000000000000000000, 0.000000000000000000 ) ) ;
#8956 = DIRECTION ( 'NONE',  ( 0.000000000000000000, 0.000000000000000000, 1.000000000000000000 ) ) ;
#8957 = DIRECTION ( 'NONE',  ( -0.8746197071393926326, 0.4848096202463430537, 8.676864087101709653E-18 ) ) ;
#8958 = LINE ( 'NONE', #18952, #10526 ) ;
#8959 = ORIENTED_EDGE ( 'NONE', *, *, #7651, .T. ) ;
#8960 = VECTOR ( 'NONE', #4726, 1000.000000000000227 ) ;
#8961 = CARTESIAN_POINT ( 'NONE',  ( -5.402144023942789808, 13.86454579224779948, 47.04930799450052348 ) ) ;
#8962 = CARTESIAN_POINT ( 'NONE',  ( -40.74228355057324791, 8.435147512834893391, 39.46050754198200394 ) ) ;
#8963 = CIRCLE ( 'NONE', #24688, 39.93581437244897359 ) ;
#8964 = EDGE_LOOP ( 'NONE', ( #10197, #29872, #7267, #15867 ) ) ;
#8965 = VECTOR ( 'NONE', #26664, 1000.000000000000000 ) ;
#8967 = EDGE_CURVE ( 'NONE', #3586, #18781, #11176, .T. ) ;
#8966 = LINE ( 'NONE', #16507, #19823 ) ;
#8968 = AXIS2_PLACEMENT_3D ( 'NONE', #30285, #17799, #27823 ) ;
#8969 = DIRECTION ( 'NONE',  ( -1.101824276508909887E-16, 1.000000000000000000, -0.000000000000000000 ) ) ;
#8970 = ORIENTED_EDGE ( 'NONE', *, *, #8427, .F. ) ;
#8971 = ORIENTED_EDGE ( 'NONE', *, *, #25730, .T. ) ;
#8972 = AXIS2_PLACEMENT_3D ( 'NONE', #17588, #4962, #10057 ) ;
#8973 = ORIENTED_EDGE ( 'NONE', *, *, #30886, .T. ) ;
#8974 = EDGE_CURVE ( 'NONE', #11669, #14845, #24886, .T. ) ;
#8975 = EDGE_CURVE ( 'NONE', #2830, #12487, #5843, .T. ) ;
#8976 = CONICAL_SURFACE ( 'NONE', #5855, 30.00000000000000000, 1.378810109075523149 ) ;
#8977 = CIRCLE ( 'NONE', #28906, 67.36417311134211161 ) ;
#8978 = CARTESIAN_POINT ( 'NONE',  ( -36.18493864628602807, 8.798967949527998655, 60.24930799450051211 ) ) ;
#8979 = VECTOR ( 'NONE', #18634, 1000.000000000000341 ) ;
#8980 = EDGE_LOOP ( 'NONE', ( #4662, #24894, #1785, #31811 ) ) ;
#8981 = DIRECTION ( 'NONE',  ( -0.000000000000000000, -1.000000000000000000, -0.000000000000000000 ) ) ;
#8982 = CYLINDRICAL_SURFACE ( 'NONE', #31912, 12.62506659569710266 ) ;
#8983 = DIRECTION ( 'NONE',  ( -1.000000000000000000, 0.000000000000000000, 0.000000000000000000 ) ) ;
#8984 = CARTESIAN_POINT ( 'NONE',  ( 21.09785597605720042, -13.88867167006704939, 105.7507399849467333 ) ) ;
#8985 = CARTESIAN_POINT ( 'NONE',  ( 48.80717017713595141, 28.71952976649964739, 48.15820438821415195 ) ) ;
#8986 = EDGE_LOOP ( 'NONE', ( #13146, #28919, #5080, #28783 ) ) ;
#8987 = ORIENTED_EDGE ( 'NONE', *, *, #24798, .T. ) ;
#8988 = DIRECTION ( 'NONE',  ( -0.8746197071393790878, 0.4848096202463673676, 1.277302113040196197E-17 ) ) ;
#8989 = AXIS2_PLACEMENT_3D ( 'NONE', #5378, #8162, #13260 ) ;
#8990 = ORIENTED_EDGE ( 'NONE', *, *, #20565, .F. ) ;
#8992 = EDGE_CURVE ( 'NONE', #13785, #25827, #26580, .T. ) ;
#8991 = CARTESIAN_POINT ( 'NONE',  ( 33.72499318558949710, 29.59143805560861296, 47.04930799450051637 ) ) ;
#8993 = DIRECTION ( 'NONE',  ( 0.8746197071393926326, -0.4848096202463430537, -8.676864087101709653E-18 ) ) ;
#8994 = CARTESIAN_POINT ( 'NONE',  ( -40.64264863745309952, 6.822556421825392015, 39.42643144487149698 ) ) ;
#8995 = DIRECTION ( 'NONE',  ( -0.8746197071393926326, 0.4848096202463430537, 8.676864087101709653E-18 ) ) ;
#8996 = CARTESIAN_POINT ( 'NONE',  ( 8.474859994195286461, 28.34184655352419213, 47.04930799450051637 ) ) ;
#8997 = CARTESIAN_POINT ( 'NONE',  ( 48.73570333863616355, 26.42287913140504330, 44.52463952959527660 ) ) ;
#8998 = FACE_OUTER_BOUND ( 'NONE', #25285, .T. ) ;
#8999 = DIRECTION ( 'NONE',  ( -1.101824276508909887E-16, 1.000000000000000000, -0.000000000000000000 ) ) ;
#9000 = EDGE_LOOP ( 'NONE', ( #25350, #3801, #27129, #14058, #5591, #14773 ) ) ;
#9001 = LINE ( 'NONE', #18997, #20782 ) ;
#9003 = EDGE_CURVE ( 'NONE', #16786, #10137, #10744, .T. ) ;
#9002 = DIRECTION ( 'NONE',  ( -1.000000000000000000, -1.101824276508909887E-16, 0.000000000000000000 ) ) ;
#9004 = CARTESIAN_POINT ( 'NONE',  ( 21.09785597605719332, 15.56454579224779877, 47.04930799450051637 ) ) ;
#9005 = EDGE_CURVE ( 'NONE', #6385, #11329, #21723, .T. ) ;
#9006 = CIRCLE ( 'NONE', #27348, 0.8999999999999991340 ) ;
#9007 = CARTESIAN_POINT ( 'NONE',  ( 33.46699938050304013, 24.22145308207319303, 47.04930799450050927 ) ) ;
#9008 = DIRECTION ( 'NONE',  ( -1.000000000000000000, 0.000000000000000000, 0.000000000000000000 ) ) ;
#9009 = VERTEX_POINT ( 'NONE', #24772 ) ;
#9010 = CARTESIAN_POINT ( 'NONE',  ( 21.09785597605719332, -15.93545420775219945, -32.16074251183835031 ) ) ;
#9011 = AXIS2_PLACEMENT_3D ( 'NONE', #29265, #31255, #19075 ) ;
#9012 = ORIENTED_EDGE ( 'NONE', *, *, #28527, .T. ) ;
#9013 = DIRECTION ( 'NONE',  ( -1.000000000000000000, 0.000000000000000000, 0.000000000000000000 ) ) ;
#9014 = CYLINDRICAL_SURFACE ( 'NONE', #28238, 0.1000000000000007272 ) ;
#9015 = ORIENTED_EDGE ( 'NONE', *, *, #3618, .T. ) ;
#9016 = ADVANCED_FACE ( 'NONE', ( #20003 ), #11789, .T. ) ;
#9017 = AXIS2_PLACEMENT_3D ( 'NONE', #5016, #15025, #24533 ) ;
#9018 = ORIENTED_EDGE ( 'NONE', *, *, #522, .F. ) ;
#9019 = CYLINDRICAL_SURFACE ( 'NONE', #31196, 12.48414152717711900 ) ;
#9020 = DIRECTION ( 'NONE',  ( 0.2756373558169974980, -0.9612616959383194493, -1.315048337272770743E-17 ) ) ;
#9021 = DIRECTION ( 'NONE',  ( 1.188208965918165239E-16, 1.880121038077813132E-16, 1.000000000000000000 ) ) ;
#9022 = CIRCLE ( 'NONE', #31572, 0.1250000000000001110 ) ;
#9023 = ORIENTED_EDGE ( 'NONE', *, *, #11646, .F. ) ;
#9024 = CARTESIAN_POINT ( 'NONE',  ( 21.09785597605719332, 30.56454579224779522, 47.04930799450051637 ) ) ;
#9025 = AXIS2_PLACEMENT_3D ( 'NONE', #24095, #1613, #24261 ) ;
#9026 = DIRECTION ( 'NONE',  ( 0.4848096202463645921, 0.8746197071393805311, 0.000000000000000000 ) ) ;
#9027 = CARTESIAN_POINT ( 'NONE',  ( -40.09616233467398416, 6.848043556934189091, 39.27380670015330821 ) ) ;
#9028 = EDGE_CURVE ( 'NONE', #17607, #21751, #20193, .T. ) ;
#9029 = ORIENTED_EDGE ( 'NONE', *, *, #9535, .T. ) ;
#9030 = ORIENTED_EDGE ( 'NONE', *, *, #1578, .F. ) ;
#9031 = EDGE_CURVE ( 'NONE', #26992, #3864, #27537, .T. ) ;
#9032 = CARTESIAN_POINT ( 'NONE',  ( -4.902144023942810236, 30.56554579224779644, 47.04930799450042400 ) ) ;
#9033 = DIRECTION ( 'NONE',  ( 1.234978253042719660E-16, -1.000000000000000000, -1.109335647967047851E-31 ) ) ;
#9034 = FACE_OUTER_BOUND ( 'NONE', #14746, .T. ) ;
#9035 = DIRECTION ( 'NONE',  ( 0.7999999999999990452, -8.326672684688674053E-17, -0.6000000000000014211 ) ) ;
#9036 = ORIENTED_EDGE ( 'NONE', *, *, #15632, .F. ) ;
#9037 = ORIENTED_EDGE ( 'NONE', *, *, #13324, .T. ) ;
#9038 = CARTESIAN_POINT ( 'NONE',  ( 39.08163115802606313, -13.30632128221581034, -5.912965210926095061 ) ) ;
#9039 = CARTESIAN_POINT ( 'NONE',  ( -40.02540636251513462, 2.839176264122873050, 38.54930799450052348 ) ) ;
#9040 = EDGE_CURVE ( 'NONE', #24287, #10826, #24382, .T. ) ;
#9041 = ADVANCED_FACE ( 'NONE', ( #17052 ), #7048, .F. ) ;
#9042 = DIRECTION ( 'NONE',  ( -1.000000000000000000, 0.000000000000000000, 0.000000000000000000 ) ) ;
#9043 = AXIS2_PLACEMENT_3D ( 'NONE', #30043, #17389, #27236 ) ;
#9044 = ORIENTED_EDGE ( 'NONE', *, *, #15849, .T. ) ;
#9045 = DIRECTION ( 'NONE',  ( -1.000000000000000000, 0.000000000000000000, 0.000000000000000000 ) ) ;
#9046 = CARTESIAN_POINT ( 'NONE',  ( 76.34803497562472785, -13.74047052604243468, 28.28865559504965077 ) ) ;
#9047 = AXIS2_PLACEMENT_3D ( 'NONE', #7386, #10008, #12639 ) ;
#9048 = ORIENTED_EDGE ( 'NONE', *, *, #23668, .T. ) ;
#9049 = PLANE ( 'NONE',  #29900 ) ;
#9050 = CARTESIAN_POINT ( 'NONE',  ( 49.41945501136223839, 27.76454579807170830, 45.86501535757901848 ) ) ;
#9051 = AXIS2_PLACEMENT_3D ( 'NONE', #17667, #27687, #2742 ) ;
#9052 = DIRECTION ( 'NONE',  ( -1.000000000000000000, 0.000000000000000000, 0.000000000000000000 ) ) ;
#9053 = CIRCLE ( 'NONE', #13274, 1.000000000000000888 ) ;
#9054 = ORIENTED_EDGE ( 'NONE', *, *, #7494, .F. ) ;
#9055 = CARTESIAN_POINT ( 'NONE',  ( 21.09785597605719332, 30.36454579224777461, 47.04930799450051637 ) ) ;
#9056 = CARTESIAN_POINT ( 'NONE',  ( -40.28779227465695811, 2.984619150196779369, 59.04930799450051637 ) ) ;
#9057 = CARTESIAN_POINT ( 'NONE',  ( 48.23388202445966044, 28.35087065737811685, 49.27628909396054979 ) ) ;
#9058 = CARTESIAN_POINT ( 'NONE',  ( 48.94625023931840246, 28.15784706826092787, 46.10640627770150246 ) ) ;
#9059 = ORIENTED_EDGE ( 'NONE', *, *, #20670, .F. ) ;
#9060 = TOROIDAL_SURFACE ( 'NONE', #3810, 12.40141737965283575, 0.1250000000000000278 ) ;
#9061 = DIRECTION ( 'NONE',  ( -0.2756373558169932791, 0.9612616959383205595, 2.447694389463610066E-31 ) ) ;
#9063 = CARTESIAN_POINT ( 'NONE',  ( 21.09785597605719332, 48.06454579224779877, 44.09837764023711770 ) ) ;
#9062 = AXIS2_PLACEMENT_3D ( 'NONE', #12431, #29992, #27030 ) ;
#9064 = EDGE_CURVE ( 'NONE', #27697, #16912, #10250, .T. ) ;
#9065 = CARTESIAN_POINT ( 'NONE',  ( 72.54343063773337974, 4.323180411458211303, 16.03292188782365812 ) ) ;
#9066 = EDGE_CURVE ( 'NONE', #22928, #229, #24440, .T. ) ;
#9067 = DIRECTION ( 'NONE',  ( -0.000000000000000000, -1.000000000000000000, -0.000000000000000000 ) ) ;
#9068 = CARTESIAN_POINT ( 'NONE',  ( -24.99296521467773147, 14.05098971466613023, 47.04930799450052348 ) ) ;
#9069 = CARTESIAN_POINT ( 'NONE',  ( 48.23388202445966044, 28.22822092656774373, 49.27628909396054979 ) ) ;
#9070 = CARTESIAN_POINT ( 'NONE',  ( -40.59758774925371938, 7.567737757495683226, 38.44930799450052916 ) ) ;
#9071 = VECTOR ( 'NONE', #20429, 1000.000000000000114 ) ;
#9072 = CIRCLE ( 'NONE', #2800, 67.18681090792816235 ) ;
#9073 = CARTESIAN_POINT ( 'NONE',  ( 33.46699938050304013, 28.96183152705961206, 47.04930799450051637 ) ) ;
#9074 = ORIENTED_EDGE ( 'NONE', *, *, #24260, .T. ) ;
#9075 = DIRECTION ( 'NONE',  ( -0.8746197071393926326, 0.4848096202463430537, 8.676864087101709653E-18 ) ) ;
#9076 = CARTESIAN_POINT ( 'NONE',  ( 48.83862994770794330, 29.35457786121581591, 48.17861352429476796 ) ) ;
#9077 = CARTESIAN_POINT ( 'NONE',  ( 81.54661244041565737, -5.936463391120013533, 77.99460177298303165 ) ) ;
#9078 = EDGE_CURVE ( 'NONE', #23287, #14081, #2454, .T. ) ;
#9079 = CARTESIAN_POINT ( 'NONE',  ( 21.09992658989238734, 32.46664230456639899, 47.04930799450051637 ) ) ;
#9080 = FACE_OUTER_BOUND ( 'NONE', #3114, .T. ) ;
#9081 = VERTEX_POINT ( 'NONE', #11978 ) ;
#9082 = CARTESIAN_POINT ( 'NONE',  ( -39.56032632130286686, -5.936105616667935791, 77.94281019529569221 ) ) ;
#9083 = DIRECTION ( 'NONE',  ( -0.4441739386571982307, 0.2110602665713104398, -0.8707256032141232893 ) ) ;
#9084 = DIRECTION ( 'NONE',  ( -0.000000000000000000, -1.000000000000000000, 0.000000000000000000 ) ) ;
#9085 = ORIENTED_EDGE ( 'NONE', *, *, #14998, .F. ) ;
#9086 = DIRECTION ( 'NONE',  ( 0.000000000000000000, 0.000000000000000000, -1.000000000000000000 ) ) ;
#9087 = DIRECTION ( 'NONE',  ( 0.4848096202463637039, 0.8746197071393810862, 0.000000000000000000 ) ) ;
#9088 = DIRECTION ( 'NONE',  ( -0.4848096202463069715, -0.8746197071394126166, 0.000000000000000000 ) ) ;
#9089 = DIRECTION ( 'NONE',  ( -0.8746197071393926326, 0.4848096202463430537, 8.676864087101709653E-18 ) ) ;
#9090 = AXIS2_PLACEMENT_3D ( 'NONE', #440, #30806, #23091 ) ;
#9091 = ORIENTED_EDGE ( 'NONE', *, *, #20814, .T. ) ;
#9092 = DIRECTION ( 'NONE',  ( -1.101824276508909887E-16, 1.000000000000000000, -0.000000000000000000 ) ) ;
#9093 = EDGE_LOOP ( 'NONE', ( #17876, #3245, #7363, #32021 ) ) ;
#9094 = VECTOR ( 'NONE', #27276, 1000.000000000000000 ) ;
#9095 = APPLICATION_CONTEXT ( 'automotive_design' ) ;
#9096 = ORIENTED_EDGE ( 'NONE', *, *, #20338, .T. ) ;
#9097 = AXIS2_PLACEMENT_3D ( 'NONE', #24175, #26482, #26963 ) ;
#9098 =( GEOMETRIC_REPRESENTATION_CONTEXT ( 3 ) GLOBAL_UNCERTAINTY_ASSIGNED_CONTEXT ( ( #13433 ) ) GLOBAL_UNIT_ASSIGNED_CONTEXT ( ( #3258, #6054, #8515 ) ) REPRESENTATION_CONTEXT ( 'NONE', 'WORKASPACE' ) );
#9099 = AXIS2_PLACEMENT_3D ( 'NONE', #4820, #20075, #7616 ) ;
#9100 = AXIS2_PLACEMENT_3D ( 'NONE', #18162, #25882, #28187 ) ;
#9101 = DIRECTION ( 'NONE',  ( -1.101824276508909887E-16, 1.000000000000000000, -0.000000000000000000 ) ) ;
#9102 = FACE_OUTER_BOUND ( 'NONE', #32353, .T. ) ;
#9103 = CARTESIAN_POINT ( 'NONE',  ( -29.73671797196985622, 6.636213240270868674, 76.58164681996676393 ) ) ;
#9104 = LINE ( 'NONE', #24197, #2555 ) ;
#9105 = ORIENTED_EDGE ( 'NONE', *, *, #26631, .T. ) ;
#9106 = CARTESIAN_POINT ( 'NONE',  ( -42.37913764077812573, 15.23192269303852697, 38.44930799450052916 ) ) ;
#9107 = ORIENTED_EDGE ( 'NONE', *, *, #3804, .T. ) ;
#9108 = DIRECTION ( 'NONE',  ( -1.101824276508909887E-16, 1.000000000000000000, -0.000000000000000000 ) ) ;
#9109 = CARTESIAN_POINT ( 'NONE',  ( -3.122697032861657895, 11.19016079752309345, 97.83781872318185435 ) ) ;
#9110 = EDGE_LOOP ( 'NONE', ( #20468, #24707, #31764, #26539 ) ) ;
#9111 = CARTESIAN_POINT ( 'NONE',  ( -43.73393778030726509, 1.305471833569777695, 60.54930799450051637 ) ) ;
#9112 = FACE_OUTER_BOUND ( 'NONE', #9734, .T. ) ;
#9113 = CARTESIAN_POINT ( 'NONE',  ( -42.35386648718987601, 15.27751306094253714, 35.56396816118280668 ) ) ;
#9114 = ORIENTED_EDGE ( 'NONE', *, *, #25213, .F. ) ;
#9115 = DIRECTION ( 'NONE',  ( -0.2756373558169956106, 0.9612616959383197823, 0.000000000000000000 ) ) ;
#9116 = EDGE_CURVE ( 'NONE', #28525, #23085, #3410, .T. ) ;
#9117 = CARTESIAN_POINT ( 'NONE',  ( -40.47970302497625994, 7.463434137431151250, 53.64930799450051779 ) ) ;
#9118 = CARTESIAN_POINT ( 'NONE',  ( 46.33059210211230550, 22.93807716476589675, 45.54522087609679204 ) ) ;
#9119 = DIRECTION ( 'NONE',  ( 0.4151817967359032746, -0.9097384655268496711, -1.287451903529927940E-17 ) ) ;
#9120 = VECTOR ( 'NONE', #22732, 1000.000000000000000 ) ;
#9121 = EDGE_CURVE ( 'NONE', #22576, #23397, #13393, .T. ) ;
#9122 = EDGE_CURVE ( 'NONE', #294, #9753, #2288, .T. ) ;
#9123 = ADVANCED_FACE ( 'NONE', ( #150 ), #16893, .T. ) ;
#9124 = EDGE_LOOP ( 'NONE', ( #23420, #19121, #24753, #5458 ) ) ;
#9125 = DIRECTION ( 'NONE',  ( -1.101824276508909887E-16, 1.000000000000000000, -0.000000000000000000 ) ) ;
#9126 = CARTESIAN_POINT ( 'NONE',  ( 21.09992658989238734, 32.09164230456639899, 47.04930799450051637 ) ) ;
#9127 = ORIENTED_EDGE ( 'NONE', *, *, #25718, .T. ) ;
#9128 = CARTESIAN_POINT ( 'NONE',  ( 21.09992658989239089, 27.21664230456639899, 47.04930799450051637 ) ) ;
#9129 = CARTESIAN_POINT ( 'NONE',  ( 21.09992658989239089, 27.34164230456639544, 47.04930799450051637 ) ) ;
#9130 = ORIENTED_EDGE ( 'NONE', *, *, #10502, .F. ) ;
#9131 = ORIENTED_EDGE ( 'NONE', *, *, #29417, .T. ) ;
#9132 = UNCERTAINTY_MEASURE_WITH_UNIT (LENGTH_MEASURE( 1.000000000000000082E-05 ), #26678, 'distance_accuracy_value', 'NONE');
#9133 = ORIENTED_EDGE ( 'NONE', *, *, #18080, .T. ) ;
#9134 = CIRCLE ( 'NONE', #27486, 12.62506659569710266 ) ;
#9135 = VECTOR ( 'NONE', #26949, 1000.000000000000227 ) ;
#9136 = AXIS2_PLACEMENT_3D ( 'NONE', #25822, #5483, #553 ) ;
#9137 = AXIS2_PLACEMENT_3D ( 'NONE', #15285, #21154, #15591 ) ;
#9138 = PLANE ( 'NONE',  #31864 ) ;
#9139 = EDGE_CURVE ( 'NONE', #5852, #2479, #26912, .T. ) ;
#9140 = ORIENTED_EDGE ( 'NONE', *, *, #25255, .T. ) ;
#9141 = CARTESIAN_POINT ( 'NONE',  ( 21.09992658989238734, 32.46183152705962272, 47.04930799450051637 ) ) ;
#9142 = DIRECTION ( 'NONE',  ( -0.000000000000000000, 1.000000000000000000, -0.000000000000000000 ) ) ;
#9143 = CARTESIAN_POINT ( 'NONE',  ( -39.67555847965937943, 2.645252416024337361, 47.04930799450051637 ) ) ;
#9144 = CARTESIAN_POINT ( 'NONE',  ( 1.597855976057205973, 14.86454579224779948, 47.04930799450052348 ) ) ;
#9145 = CARTESIAN_POINT ( 'NONE',  ( 46.02876340639226527, 29.01119643316631524, 44.95353858666495483 ) ) ;
#9146 = ORIENTED_EDGE ( 'NONE', *, *, #12262, .F. ) ;
#9147 = CARTESIAN_POINT ( 'NONE',  ( -63.90214402394282445, 11.92558985988973674, 54.04930799450053769 ) ) ;
#9148 = ORIENTED_EDGE ( 'NONE', *, *, #10905, .F. ) ;
#9149 = FACE_OUTER_BOUND ( 'NONE', #12416, .T. ) ;
#9150 = ORIENTED_EDGE ( 'NONE', *, *, #18158, .T. ) ;
#9151 = FACE_OUTER_BOUND ( 'NONE', #1534, .T. ) ;
#9152 = CARTESIAN_POINT ( 'NONE',  ( 8.096071960694297687, 15.70210863493540288, 47.04930799450052348 ) ) ;
#9153 = CARTESIAN_POINT ( 'NONE',  ( -40.49379808738640207, 7.146223304872329152, 38.94335650327652587 ) ) ;
#9154 = DIRECTION ( 'NONE',  ( -0.000000000000000000, -1.000000000000000000, 0.000000000000000000 ) ) ;
#9155 = CYLINDRICAL_SURFACE ( 'NONE', #17457, 2.000000000000001776 ) ;
#9156 = EDGE_CURVE ( 'NONE', #10438, #28013, #23337, .T. ) ;
#9157 = EDGE_CURVE ( 'NONE', #12851, #26804, #15997, .T. ) ;
#9158 = CARTESIAN_POINT ( 'NONE',  ( 50.10320668408830613, 27.00621246473837544, 47.20539118556276037 ) ) ;
#9159 = CIRCLE ( 'NONE', #2348, 54.30000000000000426 ) ;
#9160 = EDGE_CURVE ( 'NONE', #10311, #18805, #29545, .T. ) ;
#9161 = FACE_OUTER_BOUND ( 'NONE', #19841, .T. ) ;
#9162 = CARTESIAN_POINT ( 'NONE',  ( -41.02113223168485234, 7.230835263863471418, 34.54930799450052348 ) ) ;
#9163 = TOROIDAL_SURFACE ( 'NONE', #30679, 12.61792373059895844, 0.1249999999999980571 ) ;
#9164 = EDGE_CURVE ( 'NONE', #15510, #19268, #24607, .T. ) ;
#9165 = ORIENTED_EDGE ( 'NONE', *, *, #21785, .F. ) ;
#9166 = DIRECTION ( 'NONE',  ( 1.000000000000000000, 0.000000000000000000, 0.000000000000000000 ) ) ;
#9167 = DIRECTION ( 'NONE',  ( -1.101824276508909887E-16, 1.000000000000000000, -0.000000000000000000 ) ) ;
#9168 = VECTOR ( 'NONE', #17170, 1000.000000000000114 ) ;
#9169 = DIRECTION ( 'NONE',  ( 0.8746197071393926326, -0.4848096202463430537, -8.676864087101709653E-18 ) ) ;
#9170 = VECTOR ( 'NONE', #332, 1000.000000000000000 ) ;
#9171 = CIRCLE ( 'NONE', #19655, 0.1000000000000018235 ) ;
#9172 = CARTESIAN_POINT ( 'NONE',  ( 47.99481790889201704, 22.99884124225578930, 45.95397743221676023 ) ) ;
#9173 = CARTESIAN_POINT ( 'NONE',  ( 21.09992658989239089, 25.59164230456639899, 47.04930799450051637 ) ) ;
#9174 = ORIENTED_EDGE ( 'NONE', *, *, #31123, .T. ) ;
#9175 = CARTESIAN_POINT ( 'NONE',  ( -12.40214402394279603, -5.098646251524523443, 47.04930799450052348 ) ) ;
#9176 = ORIENTED_EDGE ( 'NONE', *, *, #17454, .F. ) ;
#9177 = CYLINDRICAL_SURFACE ( 'NONE', #21454, 12.36707279061065101 ) ;
#9178 = CARTESIAN_POINT ( 'NONE',  ( 21.09785597605720753, -5.098646251524523443, 47.04930799450052348 ) ) ;
#9179 = EDGE_LOOP ( 'NONE', ( #30866, #27654 ) ) ;
#9180 = EDGE_LOOP ( 'NONE', ( #444, #31837, #11917, #28031 ) ) ;
#9181 = AXIS2_PLACEMENT_3D ( 'NONE', #27075, #12414, #21975 ) ;
#9182 = LINE ( 'NONE', #21806, #20175 ) ;
#9183 = EDGE_CURVE ( 'NONE', #25724, #5204, #28045, .T. ) ;
#9184 = DIRECTION ( 'NONE',  ( 0.000000000000000000, 1.000000000000000000, 0.000000000000000000 ) ) ;
#9186 = DIRECTION ( 'NONE',  ( -1.101824276508909887E-16, 1.000000000000000000, -0.000000000000000000 ) ) ;
#9185 = CIRCLE ( 'NONE', #8144, 12.62506659569710266 ) ;
#9187 = ADVANCED_FACE ( 'NONE', ( #23117 ), #283, .T. ) ;
#9188 = CONICAL_SURFACE ( 'NONE', #21759, 54.55130244989821620, 1.291543646475813212 ) ;
#9189 = CIRCLE ( 'NONE', #26477, 1.142135311067127512 ) ;
#9190 = VERTEX_POINT ( 'NONE', #28207 ) ;
#9191 = DIRECTION ( 'NONE',  ( 0.000000000000000000, 0.000000000000000000, 1.000000000000000000 ) ) ;
#9192 = CARTESIAN_POINT ( 'NONE',  ( -35.51631071586560751, 11.48547954296073570, 41.32792022444346003 ) ) ;
#9193 = CARTESIAN_POINT ( 'NONE',  ( -40.11085926462317275, 6.816553873983420608, 39.35917588466254813 ) ) ;
#9194 = ORIENTED_EDGE ( 'NONE', *, *, #17037, .T. ) ;
#9195 = CARTESIAN_POINT ( 'NONE',  ( 45.84097905237065618, 22.80400562401890241, 48.98672734302541443 ) ) ;
#9196 = VERTEX_POINT ( 'NONE', #15729 ) ;
#9197 = FACE_OUTER_BOUND ( 'NONE', #9372, .T. ) ;
#9198 = CARTESIAN_POINT ( 'NONE',  ( 33.46699938050304013, 30.21183152705961561, 47.04930799450051637 ) ) ;
#9199 = LINE ( 'NONE', #24291, #39 ) ;
#9200 = EDGE_CURVE ( 'NONE', #10938, #25889, #17569, .T. ) ;
#9201 = SURFACE_SIDE_STYLE ('',( #6903 ) ) ;
#9202 = VERTEX_POINT ( 'NONE', #307 ) ;
#9203 = ORIENTED_EDGE ( 'NONE', *, *, #24975, .F. ) ;
#9204 = DIRECTION ( 'NONE',  ( -1.101824276508909887E-16, 1.000000000000000000, -0.000000000000000000 ) ) ;
#9205 = CARTESIAN_POINT ( 'NONE',  ( 21.09785597605719332, 30.36454579224777461, 47.04930799450051637 ) ) ;
#9206 = DIRECTION ( 'NONE',  ( 0.000000000000000000, 0.000000000000000000, -1.000000000000000000 ) ) ;
#9207 = CIRCLE ( 'NONE', #8166, 43.50000000000000000 ) ;
#9208 = ORIENTED_EDGE ( 'NONE', *, *, #5577, .F. ) ;
#9209 = CARTESIAN_POINT ( 'NONE',  ( -12.09164073932641870, -4.535950511381766859, -9.747560124061404707 ) ) ;
#9210 = CARTESIAN_POINT ( 'NONE',  ( 46.89984767728657999, -13.74047052604243291, -5.284252768999646577 ) ) ;
#9211 = ORIENTED_EDGE ( 'NONE', *, *, #9674, .F. ) ;
#9212 = LINE ( 'NONE', #32193, #7785 ) ;
#9213 = AXIS2_PLACEMENT_3D ( 'NONE', #27940, #22842, #22191 ) ;
#9214 = CARTESIAN_POINT ( 'NONE',  ( -63.90214402394282445, 11.92558985988973674, 40.04930799450050216 ) ) ;
#9215 = CIRCLE ( 'NONE', #29127, 0.1250000000000001110 ) ;
#9216 = EDGE_CURVE ( 'NONE', #13562, #19299, #24915, .T. ) ;
#9217 = ADVANCED_FACE ( 'NONE', ( #25901 ), #3081, .T. ) ;
#9218 = VECTOR ( 'NONE', #21647, 1000.000000000000000 ) ;
#9219 = EDGE_LOOP ( 'NONE', ( #15712, #7550, #24489, #12452 ) ) ;
#9220 = CARTESIAN_POINT ( 'NONE',  ( 21.09785597605719332, 11.78014697381582643, 102.6448323059792358 ) ) ;
#9221 = DIRECTION ( 'NONE',  ( -0.4151817967359235362, 0.9097384655268405673, 0.000000000000000000 ) ) ;
#9222 = ADVANCED_FACE ( 'NONE', ( #15897 ), #9707, .T. ) ;
#9223 = CARTESIAN_POINT ( 'NONE',  ( 33.50134396954526750, 24.84164230456639544, 47.04930799450051637 ) ) ;
#9224 = CARTESIAN_POINT ( 'NONE',  ( 45.35708200440645044, 29.09118040159425789, 45.92000246470679770 ) ) ;
#9225 = EDGE_CURVE ( 'NONE', #17298, #26367, #30351, .T. ) ;
#9226 = VERTEX_POINT ( 'NONE', #13290 ) ;
#9227 = EDGE_CURVE ( 'NONE', #3003, #23526, #20165, .T. ) ;
#9228 = DIRECTION ( 'NONE',  ( -0.000000000000000000, -1.000000000000000000, -0.000000000000000000 ) ) ;
#9229 = DIRECTION ( 'NONE',  ( 0.000000000000000000, 0.000000000000000000, 1.000000000000000000 ) ) ;
#9230 = AXIS2_PLACEMENT_3D ( 'NONE', #12160, #32345, #7228 ) ;
#9231 = CARTESIAN_POINT ( 'NONE',  ( 54.78651577895161040, -1.820484904611813670, -6.751011824304275599 ) ) ;
#9232 = COLOUR_RGB ( '',0.7921568627450980005, 0.8196078431372548767, 0.9333333333333333481 ) ;
#9233 = PLANE ( 'NONE',  #16534 ) ;
#9234 = DIRECTION ( 'NONE',  ( 1.000000000000000000, 0.000000000000000000, 0.000000000000000000 ) ) ;
#9235 = CARTESIAN_POINT ( 'NONE',  ( 17.28711060612851469, -13.74047052604243468, 105.2732083934160840 ) ) ;
#9236 = CARTESIAN_POINT ( 'NONE',  ( -39.58809650894544774, 2.596771453999702661, 47.04930799450051637 ) ) ;
#9237 = DIRECTION ( 'NONE',  ( -0.4848096202463636484, -0.8746197071393810862, 0.000000000000000000 ) ) ;
#9238 = EDGE_CURVE ( 'NONE', #180, #10311, #13120, .T. ) ;
#9239 = ORIENTED_EDGE ( 'NONE', *, *, #7039, .F. ) ;
#9240 = LINE ( 'NONE', #19228, #14984 ) ;
#9241 = CARTESIAN_POINT ( 'NONE',  ( -40.42362386230406912, 8.537703822322061598, 34.55508635502626902 ) ) ;
#9242 = CARTESIAN_POINT ( 'NONE',  ( -29.95217301285917699, 11.55131472896195710, 23.86477200840625912 ) ) ;
#9243 = AXIS2_PLACEMENT_3D ( 'NONE', #8938, #3853, #32081 ) ;
#9244 = CARTESIAN_POINT ( 'NONE',  ( 21.09992658989238734, 38.56284415653841791, 47.04930799450051637 ) ) ;
#9245 = EDGE_LOOP ( 'NONE', ( #20790, #31187, #32307, #29361 ) ) ;
#9246 = LINE ( 'NONE', #9408, #19213 ) ;
#9247 = CARTESIAN_POINT ( 'NONE',  ( 47.37433252627624825, 14.98691807112499141, 47.59129209129815763 ) ) ;
#9248 = CARTESIAN_POINT ( 'NONE',  ( -43.64647580959332629, 1.256990871545142774, 53.64930799450051779 ) ) ;
#9249 = ORIENTED_EDGE ( 'NONE', *, *, #19013, .F. ) ;
#9250 = VERTEX_POINT ( 'NONE', #17697 ) ;
#9251 = DIRECTION ( 'NONE',  ( 0.000000000000000000, -1.000000000000000000, 0.000000000000000000 ) ) ;
#9252 = CARTESIAN_POINT ( 'NONE',  ( -39.57405207560572791, -5.936374393131169214, 77.91251232197767251 ) ) ;
#9253 = CARTESIAN_POINT ( 'NONE',  ( 21.09992658989239089, 27.34184655352419568, 47.04930799450051637 ) ) ;
#9254 = CARTESIAN_POINT ( 'NONE',  ( 47.05339576314583638, 22.89977464660286444, 45.18578914680342251 ) ) ;
#9255 = ORIENTED_EDGE ( 'NONE', *, *, #26298, .F. ) ;
#9256 = CARTESIAN_POINT ( 'NONE',  ( 72.46983671362423252, 10.06999148276586453, 20.80324894526496138 ) ) ;
#9257 = EDGE_LOOP ( 'NONE', ( #30820, #14550, #412, #20656 ) ) ;
#9258 = EDGE_CURVE ( 'NONE', #28679, #10039, #7869, .T. ) ;
#9259 = AXIS2_PLACEMENT_3D ( 'NONE', #6380, #26886, #8836 ) ;
#9260 = EDGE_CURVE ( 'NONE', #5063, #19350, #6641, .T. ) ;
#9261 = ORIENTED_EDGE ( 'NONE', *, *, #11523, .T. ) ;
#9262 = CARTESIAN_POINT ( 'NONE',  ( 52.12082631206856576, -5.937449718911894436, 107.4212530892143889 ) ) ;
#9263 = EDGE_CURVE ( 'NONE', #6715, #11279, #18179, .T. ) ;
#9264 = CIRCLE ( 'NONE', #360, 0.1249999999999931721 ) ;
#9265 = ADVANCED_FACE ( 'NONE', ( #5891 ), #5404, .F. ) ;
#9266 =( BOUNDED_CURVE ( )  B_SPLINE_CURVE ( 3, ( #25594, #15105, #27417, #5421 ),
 .UNSPECIFIED., .F., .F. ) 
 B_SPLINE_CURVE_WITH_KNOTS ( ( 4, 4 ),
 ( 5.497787143782109531, 6.283185307179586232 ),
 .UNSPECIFIED. ) 
 CURVE ( )  GEOMETRIC_REPRESENTATION_ITEM ( )  RATIONAL_B_SPLINE_CURVE ( ( 1.000000000000000000, 0.9492530216741874582, 0.9492530216741874582, 1.000000000000000000 ) ) 
 REPRESENTATION_ITEM ( '' )  );
#9267 = CARTESIAN_POINT ( 'NONE',  ( 21.09992658989238734, 38.56284415653841791, 47.04930799450051637 ) ) ;
#9268 = CARTESIAN_POINT ( 'NONE',  ( -31.51145727905382188, 0.7402364505617297086, 79.96531199145222502 ) ) ;
#9269 = ORIENTED_EDGE ( 'NONE', *, *, #29204, .T. ) ;
#9270 = DIRECTION ( 'NONE',  ( 0.2756373558169954441, -0.9612616959383198934, 1.479773560108263451E-16 ) ) ;
#9271 = ORIENTED_EDGE ( 'NONE', *, *, #32101, .T. ) ;
#9272 = CARTESIAN_POINT ( 'NONE',  ( 21.09785597605719332, 47.94190058235918173, 47.04930799450051637 ) ) ;
#9273 = DIRECTION ( 'NONE',  ( 0.4848096202463655358, 0.8746197071393799760, 0.000000000000000000 ) ) ;
#9274 = CARTESIAN_POINT ( 'NONE',  ( 8.732853799281732776, 24.97145308207319303, 47.04930799450051637 ) ) ;
#9275 = ORIENTED_EDGE ( 'NONE', *, *, #25092, .F. ) ;
#9276 = DIRECTION ( 'NONE',  ( -1.000000000000000000, 0.000000000000000000, 0.000000000000000000 ) ) ;
#9277 = DIRECTION ( 'NONE',  ( -0.000000000000000000, -1.000000000000000000, 0.000000000000000000 ) ) ;
#9279 = FACE_OUTER_BOUND ( 'NONE', #26566, .T. ) ;
#9278 = CIRCLE ( 'NONE', #27630, 47.05803085792211249 ) ;
#9280 = LINE ( 'NONE', #14374, #115 ) ;
#9281 = DIRECTION ( 'NONE',  ( -1.000000000000000000, -1.101824276508909887E-16, 0.000000000000000000 ) ) ;
#9282 = CARTESIAN_POINT ( 'NONE',  ( -40.13663441551143762, 7.212672898651366182, 35.13832588636704912 ) ) ;
#9283 = DIRECTION ( 'NONE',  ( -1.000000000000000000, 0.000000000000000000, 0.000000000000000000 ) ) ;
#9284 = EDGE_LOOP ( 'NONE', ( #31778, #9991, #23579, #8312 ) ) ;
#9285 = DIRECTION ( 'NONE',  ( -0.000000000000000000, 1.000000000000000000, -0.000000000000000000 ) ) ;
#9286 = CARTESIAN_POINT ( 'NONE',  ( 33.50134396954524618, 26.84164230456639899, 47.04930799450051637 ) ) ;
#9287 = ORIENTED_EDGE ( 'NONE', *, *, #7783, .T. ) ;
#9288 = CARTESIAN_POINT ( 'NONE',  ( -43.35833523721898075, -3.935454207752190126, 42.04930799450051637 ) ) ;
#9289 = B_SPLINE_CURVE_WITH_KNOTS ( 'NONE', 3,
 ( #21665, #11341, #21330, #14132 ),
 .UNSPECIFIED., .F., .F.,
 ( 4, 4 ),
 ( 0.07446322096370984467, 0.09032397578024474460 ),
 .UNSPECIFIED. ) ;
#9290 = DIRECTION ( 'NONE',  ( -1.101824276508909887E-16, 1.000000000000000000, -0.000000000000000000 ) ) ;
#9291 = EDGE_LOOP ( 'NONE', ( #24511, #16194, #27320, #25913 ) ) ;
#9292 = ORIENTED_EDGE ( 'NONE', *, *, #300, .T. ) ;
#9293 = CIRCLE ( 'NONE', #18716, 12.36707279061065101 ) ;
#9294 = ORIENTED_EDGE ( 'NONE', *, *, #14679, .F. ) ;
#9295 = AXIS2_PLACEMENT_3D ( 'NONE', #6755, #31384, #16590 ) ;
#9296 = ADVANCED_FACE ( 'NONE', ( #28047 ), #29094, .T. ) ;
#9297 = ADVANCED_FACE ( 'NONE', ( #25576 ), #1589, .T. ) ;
#9298 = AXIS2_PLACEMENT_3D ( 'NONE', #18434, #13847, #28466 ) ;
#9299 = DIRECTION ( 'NONE',  ( 0.4848096202463636484, 0.8746197071393810862, 0.000000000000000000 ) ) ;
#9300 = ORIENTED_EDGE ( 'NONE', *, *, #12086, .F. ) ;
#9301 = CIRCLE ( 'NONE', #13001, 0.04999999999999768518 ) ;
#9302 = EDGE_LOOP ( 'NONE', ( #4634, #22631, #7439, #27437 ) ) ;
#9303 = CARTESIAN_POINT ( 'NONE',  ( -42.92119432306954252, 16.03391241267916811, 37.04930799450052348 ) ) ;
#9304 = CARTESIAN_POINT ( 'NONE',  ( 47.86364407361583062, 22.99884124225578930, 45.86888002329718717 ) ) ;
#9305 = FACE_OUTER_BOUND ( 'NONE', #16809, .T. ) ;
#9306 = DIRECTION ( 'NONE',  ( 0.000000000000000000, 0.000000000000000000, -1.000000000000000000 ) ) ;
#9307 = CARTESIAN_POINT ( 'NONE',  ( 44.74832014356462651, 27.02786309983298452, 46.92728461490987257 ) ) ;
#9308 = ORIENTED_EDGE ( 'NONE', *, *, #9535, .F. ) ;
#9309 = DIRECTION ( 'NONE',  ( -0.2756373558169958327, 0.9612616959383198934, 0.000000000000000000 ) ) ;
#9310 = ORIENTED_EDGE ( 'NONE', *, *, #12133, .F. ) ;
#9311 = DIRECTION ( 'NONE',  ( -1.000000000000000000, -1.101824276508909887E-16, 0.000000000000000000 ) ) ;
#9312 = ORIENTED_EDGE ( 'NONE', *, *, #5943, .F. ) ;
#9313 = CARTESIAN_POINT ( 'NONE',  ( 49.18002788330665709, 29.51722998668063624, 47.59998504452501322 ) ) ;
#9314 = CARTESIAN_POINT ( 'NONE',  ( 21.09785597605719332, 28.56454579224779877, 47.04930799450051637 ) ) ;
#9315 = CARTESIAN_POINT ( 'NONE',  ( -40.56960242289655838, 7.470141326142095473, 38.67132538937698882 ) ) ;
#9316 = CARTESIAN_POINT ( 'NONE',  ( -40.68572042366827191, 6.804601513393670587, 39.33474082486971213 ) ) ;
#9317 = CARTESIAN_POINT ( 'NONE',  ( -40.51045226066063520, 7.589116544599141534, 60.22001867261916885 ) ) ;
#9318 = CARTESIAN_POINT ( 'NONE',  ( 47.23302798462060537, 27.88121246473837544, 44.44659793406428605 ) ) ;
#9319 = FACE_OUTER_BOUND ( 'NONE', #4377, .T. ) ;
#9320 = DIRECTION ( 'NONE',  ( 0.4544104193609908027, 5.611869858668450607E-17, 0.8907924397839086517 ) ) ;
#9321 = ORIENTED_EDGE ( 'NONE', *, *, #26227, .T. ) ;
#9322 = CARTESIAN_POINT ( 'NONE',  ( -36.37788479535792163, 9.471851136684824368, 59.54930799450050927 ) ) ;
#9323 = FACE_OUTER_BOUND ( 'NONE', #14434, .T. ) ;
#9324 = AXIS2_PLACEMENT_3D ( 'NONE', #9010, #16704, #4408 ) ;
#9325 = DIRECTION ( 'NONE',  ( 0.000000000000000000, 0.000000000000000000, -1.000000000000000000 ) ) ;
#9326 = AXIS2_PLACEMENT_3D ( 'NONE', #15203, #32118, #22409 ) ;
#9327 = DIRECTION ( 'NONE',  ( 0.000000000000000000, 0.7071067811865487940, 0.7071067811865463515 ) ) ;
#9328 = CARTESIAN_POINT ( 'NONE',  ( 8.732853799281732776, 32.46183152705962272, 47.04930799450051637 ) ) ;
#9329 = ORIENTED_EDGE ( 'NONE', *, *, #1393, .T. ) ;
#9330 = CYLINDRICAL_SURFACE ( 'NONE', #11428, 12.62506659569710443 ) ;
#9331 = TOROIDAL_SURFACE ( 'NONE', #10398, 12.61792373059893535, 0.1249999999999994033 ) ;
#9332 = ORIENTED_EDGE ( 'NONE', *, *, #32492, .F. ) ;
#9333 = CARTESIAN_POINT ( 'NONE',  ( 21.09992658989239089, 30.34184655352422411, 47.04930799450051637 ) ) ;
#9334 = CYLINDRICAL_SURFACE ( 'NONE', #29838, 0.1000000000000028644 ) ;
#9335 = CIRCLE ( 'NONE', #6729, 0.1000000000000008243 ) ;
#9336 = VERTEX_POINT ( 'NONE', #13594 ) ;
#9337 = EDGE_CURVE ( 'NONE', #22133, #23145, #14958, .T. ) ;
#9338 = ADVANCED_FACE ( 'NONE', ( #23599 ), #11809, .T. ) ;
#9339 = ADVANCED_FACE ( 'NONE', ( #26700 ), #26384, .F. ) ;
#9340 = ORIENTED_EDGE ( 'NONE', *, *, #30110, .F. ) ;
#9341 = EDGE_CURVE ( 'NONE', #12012, #25631, #1844, .T. ) ;
#9342 = EDGE_CURVE ( 'NONE', #16815, #12159, #8667, .T. ) ;
#9343 = FACE_OUTER_BOUND ( 'NONE', #13922, .T. ) ;
#9344 = TOROIDAL_SURFACE ( 'NONE', #18764, 12.40141737965285706, 0.1250000000000007494 ) ;
#9345 = DIRECTION ( 'NONE',  ( -1.224646799147353207E-16, -1.349345573449484691E-32, 1.000000000000000000 ) ) ;
#9346 = FACE_OUTER_BOUND ( 'NONE', #7738, .T. ) ;
#9347 = AXIS2_PLACEMENT_3D ( 'NONE', #29459, #6968, #10533 ) ;
#9348 = AXIS2_PLACEMENT_3D ( 'NONE', #17404, #15583, #22482 ) ;
#9349 = ORIENTED_EDGE ( 'NONE', *, *, #28269, .F. ) ;
#9350 = CIRCLE ( 'NONE', #6721, 2.500000000000002220 ) ;
#9351 = CARTESIAN_POINT ( 'NONE',  ( -40.61530068986830599, 9.443487761709571160, 39.52001867261917312 ) ) ;
#9352 = AXIS2_PLACEMENT_3D ( 'NONE', #3062, #30982, #10644 ) ;
#9353 = FACE_OUTER_BOUND ( 'NONE', #23955, .T. ) ;
#9354 = FACE_OUTER_BOUND ( 'NONE', #31339, .T. ) ;
#9355 = VERTEX_POINT ( 'NONE', #10974 ) ;
#9356 = VERTEX_POINT ( 'NONE', #26542 ) ;
#9357 = CARTESIAN_POINT ( 'NONE',  ( 45.33322567907855927, 22.86454579224779948, 47.99136533781562974 ) ) ;
#9358 = ORIENTED_EDGE ( 'NONE', *, *, #10555, .T. ) ;
#9359 = CIRCLE ( 'NONE', #13029, 0.09999999999999921452 ) ;
#9360 = DIRECTION ( 'NONE',  ( -0.000000000000000000, -1.000000000000000000, 0.000000000000000000 ) ) ;
#9361 = DIRECTION ( 'NONE',  ( -1.101824276508909887E-16, 1.000000000000000000, -0.000000000000000000 ) ) ;
#9362 = CARTESIAN_POINT ( 'NONE',  ( 21.09785597605718976, -13.68121847681060643, -10.98357976667645808 ) ) ;
#9363 = ADVANCED_FACE ( 'NONE', ( #20968 ), #12880, .T. ) ;
#9364 = VERTEX_POINT ( 'NONE', #30998 ) ;
#9365 = VERTEX_POINT ( 'NONE', #1260 ) ;
#9366 = CARTESIAN_POINT ( 'NONE',  ( 63.14652337230383949, -13.30632128221581212, 10.16668169048476855 ) ) ;
#9367 = CARTESIAN_POINT ( 'NONE',  ( 21.09785597605720042, -16.93545420775220123, -31.45069200549948363 ) ) ;
#9368 = LINE ( 'NONE', #2145, #4147 ) ;
#9369 = ORIENTED_EDGE ( 'NONE', *, *, #5434, .F. ) ;
#9370 = CARTESIAN_POINT ( 'NONE',  ( -10.93321727514354968, 2.565965067347318662, -5.856419385355146723 ) ) ;
#9371 = CARTESIAN_POINT ( 'NONE',  ( -40.18454328187963398, 7.548069831825862330, 60.44930799450051495 ) ) ;
#9372 = EDGE_LOOP ( 'NONE', ( #25606, #23426, #55, #2646 ) ) ;
#9373 = CARTESIAN_POINT ( 'NONE',  ( 21.09992658989238734, 38.56284415653841791, 47.04930799450051637 ) ) ;
#9374 = CARTESIAN_POINT ( 'NONE',  ( 49.41945501136223839, 26.36454579807171328, 45.86501535757901848 ) ) ;
#9375 = EDGE_CURVE ( 'NONE', #23989, #23397, #29645, .T. ) ;
#9376 = VECTOR ( 'NONE', #9142, 1000.000000000000000 ) ;
#9377 = CIRCLE ( 'NONE', #23005, 12.36707279061065101 ) ;
#9378 = CARTESIAN_POINT ( 'NONE',  ( -40.11598084786749752, 7.671759737001394797, 53.64930799450051779 ) ) ;
#9379 = CIRCLE ( 'NONE', #17736, 0.2999999999999999334 ) ;
#9380 = ORIENTED_EDGE ( 'NONE', *, *, #9448, .T. ) ;
#9381 = CARTESIAN_POINT ( 'NONE',  ( 21.09992658989239089, 23.84143805560861296, 47.04930799450051637 ) ) ;
#9382 = ADVANCED_FACE ( 'NONE', ( #16048 ), #30705, .T. ) ;
#9383 = DIRECTION ( 'NONE',  ( 0.000000000000000000, 0.000000000000000000, -1.000000000000000000 ) ) ;
#9384 = CARTESIAN_POINT ( 'NONE',  ( 21.09785597605719332, 13.74476430820393347, 47.04930799450051637 ) ) ;
#9385 = CARTESIAN_POINT ( 'NONE',  ( 48.18662509608405031, 29.38284706826092574, 49.18364984542562013 ) ) ;
#9386 = ORIENTED_EDGE ( 'NONE', *, *, #27106, .F. ) ;
#9387 = CYLINDRICAL_SURFACE ( 'NONE', #16991, 2.499999999999997335 ) ;
#9388 = CARTESIAN_POINT ( 'NONE',  ( 8.732853799281732776, 38.56284415653841791, 47.04930799450051637 ) ) ;
#9389 = CARTESIAN_POINT ( 'NONE',  ( 48.47851147111797587, 9.126991894476594425, -3.410444923187272881 ) ) ;
#9390 = B_SPLINE_CURVE_WITH_KNOTS ( 'NONE', 3,
 ( #12690, #22678, #17747, #5291, #15297, #2817 ),
 .UNSPECIFIED., .F., .F.,
 ( 4, 2, 4 ),
 ( 0.000000000000000000, 0.5000000000000000000, 1.000000000000000000 ),
 .UNSPECIFIED. ) ;
#9391 = AXIS2_PLACEMENT_3D ( 'NONE', #27520, #17164, #15049 ) ;
#9392 = AXIS2_PLACEMENT_3D ( 'NONE', #25839, #20753, #17643 ) ;
#9393 = DIRECTION ( 'NONE',  ( -1.000000000000000000, 0.000000000000000000, 0.000000000000000000 ) ) ;
#9394 = CARTESIAN_POINT ( 'NONE',  ( 47.09785597605719687, 15.77906836436399374, 47.04930799450078638 ) ) ;
#9395 = CARTESIAN_POINT ( 'NONE',  ( -43.38408989745150990, 1.111547985471240008, 53.64930799450051779 ) ) ;
#9396 = CARTESIAN_POINT ( 'NONE',  ( -36.75072804420383932, -13.74047052604243646, 39.42791148283190950 ) ) ;
#9397 = DIRECTION ( 'NONE',  ( -1.224646799147353207E-16, -1.349345573449484691E-32, 1.000000000000000000 ) ) ;
#9398 = ADVANCED_FACE ( 'NONE', ( #28851 ), #24930, .T. ) ;
#9399 = FACE_OUTER_BOUND ( 'NONE', #31772, .T. ) ;
#9400 = ORIENTED_EDGE ( 'NONE', *, *, #12686, .T. ) ;
#9401 = CARTESIAN_POINT ( 'NONE',  ( 45.47421713364555274, 22.88065857334294861, 45.99599230681428708 ) ) ;
#9402 = CYLINDRICAL_SURFACE ( 'NONE', #26635, 0.1000000000000018235 ) ;
#9403 = EDGE_CURVE ( 'NONE', #31921, #30851, #9207, .T. ) ;
#9404 = CARTESIAN_POINT ( 'NONE',  ( -29.45605141075584754, 10.51278159275453739, 21.50388707020794499 ) ) ;
#9405 = TOROIDAL_SURFACE ( 'NONE', #11482, 12.40141737965279667, 0.1249999999999991951 ) ;
#9406 = DIRECTION ( 'NONE',  ( -0.9612616959383194493, -0.2756373558169972759, -8.795445018804907668E-19 ) ) ;
#9407 = EDGE_LOOP ( 'NONE', ( #10607, #10486, #11875, #25472 ) ) ;
#9408 = CARTESIAN_POINT ( 'NONE',  ( -33.20214402394279318, -5.098646251524523443, 47.04930799450052348 ) ) ;
#9409 = VECTOR ( 'NONE', #17855, 1000.000000000000114 ) ;
#9410 = DIRECTION ( 'NONE',  ( -0.09590798424311161585, -0.9774730502038649904, -0.1880108898004995421 ) ) ;
#9411 = CARTESIAN_POINT ( 'NONE',  ( 21.09992658989238734, 32.34164230456639899, 47.04930799450051637 ) ) ;
#9412 = ORIENTED_EDGE ( 'NONE', *, *, #8853, .F. ) ;
#9413 = ORIENTED_EDGE ( 'NONE', *, *, #11572, .T. ) ;
#9414 = DIRECTION ( 'NONE',  ( 0.000000000000000000, 0.000000000000000000, -1.000000000000000000 ) ) ;
#9415 = CARTESIAN_POINT ( 'NONE',  ( 46.99023568444673060, 29.32451373492759217, 49.12151524109405898 ) ) ;
#9416 = EDGE_CURVE ( 'NONE', #6416, #8280, #21282, .T. ) ;
#9417 = ADVANCED_FACE ( 'NONE', ( #23915 ), #1426, .T. ) ;
#9418 = DIRECTION ( 'NONE',  ( -1.224646799147353207E-16, -1.349345573449484691E-32, 1.000000000000000000 ) ) ;
#9419 = CARTESIAN_POINT ( 'NONE',  ( 21.09992658989238734, 30.84184655352422411, 47.04930799450051637 ) ) ;
#9420 = VERTEX_POINT ( 'NONE', #18976 ) ;
#9421 = FACE_BOUND ( 'NONE', #4130, .T. ) ;
#9422 = EDGE_LOOP ( 'NONE', ( #20927, #3158, #141, #30503 ) ) ;
#9423 = CIRCLE ( 'NONE', #16229, 0.1250000000000001110 ) ;
#9424 = AXIS2_PLACEMENT_3D ( 'NONE', #14672, #24842, #25003 ) ;
#9425 = EDGE_LOOP ( 'NONE', ( #3513, #13446, #24116, #17809 ) ) ;
#9426 = EDGE_CURVE ( 'NONE', #30184, #529, #12357, .T. ) ;
#9427 = DIRECTION ( 'NONE',  ( -1.000000000000000000, -1.101824276508909764E-16, 0.000000000000000000 ) ) ;
#9428 = AXIS2_PLACEMENT_3D ( 'NONE', #4486, #21540, #8918 ) ;
#9429 = AXIS2_PLACEMENT_3D ( 'NONE', #12540, #19907, #12379 ) ;
#9430 = EDGE_LOOP ( 'NONE', ( #28123, #20991, #32343, #7297 ) ) ;
#9431 = AXIS2_PLACEMENT_3D ( 'NONE', #30568, #27451, #10217 ) ;
#9432 = DIRECTION ( 'NONE',  ( -1.101824276508909887E-16, 1.000000000000000000, -0.000000000000000000 ) ) ;
#9433 = CARTESIAN_POINT ( 'NONE',  ( 8.823575513742490273, 15.24673779880127356, 47.37072134000479906 ) ) ;
#9434 = CARTESIAN_POINT ( 'NONE',  ( -40.18454328187963398, 7.548069831825862330, 60.54930799450051637 ) ) ;
#9435 = AXIS2_PLACEMENT_3D ( 'NONE', #16698, #3353, #5350 ) ;
#9436 = ORIENTED_EDGE ( 'NONE', *, *, #2631, .T. ) ;
#9437 = CARTESIAN_POINT ( 'NONE',  ( 21.09785597605720753, -5.098646251524523443, 47.04930799450052348 ) ) ;
#9438 = VERTEX_POINT ( 'NONE', #27357 ) ;
#9439 = CARTESIAN_POINT ( 'NONE',  ( -43.64073206722599707, 1.267352857069778960, 34.64930799450052490 ) ) ;
#9440 = EDGE_CURVE ( 'NONE', #5228, #2485, #24898, .T. ) ;
#9441 = LINE ( 'NONE', #32258, #11088 ) ;
#9442 = DIRECTION ( 'NONE',  ( 0.1949050434465250947, -0.6797146636928670382, 0.7071067811865481278 ) ) ;
#9443 = ORIENTED_EDGE ( 'NONE', *, *, #14720, .F. ) ;
#9444 = CARTESIAN_POINT ( 'NONE',  ( 43.09785597605720397, 14.86454579224779948, 47.04930799450052348 ) ) ;
#9445 = DIRECTION ( 'NONE',  ( 0.000000000000000000, 0.000000000000000000, 1.000000000000000000 ) ) ;
#9446 = CIRCLE ( 'NONE', #12592, 2.000000000000001776 ) ;
#9447 = CARTESIAN_POINT ( 'NONE',  ( 21.09785597605719332, 77.37245976740706510, -36.90550222348115028 ) ) ;
#9448 = EDGE_CURVE ( 'NONE', #17902, #9841, #10797, .T. ) ;
#9449 = CARTESIAN_POINT ( 'NONE',  ( -43.35833523721896654, -3.935454207752183020, 52.04930799450050927 ) ) ;
#9450 = CARTESIAN_POINT ( 'NONE',  ( 47.09785597605719687, 24.86454579224779593, 47.04930799450078638 ) ) ;
#9451 = CARTESIAN_POINT ( 'NONE',  ( 33.72499318558949710, 28.84184655352418858, 47.04930799450051637 ) ) ;
#9452 = VERTEX_POINT ( 'NONE', #22416 ) ;
#9453 = DIRECTION ( 'NONE',  ( -1.224646799147353207E-16, -1.349345573449484691E-32, 1.000000000000000000 ) ) ;
#9454 = ORIENTED_EDGE ( 'NONE', *, *, #3933, .F. ) ;
#9455 = DIRECTION ( 'NONE',  ( -2.779292025043186357E-18, 1.288349127009862211E-17, -1.000000000000000000 ) ) ;
#9456 = ADVANCED_FACE ( 'NONE', ( #31956 ), #32274, .T. ) ;
#9457 = CIRCLE ( 'NONE', #13115, 0.09999999999999753530 ) ;
#9458 = DIRECTION ( 'NONE',  ( 0.2756373558169973870, -0.9612616959383193382, -1.315048337272770435E-17 ) ) ;
#9459 = EDGE_CURVE ( 'NONE', #28129, #25242, #19136, .T. ) ;
#9460 = ORIENTED_EDGE ( 'NONE', *, *, #10487, .T. ) ;
#9461 = AXIS2_PLACEMENT_3D ( 'NONE', #17555, #27572, #12651 ) ;
#9462 = VERTEX_POINT ( 'NONE', #7008 ) ;
#9463 = CIRCLE ( 'NONE', #18881, 0.1250000000000001110 ) ;
#9464 = TOROIDAL_SURFACE ( 'NONE', #12092, 23.50000000000000000, 2.000000000000001776 ) ;
#9465 = UNCERTAINTY_MEASURE_WITH_UNIT (LENGTH_MEASURE( 1.000000000000000082E-05 ), #11738, 'distance_accuracy_value', 'NONE');
#9466 = ORIENTED_EDGE ( 'NONE', *, *, #3889, .F. ) ;
#9467 = CIRCLE ( 'NONE', #15746, 12.27641737965283575 ) ;
#9468 = DIRECTION ( 'NONE',  ( -0.000000000000000000, -1.000000000000000000, 0.000000000000000000 ) ) ;
#9469 = AXIS2_PLACEMENT_3D ( 'NONE', #10140, #23413, #13095 ) ;
#9470 = VERTEX_POINT ( 'NONE', #19302 ) ;
#9471 = ORIENTED_EDGE ( 'NONE', *, *, #25091, .F. ) ;
#9472 = DIRECTION ( 'NONE',  ( -1.101824276508909887E-16, 1.000000000000000000, -0.000000000000000000 ) ) ;
#9473 = DIRECTION ( 'NONE',  ( 0.4848096202463637039, 0.8746197071393810862, 0.000000000000000000 ) ) ;
#9474 = VECTOR ( 'NONE', #1316, 1000.000000000000114 ) ;
#9475 = CARTESIAN_POINT ( 'NONE',  ( -40.47970302497625994, 7.463434137431150361, 60.29072935073781991 ) ) ;
#9476 = DIRECTION ( 'NONE',  ( -0.8746197071393926326, 0.4848096202463430537, 8.676864087101709653E-18 ) ) ;
#9477 = EDGE_CURVE ( 'NONE', #14445, #28679, #2399, .T. ) ;
#9478 = CARTESIAN_POINT ( 'NONE',  ( 44.74832014356462651, 29.82786309983297812, 46.92728461490987257 ) ) ;
#9479 = AXIS2_PLACEMENT_3D ( 'NONE', #29294, #28647, #18780 ) ;
#9480 = ORIENTED_EDGE ( 'NONE', *, *, #22080, .T. ) ;
#9481 = CARTESIAN_POINT ( 'NONE',  ( 8.823509210239501854, 23.59164230456639544, 47.04930799450051637 ) ) ;
#9482 = ORIENTED_EDGE ( 'NONE', *, *, #11238, .T. ) ;
#9483 = CARTESIAN_POINT ( 'NONE',  ( -9.475102253000542873, 5.053071141216427975, -4.190450134571573670 ) ) ;
#9484 = VECTOR ( 'NONE', #26317, 1000.000000000000000 ) ;
#9485 = EDGE_LOOP ( 'NONE', ( #1744, #17144, #7596, #25343 ) ) ;
#9486 = LINE ( 'NONE', #19483, #5877 ) ;
#9487 = FACE_OUTER_BOUND ( 'NONE', #6280, .T. ) ;
#9488 = DIRECTION ( 'NONE',  ( -1.000000000000000000, 0.000000000000000000, 0.000000000000000000 ) ) ;
#9489 = CARTESIAN_POINT ( 'NONE',  ( -40.37748943095153464, 8.220953018982690708, 54.59072935073782418 ) ) ;
#9490 = CARTESIAN_POINT ( 'NONE',  ( 21.09785597605719332, 24.86454579224779948, 47.04930799450051637 ) ) ;
#9491 = CARTESIAN_POINT ( 'NONE',  ( 50.10320668408830613, 27.70621246473837118, 47.20539118556276037 ) ) ;
#9492 = DIRECTION ( 'NONE',  ( -0.000000000000000000, -1.000000000000000000, -0.000000000000000000 ) ) ;
#9493 = DIRECTION ( 'NONE',  ( 0.4848096202463424986, 0.8746197071393928546, -2.220446049250312834E-16 ) ) ;
#9494 = EDGE_LOOP ( 'NONE', ( #20381, #26116, #23964, #513 ) ) ;
#9495 = DIRECTION ( 'NONE',  ( 1.188208965918165239E-16, 1.880121038077813132E-16, 1.000000000000000000 ) ) ;
#9496 = DIRECTION ( 'NONE',  ( 0.000000000000000000, 0.000000000000000000, -1.000000000000000000 ) ) ;
#9497 = VECTOR ( 'NONE', #29017, 1000.000000000000000 ) ;
#9498 = FACE_OUTER_BOUND ( 'NONE', #31590, .T. ) ;
#9499 = ADVANCED_FACE ( 'NONE', ( #29991 ), #26868, .T. ) ;
#9500 = LINE ( 'NONE', #22119, #26858 ) ;
#9501 = CARTESIAN_POINT ( 'NONE',  ( 33.50134396954525329, 25.84164230456639899, 47.04930799450051637 ) ) ;
#9502 = EDGE_LOOP ( 'NONE', ( #14669, #11914, #15074, #8019 ) ) ;
#9503 = ORIENTED_EDGE ( 'NONE', *, *, #8662, .T. ) ;
#9504 = FACE_OUTER_BOUND ( 'NONE', #21593, .T. ) ;
#9505 = VERTEX_POINT ( 'NONE', #4381 ) ;
#9506 = CIRCLE ( 'NONE', #32019, 1.000000000000000888 ) ;
#9507 = AXIS2_PLACEMENT_3D ( 'NONE', #13883, #14695, #25021 ) ;
#9508 = CIRCLE ( 'NONE', #24715, 12.27641737965281976 ) ;
#9509 = AXIS2_PLACEMENT_3D ( 'NONE', #922, #28183, #770 ) ;
#9510 = EDGE_LOOP ( 'NONE', ( #2956, #12509, #797, #20751 ) ) ;
#9511 = PRODUCT_DEFINITION ( 'UNKNOWN', '', #15008, #31149 ) ;
#9512 = DIRECTION ( 'NONE',  ( -1.000000000000000000, 0.000000000000000000, 0.000000000000000000 ) ) ;
#9513 = CARTESIAN_POINT ( 'NONE',  ( 56.35042632428687881, -3.295808585244886402, -3.337848843846767721 ) ) ;
#9514 = CARTESIAN_POINT ( 'NONE',  ( -9.856458276043465361, -5.936245040125576189, 107.6870354947489403 ) ) ;
#9515 = AXIS2_PLACEMENT_3D ( 'NONE', #19150, #1268, #16685 ) ;
#9516 = ORIENTED_EDGE ( 'NONE', *, *, #30807, .T. ) ;
#9517 = DIRECTION ( 'NONE',  ( -1.000000000000000000, 0.000000000000000000, 0.000000000000000000 ) ) ;
#9518 = CARTESIAN_POINT ( 'NONE',  ( -40.15599670534037102, 7.478908884098767196, 34.54930799450052348 ) ) ;
#9519 = CARTESIAN_POINT ( 'NONE',  ( 72.64116057150748418, 7.652955895019256438, 18.28344188472927456 ) ) ;
#9520 = ORIENTED_EDGE ( 'NONE', *, *, #12170, .F. ) ;
#9521 = ORIENTED_EDGE ( 'NONE', *, *, #2484, .F. ) ;
#9522 = CARTESIAN_POINT ( 'NONE',  ( 45.67120842389707747, 22.84434098701873594, 48.65392161081025790 ) ) ;
#9523 = ORIENTED_EDGE ( 'NONE', *, *, #29916, .T. ) ;
#9524 = CARTESIAN_POINT ( 'NONE',  ( 21.09785597605719332, 25.56454579224779167, 75.54930799450052348 ) ) ;
#9525 = VECTOR ( 'NONE', #25352, 1000.000000000000114 ) ;
#9526 = CARTESIAN_POINT ( 'NONE',  ( 21.09992658989239089, 30.09164230456639544, 47.04930799450051637 ) ) ;
#9527 = DIRECTION ( 'NONE',  ( -0.4544104193609908027, 6.737912671758736131E-17, -0.8907924397839086517 ) ) ;
#9528 = AXIS2_PLACEMENT_3D ( 'NONE', #4034, #9125, #19116 ) ;
#9529 = DIRECTION ( 'NONE',  ( -1.101824276508909887E-16, 1.000000000000000000, -0.000000000000000000 ) ) ;
#9530 = AXIS2_PLACEMENT_3D ( 'NONE', #18583, #3821, #21529 ) ;
#9531 = EDGE_LOOP ( 'NONE', ( #20759, #15621, #8027, #21384 ) ) ;
#9532 = ORIENTED_EDGE ( 'NONE', *, *, #335, .T. ) ;
#9533 = FACE_OUTER_BOUND ( 'NONE', #26133, .T. ) ;
#9534 = FACE_OUTER_BOUND ( 'NONE', #15714, .T. ) ;
#9535 = EDGE_CURVE ( 'NONE', #27500, #5504, #22294, .T. ) ;
#9536 = ADVANCED_FACE ( 'NONE', ( #14727 ), #32234, .T. ) ;
#9537 = DIRECTION ( 'NONE',  ( -1.000000000000000000, -1.101824276508909887E-16, 0.000000000000000000 ) ) ;
#9538 = EDGE_CURVE ( 'NONE', #11991, #24621, #16466, .T. ) ;
#9539 = EDGE_CURVE ( 'NONE', #2200, #10117, #23819, .T. ) ;
#9540 = EDGE_LOOP ( 'NONE', ( #12770, #24701 ) ) ;
#9541 = FACE_OUTER_BOUND ( 'NONE', #12620, .T. ) ;
#9542 = CARTESIAN_POINT ( 'NONE',  ( 21.09785597605719332, -13.74048473023143835, 105.2732083928529221 ) ) ;
#9543 = EDGE_CURVE ( 'NONE', #13599, #24672, #11773, .T. ) ;
#9544 = ORIENTED_EDGE ( 'NONE', *, *, #30484, .T. ) ;
#9545 = FACE_OUTER_BOUND ( 'NONE', #14610, .T. ) ;
#9546 = DIRECTION ( 'NONE',  ( 1.000000000000000000, 0.000000000000000000, 0.000000000000000000 ) ) ;
#9547 = AXIS2_PLACEMENT_3D ( 'NONE', #23922, #26393, #3902 ) ;
#9548 = LINE ( 'NONE', #15, #3327 ) ;
#9549 = ORIENTED_EDGE ( 'NONE', *, *, #5945, .F. ) ;
#9550 = AXIS2_PLACEMENT_3D ( 'NONE', #12409, #5346, #23047 ) ;
#9551 = LINE ( 'NONE', #21681, #30611 ) ;
#9552 = DIRECTION ( 'NONE',  ( -0.9612616959383205595, -0.2756373558169932236, 1.660411357259282445E-16 ) ) ;
#9553 = CARTESIAN_POINT ( 'NONE',  ( 73.95065972402362320, 11.92558985988973497, 67.46350265493038023 ) ) ;
#9554 = CARTESIAN_POINT ( 'NONE',  ( 47.20547626766766314, 26.17451373492760069, 44.97710074790751378 ) ) ;
#9555 = ORIENTED_EDGE ( 'NONE', *, *, #21076, .T. ) ;
#9556 = DIRECTION ( 'NONE',  ( 0.000000000000000000, 0.000000000000000000, 1.000000000000000000 ) ) ;
#9557 = ADVANCED_FACE ( 'NONE', ( #6850, #2245, #19794, #11931, #9305, #29326 ), #16849, .F. ) ;
#9558 = SPHERICAL_SURFACE ( 'NONE', #17865, 0.1000000000000000056 ) ;
#9559 = DIRECTION ( 'NONE',  ( -0.8746197071393926326, 0.4848096202463430537, 8.676864087101709653E-18 ) ) ;
#9560 = CARTESIAN_POINT ( 'NONE',  ( 21.09785597605720042, -14.04221034894631615, 47.04930799450051637 ) ) ;
#9561 = CARTESIAN_POINT ( 'NONE',  ( 21.09785597605719332, 30.56454579224779522, 15.74930799450053520 ) ) ;
#9562 = CARTESIAN_POINT ( 'NONE',  ( -4.704135725172235105, -13.74047052604243646, -5.284252768999630590 ) ) ;
#9563 = VECTOR ( 'NONE', #3127, 1000.000000000000000 ) ;
#9564 = PRODUCT ( 'Coil', 'Coil', '', ( #27574 ) ) ;
#9565 = CARTESIAN_POINT ( 'NONE',  ( 47.09785597605719687, 30.56454579224779522, 44.54930799450078638 ) ) ;
#9566 = CARTESIAN_POINT ( 'NONE',  ( 21.09785597605720753, 14.56454579224780055, 47.04930799450052348 ) ) ;
#9567 = ORIENTED_EDGE ( 'NONE', *, *, #15966, .T. ) ;
#9568 = CARTESIAN_POINT ( 'NONE',  ( 45.68651739446661963, 22.98879437201065912, 46.64337703648620703 ) ) ;
#9569 = CARTESIAN_POINT ( 'NONE',  ( 9.016997203727585841, 15.24673779880127356, 46.73295957419995261 ) ) ;
#9570 = AXIS2_PLACEMENT_3D ( 'NONE', #4232, #16682, #9311 ) ;
#9571 = DIRECTION ( 'NONE',  ( -1.000000000000000000, 0.000000000000000000, 0.000000000000000000 ) ) ;
#9572 = EDGE_CURVE ( 'NONE', #1013, #11782, #14391, .T. ) ;
#9573 = CARTESIAN_POINT ( 'NONE',  ( 47.22751897799751220, 27.24253733014356271, 44.55267275764142454 ) ) ;
#9574 = EDGE_CURVE ( 'NONE', #2286, #1790, #22094, .T. ) ;
#9575 = ORIENTED_EDGE ( 'NONE', *, *, #28830, .T. ) ;
#9576 = AXIS2_PLACEMENT_3D ( 'NONE', #27704, #10315, #25248 ) ;
#9577 = CARTESIAN_POINT ( 'NONE',  ( 21.09992658989239089, 25.21183152705960140, 47.04930799450051637 ) ) ;
#9578 = CYLINDRICAL_SURFACE ( 'NONE', #16324, 37.00000000000000711 ) ;
#9579 = LINE ( 'NONE', #54, #25658 ) ;
#9580 = ORIENTED_EDGE ( 'NONE', *, *, #3107, .T. ) ;
#9581 = ORIENTED_EDGE ( 'NONE', *, *, #5152, .T. ) ;
#9582 = LINE ( 'NONE', #12039, #16270 ) ;
#9583 = ADVANCED_FACE ( 'NONE', ( #17335 ), #29826, .T. ) ;
#9584 = CARTESIAN_POINT ( 'NONE',  ( -39.39739818181173803, -5.935416493863505671, 77.98611552785908430 ) ) ;
#9585 = DIRECTION ( 'NONE',  ( 1.000000000000000000, -0.000000000000000000, -0.000000000000000000 ) ) ;
#9586 = FACE_OUTER_BOUND ( 'NONE', #11186, .T. ) ;
#9587 = CARTESIAN_POINT ( 'NONE',  ( 72.88142102655359622, 11.91446173404583853, 26.08880013017983401 ) ) ;
#9588 = ORIENTED_EDGE ( 'NONE', *, *, #12951, .T. ) ;
#9589 = ORIENTED_EDGE ( 'NONE', *, *, #8740, .T. ) ;
#9590 = AXIS2_PLACEMENT_3D ( 'NONE', #21940, #26880, #24413 ) ;
#9591 = CIRCLE ( 'NONE', #27935, 1.500000000000001332 ) ;
#9592 = FACE_OUTER_BOUND ( 'NONE', #4429, .T. ) ;
#9593 = VERTEX_POINT ( 'NONE', #22259 ) ;
#9594 = AXIS2_PLACEMENT_3D ( 'NONE', #20952, #618, #18168 ) ;
#9595 = CARTESIAN_POINT ( 'NONE',  ( 33.46699938050304013, 28.47145308207318237, 47.04930799450050927 ) ) ;
#9596 = CARTESIAN_POINT ( 'NONE',  ( -30.10465965134422106, 11.68564528720922979, 69.71257766022019098 ) ) ;
#9597 = EDGE_CURVE ( 'NONE', #16953, #20581, #10728, .T. ) ;
#9598 = ADVANCED_FACE ( 'NONE', ( #597 ), #4427, .T. ) ;
#9599 = VERTEX_POINT ( 'NONE', #25706 ) ;
#9600 = CARTESIAN_POINT ( 'NONE',  ( 52.02704899015044759, -5.937394935145313468, -13.65255231306078798 ) ) ;
#9601 = EDGE_LOOP ( 'NONE', ( #21554, #6372, #9030, #15092, #21309 ) ) ;
#9602 = DIRECTION ( 'NONE',  ( 1.188208965918165239E-16, 1.880121038077813132E-16, 1.000000000000000000 ) ) ;
#9603 = DIRECTION ( 'NONE',  ( 0.3958453973320081309, 0.7141240004913237405, 0.5773502691896250649 ) ) ;
#9604 = ORIENTED_EDGE ( 'NONE', *, *, #19433, .F. ) ;
#9605 = DIRECTION ( 'NONE',  ( 0.9612616959383266657, 0.2756373558169715743, 0.000000000000000000 ) ) ;
#9606 = DIRECTION ( 'NONE',  ( -1.000000000000000000, -1.101824276508909887E-16, 0.000000000000000000 ) ) ;
#9607 = CARTESIAN_POINT ( 'NONE',  ( 8.823509210239574685, 30.59164230456639544, 47.04930799450051637 ) ) ;
#9608 = CARTESIAN_POINT ( 'NONE',  ( -40.48129536610376533, 8.613360132207176889, 39.44930799450052206 ) ) ;
#9609 = CARTESIAN_POINT ( 'NONE',  ( 21.09785597605719687, 24.86454579224779948, 7.349896848133565364 ) ) ;
#9610 = CIRCLE ( 'NONE', #27958, 0.1250000000000001110 ) ;
#9611 = DIRECTION ( 'NONE',  ( -0.9612616959383208926, -0.2756373558169918914, 1.188214443479423533E-14 ) ) ;
#9612 = ORIENTED_EDGE ( 'NONE', *, *, #31875, .F. ) ;
#9613 = CARTESIAN_POINT ( 'NONE',  ( 62.59785597605721819, 14.86454579224779948, 47.04930799450051637 ) ) ;
#9614 = CYLINDRICAL_SURFACE ( 'NONE', #21686, 2.499999999999997335 ) ;
#9615 = AXIS2_PLACEMENT_3D ( 'NONE', #6683, #1758, #21123 ) ;
#9616 = ORIENTED_EDGE ( 'NONE', *, *, #13826, .T. ) ;
#9617 = EDGE_CURVE ( 'NONE', #30017, #27962, #15371, .T. ) ;
#9618 = CARTESIAN_POINT ( 'NONE',  ( -45.58207439260966964, -5.881649745666465812, 53.58233204886106904 ) ) ;
#9619 = CARTESIAN_POINT ( 'NONE',  ( 21.09992658989239089, 26.72145308207318948, 47.04930799450051637 ) ) ;
#9620 = AXIS2_PLACEMENT_3D ( 'NONE', #28308, #28471, #734 ) ;
#9621 = ORIENTED_EDGE ( 'NONE', *, *, #32083, .F. ) ;
#9622 = CIRCLE ( 'NONE', #32158, 15.52755282421446026 ) ;
#9623 = TOROIDAL_SURFACE ( 'NONE', #12780, 1.299999999999999822, 0.1000000000000000056 ) ;
#9624 = ORIENTED_EDGE ( 'NONE', *, *, #1621, .T. ) ;
#9625 = EDGE_LOOP ( 'NONE', ( #2435, #11426, #23644, #25768 ) ) ;
#9626 = EDGE_CURVE ( 'NONE', #31872, #25938, #1275, .T. ) ;
#9627 = EDGE_CURVE ( 'NONE', #26975, #29567, #12305, .T. ) ;
#9628 = VECTOR ( 'NONE', #20725, 1000.000000000000114 ) ;
#9629 = CARTESIAN_POINT ( 'NONE',  ( 21.09785597605719332, 40.06454579224778456, 47.04930799450051637 ) ) ;
#9630 = ADVANCED_FACE ( 'NONE', ( #10453 ), #5684, .F. ) ;
#9631 = ADVANCED_FACE ( 'NONE', ( #30642 ), #15953, .T. ) ;
#9632 = EDGE_LOOP ( 'NONE', ( #7107, #28517, #8747 ) ) ;
#9633 = ORIENTED_EDGE ( 'NONE', *, *, #4301, .T. ) ;
#9634 = FACE_OUTER_BOUND ( 'NONE', #9713, .T. ) ;
#9635 = EDGE_CURVE ( 'NONE', #15925, #13273, #18143, .T. ) ;
#9636 = AXIS2_PLACEMENT_3D ( 'NONE', #28625, #13382, #10760 ) ;
#9637 = DIRECTION ( 'NONE',  ( 0.2756373558169974980, -0.9612616959383193382, -1.315048337272770589E-17 ) ) ;
#9638 = CARTESIAN_POINT ( 'NONE',  ( -41.34584395867850048, 11.59800658573647247, 57.04930799450051637 ) ) ;
#9639 = DIRECTION ( 'NONE',  ( -1.000000000000000000, 0.000000000000000000, 0.000000000000000000 ) ) ;
#9640 = ORIENTED_EDGE ( 'NONE', *, *, #11266, .F. ) ;
#9641 = DIRECTION ( 'NONE',  ( 0.000000000000000000, -1.000000000000000000, 0.000000000000000000 ) ) ;
#9642 = ORIENTED_EDGE ( 'NONE', *, *, #22038, .T. ) ;
#9643 = CARTESIAN_POINT ( 'NONE',  ( -32.19571876111664466, 1.434145862199238675, 14.44898717713608427 ) ) ;
#9644 = FACE_OUTER_BOUND ( 'NONE', #21802, .T. ) ;
#9645 = ORIENTED_EDGE ( 'NONE', *, *, #26289, .T. ) ;
#9646 = CARTESIAN_POINT ( 'NONE',  ( -40.65487266620045403, 9.475231293617262907, 34.66144002885648945 ) ) ;
#9647 = DIRECTION ( 'NONE',  ( 0.000000000000000000, -1.000000000000000000, 0.000000000000000000 ) ) ;
#9648 = CARTESIAN_POINT ( 'NONE',  ( 21.09785597605719332, 44.99492099041257376, 47.04930799450051637 ) ) ;
#9649 = DIRECTION ( 'NONE',  ( 0.000000000000000000, 0.000000000000000000, -1.000000000000000000 ) ) ;
#9650 = CARTESIAN_POINT ( 'NONE',  ( 46.86059137560834387, 22.89977464660286444, 48.89819542093576388 ) ) ;
#9651 = CARTESIAN_POINT ( 'NONE',  ( 47.20547626766765603, 29.58791119454915020, 44.97710074790751378 ) ) ;
#9652 = DIRECTION ( 'NONE',  ( -0.7141240004913198547, 0.3958453973320100738, -0.5773502691896283956 ) ) ;
#9653 = DIRECTION ( 'NONE',  ( 0.000000000000000000, 3.756723415560144304E-15, -1.000000000000000000 ) ) ;
#9654 = VERTEX_POINT ( 'NONE', #2734 ) ;
#9655 = ADVANCED_FACE ( 'NONE', ( #2893, #3211 ), #759, .T. ) ;
#9656 = CYLINDRICAL_SURFACE ( 'NONE', #15553, 10.00000000000000888 ) ;
#9657 = CARTESIAN_POINT ( 'NONE',  ( -40.23397449525940317, 6.794506605641760899, 39.44930799450052206 ) ) ;
#9658 = CARTESIAN_POINT ( 'NONE',  ( 1.839586350524081038, 7.881678200673685630, 47.04930799450051637 ) ) ;
#9659 = FACE_OUTER_BOUND ( 'NONE', #26721, .T. ) ;
#9660 = CARTESIAN_POINT ( 'NONE',  ( -38.57628410747783221, 8.768497289655476479, 19.08884019352816352 ) ) ;
#9661 = ORIENTED_EDGE ( 'NONE', *, *, #10730, .F. ) ;
#9662 =( BOUNDED_CURVE ( )  B_SPLINE_CURVE ( 2, ( #20569, #3000, #8263, #8107, #3484, #866, #23025, #545, #28130 ),
 .UNSPECIFIED., .F., .F. ) 
 B_SPLINE_CURVE_WITH_KNOTS ( ( 3, 2, 2, 2, 3 ),
 ( 0.5357142868755583320, 0.5476190476190476719, 0.5714285714285713969, 0.5952380952380952328, 0.6071428583041297289 ),
 .UNSPECIFIED. ) 
 CURVE ( )  GEOMETRIC_REPRESENTATION_ITEM ( )  RATIONAL_B_SPLINE_CURVE ( ( 0.9330127018922200755, 0.9330127084266224280, 1.000000000000000000, 0.8660254037844388186, 1.000000000000000000, 0.8660254037844388186, 1.000000000000000000, 0.9330126953578163906, 0.9330127018922200755 ) ) 
 REPRESENTATION_ITEM ( '' )  );
#9663 = ORIENTED_EDGE ( 'NONE', *, *, #21357, .T. ) ;
#9664 = DIRECTION ( 'NONE',  ( 0.8746197071393928546, -0.4848096202463424986, -1.277302113040826515E-17 ) ) ;
#9665 = CIRCLE ( 'NONE', #6515, 12.36707279061065101 ) ;
#9666 = ORIENTED_EDGE ( 'NONE', *, *, #24639, .F. ) ;
#9667 = EDGE_CURVE ( 'NONE', #3138, #4416, #19619, .T. ) ;
#9668 = ADVANCED_FACE ( 'NONE', ( #23243 ), #30792, .F. ) ;
#9669 = ORIENTED_EDGE ( 'NONE', *, *, #22634, .T. ) ;
#9670 = DIRECTION ( 'NONE',  ( -1.224646799147353207E-16, 0.000000000000000000, -1.000000000000000000 ) ) ;
#9671 = CARTESIAN_POINT ( 'NONE',  ( 52.07597786784162253, -5.935454337261171887, -13.45772645143417634 ) ) ;
#9672 = ADVANCED_FACE ( 'NONE', ( #28335 ), #4949, .F. ) ;
#9673 = ORIENTED_EDGE ( 'NONE', *, *, #976, .T. ) ;
#9674 = EDGE_CURVE ( 'NONE', #13651, #30857, #30666, .T. ) ;
#9675 = CIRCLE ( 'NONE', #30663, 0.1250000000000001110 ) ;
#9676 = DIRECTION ( 'NONE',  ( 0.2756373558169942228, -0.9612616959383203374, 0.000000000000000000 ) ) ;
#9677 = DIRECTION ( 'NONE',  ( -0.9612616959383207815, -0.2756373558169926685, -8.795445018804289444E-19 ) ) ;
#9678 = CARTESIAN_POINT ( 'NONE',  ( -41.02687597405218156, 7.220473278338834788, 60.44930799450051495 ) ) ;
#9679 = AXIS2_PLACEMENT_3D ( 'NONE', #7826, #8153, #13081 ) ;
#9680 = CARTESIAN_POINT ( 'NONE',  ( 48.40186567930498285, 26.02957786121582373, 45.03923535223908203 ) ) ;
#9681 = VERTEX_POINT ( 'NONE', #20125 ) ;
#9682 = VERTEX_POINT ( 'NONE', #30480 ) ;
#9684 = FILL_AREA_STYLE_COLOUR ( '', #28034 ) ;
#9683 = CIRCLE ( 'NONE', #32236, 2.500000000000002220 ) ;
#9685 = VECTOR ( 'NONE', #16172, 1000.000000000000000 ) ;
#9686 = ORIENTED_EDGE ( 'NONE', *, *, #5361, .F. ) ;
#9687 = CARTESIAN_POINT ( 'NONE',  ( 21.09785597605719332, 25.56454579224779877, 67.04930799450050927 ) ) ;
#9688 = TOROIDAL_SURFACE ( 'NONE', #20671, 1.299999999999999822, 0.1000000000000000056 ) ;
#9689 = CARTESIAN_POINT ( 'NONE',  ( -40.70335362822509495, 9.387769322903324110, 34.54930799450052348 ) ) ;
#9690 = CARTESIAN_POINT ( 'NONE',  ( -40.69571722278732295, 6.786566810383045656, 34.64930799450051779 ) ) ;
#9691 = LINE ( 'NONE', #24451, #1090 ) ;
#9692 = CARTESIAN_POINT ( 'NONE',  ( 45.24946171279598417, 27.72124452788248661, 47.99220971130007740 ) ) ;
#9693 = DIRECTION ( 'NONE',  ( 0.9183650514339934956, -1.526556658859590243E-16, -0.3957342950827468231 ) ) ;
#9694 = ORIENTED_EDGE ( 'NONE', *, *, #11434, .F. ) ;
#9695 = VERTEX_POINT ( 'NONE', #7666 ) ;
#9696 = DIRECTION ( 'NONE',  ( 0.000000000000000000, 0.000000000000000000, 1.000000000000000000 ) ) ;
#9697 = CARTESIAN_POINT ( 'NONE',  ( -39.59300248568538194, 7.744584186742828891, 61.94930799450052206 ) ) ;
#9698 = B_SPLINE_CURVE_WITH_KNOTS ( 'NONE', 3,
 ( #2259, #19485, #7019, #12279, #17013, #12117, #4887, #17177, #32301, #27194, #4721, #22426 ),
 .UNSPECIFIED., .F., .F.,
 ( 4, 2, 2, 2, 2, 4 ),
 ( 0.000000000000000000, 7.696047042341537254E-05, 0.0001154407056351002296, 0.0001539209408467850731, 0.0002308814112701253239, 0.0003078418816934655748 ),
 .UNSPECIFIED. ) ;
#9699 = CARTESIAN_POINT ( 'NONE',  ( -41.63422246745999189, 11.51531537899137447, 57.95249952744806166 ) ) ;
#9700 = VERTEX_POINT ( 'NONE', #15209 ) ;
#9701 = CARTESIAN_POINT ( 'NONE',  ( 48.59475124299144255, 29.58954579224780090, 45.61232171765963272 ) ) ;
#9702 = DIRECTION ( 'NONE',  ( -1.101824276508909887E-16, 1.000000000000000000, -0.000000000000000000 ) ) ;
#9703 = ORIENTED_EDGE ( 'NONE', *, *, #15756, .T. ) ;
#9704 = DIRECTION ( 'NONE',  ( -0.000000000000000000, -1.000000000000000000, -0.000000000000000000 ) ) ;
#9705 = CARTESIAN_POINT ( 'NONE',  ( 44.09250526802607340, 26.65621246473837402, 46.89322480343881949 ) ) ;
#9706 = DIRECTION ( 'NONE',  ( -0.2756373558169932236, 0.9612616959383204485, -1.479773560108267395E-16 ) ) ;
#9707 = CONICAL_SURFACE ( 'NONE', #27013, 58.09216821878680292, 1.269872874662833384 ) ;
#9708 = CIRCLE ( 'NONE', #20167, 12.62506659569710266 ) ;
#9709 = AXIS2_PLACEMENT_3D ( 'NONE', #78, #7794, #25351 ) ;
#9710 = TOROIDAL_SURFACE ( 'NONE', #19127, 12.40141737965283575, 0.1250000000000000278 ) ;
#9711 = AXIS2_PLACEMENT_3D ( 'NONE', #7041, #28890, #17044 ) ;
#9712 = ORIENTED_EDGE ( 'NONE', *, *, #18523, .T. ) ;
#9713 = EDGE_LOOP ( 'NONE', ( #6244, #15193, #4596, #12695 ) ) ;
#9714 = LINE ( 'NONE', #29574, #2327 ) ;
#9715 = CARTESIAN_POINT ( 'NONE',  ( -40.51442171646695556, 7.400645970086839220, 60.37414278400746070 ) ) ;
#9716 = DIRECTION ( 'NONE',  ( -1.000000000000000000, -1.101824276508909764E-16, 0.000000000000000000 ) ) ;
#9717 = EDGE_CURVE ( 'NONE', #8855, #777, #8621, .T. ) ;
#9718 = ORIENTED_EDGE ( 'NONE', *, *, #11600, .F. ) ;
#9719 = EDGE_CURVE ( 'NONE', #19450, #19780, #31169, .T. ) ;
#9720 = CARTESIAN_POINT ( 'NONE',  ( -9.880269303432738681, -5.935454207752202116, -12.56967651669337727 ) ) ;
#9721 = CARTESIAN_POINT ( 'NONE',  ( -39.67555847965937943, 2.645252416024336028, 49.04930799450051637 ) ) ;
#9722 = APPLICATION_CONTEXT ( 'automotive_design' ) ;
#9723 = CARTESIAN_POINT ( 'NONE',  ( 52.14473852644682950, 4.272108154687120241, -4.410933505873395610 ) ) ;
#9724 = CARTESIAN_POINT ( 'NONE',  ( -40.11286833322908052, 2.887657226147509970, 59.04930799450051637 ) ) ;
#9725 = DIRECTION ( 'NONE',  ( -1.000000000000000000, 0.000000000000000000, 0.000000000000000000 ) ) ;
#9726 = DIRECTION ( 'NONE',  ( 0.000000000000000000, 1.000000000000000000, 0.000000000000000000 ) ) ;
#9727 = CARTESIAN_POINT ( 'NONE',  ( 21.09785597605720753, 14.05098971466613023, 47.04930799450052348 ) ) ;
#9728 = DIRECTION ( 'NONE',  ( -0.4544104193609908027, -5.611869858668450607E-17, -0.8907924397839086517 ) ) ;
#9729 = VECTOR ( 'NONE', #3895, 1000.000000000000000 ) ;
#9730 = CARTESIAN_POINT ( 'NONE',  ( 21.09785597605719332, -16.63545420775219696, 47.04930799450051637 ) ) ;
#9731 = PRESENTATION_STYLE_ASSIGNMENT (( #24986 ) ) ;
#9732 = AXIS2_PLACEMENT_3D ( 'NONE', #29216, #11336, #24124 ) ;
#9733 = ORIENTED_EDGE ( 'NONE', *, *, #11167, .T. ) ;
#9734 = EDGE_LOOP ( 'NONE', ( #17920, #24811, #14750, #5245 ) ) ;
#9735 = CARTESIAN_POINT ( 'NONE',  ( 21.09785597605719332, -15.72540370141337007, 47.04930799450051637 ) ) ;
#9736 =( GEOMETRIC_REPRESENTATION_CONTEXT ( 3 ) GLOBAL_UNCERTAINTY_ASSIGNED_CONTEXT ( ( #6510 ) ) GLOBAL_UNIT_ASSIGNED_CONTEXT ( ( #21204, #3823, #28770 ) ) REPRESENTATION_CONTEXT ( 'NONE', 'WORKASPACE' ) );
#9737 = CARTESIAN_POINT ( 'NONE',  ( -40.15599670534037102, 7.478908884098773413, 38.44930799450052916 ) ) ;
#9738 = CARTESIAN_POINT ( 'NONE',  ( -31.75494777190924367, 11.92558985988973319, 67.46350265493038023 ) ) ;
#9739 = AXIS2_PLACEMENT_3D ( 'NONE', #8111, #3004, #720 ) ;
#9740 = CARTESIAN_POINT ( 'NONE',  ( 80.85108986838916678, -3.295808585244886402, 82.30187834273041858 ) ) ;
#9741 = EDGE_LOOP ( 'NONE', ( #8183, #12230 ) ) ;
#9742 = CARTESIAN_POINT ( 'NONE',  ( -39.56345036642217394, -5.935781861350975852, 77.89068591715864898 ) ) ;
#9743 = DIRECTION ( 'NONE',  ( -0.3958453973320076313, -0.7141240004913228523, 0.5773502691896265082 ) ) ;
#9744 = CARTESIAN_POINT ( 'NONE',  ( -58.11219453028166981, -16.63545420775219696, 44.54930799450023216 ) ) ;
#9745 = VERTEX_POINT ( 'NONE', #3862 ) ;
#9746 = ORIENTED_EDGE ( 'NONE', *, *, #20568, .F. ) ;
#9747 = FACE_OUTER_BOUND ( 'NONE', #28582, .T. ) ;
#9748 = LINE ( 'NONE', #2192, #15698 ) ;
#9749 = DIRECTION ( 'NONE',  ( -1.101824276508909887E-16, 1.000000000000000000, -0.000000000000000000 ) ) ;
#9750 = AXIS2_PLACEMENT_3D ( 'NONE', #21964, #4419, #19831 ) ;
#9751 = FACE_OUTER_BOUND ( 'NONE', #19615, .T. ) ;
#9752 = DIRECTION ( 'NONE',  ( 0.000000000000000000, -0.000000000000000000, -1.000000000000000000 ) ) ;
#9753 = VERTEX_POINT ( 'NONE', #19393 ) ;
#9754 = ORIENTED_EDGE ( 'NONE', *, *, #18730, .F. ) ;
#9755 = LINE ( 'NONE', #29776, #7938 ) ;
#9756 = CIRCLE ( 'NONE', #28109, 12.62506659569710266 ) ;
#9757 = MECHANICAL_DESIGN_GEOMETRIC_PRESENTATION_REPRESENTATION (  '', ( #20765 ), #28110 ) ;
#9758 = VERTEX_POINT ( 'NONE', #16166 ) ;
#9759 = EDGE_CURVE ( 'NONE', #2732, #27609, #13556, .T. ) ;
#9760 = EDGE_CURVE ( 'NONE', #20704, #5958, #22247, .T. ) ;
#9761 = ADVANCED_FACE ( 'NONE', ( #26178 ), #14918, .T. ) ;
#9762 = DIRECTION ( 'NONE',  ( -0.000000000000000000, -1.000000000000000000, 0.000000000000000000 ) ) ;
#9763 = FACE_OUTER_BOUND ( 'NONE', #27399, .T. ) ;
#9764 = EDGE_CURVE ( 'NONE', #6401, #4559, #26448, .T. ) ;
#9765 = TOROIDAL_SURFACE ( 'NONE', #9243, 1.899999999999999467, 0.1000000000000000056 ) ;
#9766 = ORIENTED_EDGE ( 'NONE', *, *, #13633, .F. ) ;
#9767 = CARTESIAN_POINT ( 'NONE',  ( -40.79464149312965304, 8.438755658900303658, 34.56232498761289662 ) ) ;
#9768 = ORIENTED_EDGE ( 'NONE', *, *, #6569, .T. ) ;
#9769 = DIRECTION ( 'NONE',  ( -1.000000000000000000, -1.101824276508910010E-16, 0.000000000000000000 ) ) ;
#9770 = DIRECTION ( 'NONE',  ( 0.000000000000000000, 0.000000000000000000, -1.000000000000000000 ) ) ;
#9771 = CARTESIAN_POINT ( 'NONE',  ( 21.09785597605720753, 13.86454579224779948, 47.04930799450052348 ) ) ;
#9772 = ORIENTED_EDGE ( 'NONE', *, *, #10861, .T. ) ;
#9773 = CARTESIAN_POINT ( 'NONE',  ( 21.09785597605719332, 12.26495659406217342, -9.420836024117583918 ) ) ;
#9774 = CARTESIAN_POINT ( 'NONE',  ( 33.46699938050304013, 29.97145308207317527, 47.04930799450050927 ) ) ;
#9775 = PLANE ( 'NONE',  #21034 ) ;
#9776 = DIRECTION ( 'NONE',  ( -1.188208965918165239E-16, -1.880121038077813132E-16, -1.000000000000000000 ) ) ;
#9777 = DIRECTION ( 'NONE',  ( 0.4848096202463366700, 0.8746197071393961853, 9.920727850372755527E-18 ) ) ;
#9778 = CARTESIAN_POINT ( 'NONE',  ( 72.45825863272662559, 9.437824910247664789, 74.07738419657177076 ) ) ;
#9779 = EDGE_LOOP ( 'NONE', ( #21840, #28367, #30816, #27592 ) ) ;
#9780 = CARTESIAN_POINT ( 'NONE',  ( 73.95065972402376531, 11.92558985988973497, 26.63511333407101134 ) ) ;
#9781 = CARTESIAN_POINT ( 'NONE',  ( 21.09785597605719332, 45.28940914544685370, 47.04930799450051637 ) ) ;
#9782 = ORIENTED_EDGE ( 'NONE', *, *, #7668, .F. ) ;
#9783 = CARTESIAN_POINT ( 'NONE',  ( 33.71785032049137243, 25.46664230456640254, 47.04930799450051637 ) ) ;
#9784 = AXIS2_PLACEMENT_3D ( 'NONE', #10991, #16696, #19160 ) ;
#9785 = LINE ( 'NONE', #12908, #9071 ) ;
#9786 = ORIENTED_EDGE ( 'NONE', *, *, #10166, .F. ) ;
#9787 = ORIENTED_EDGE ( 'NONE', *, *, #15564, .F. ) ;
#9788 = ADVANCED_FACE ( 'NONE', ( #8631 ), #24337, .T. ) ;
#9789 = PRODUCT_DEFINITION_CONTEXT ( 'detailed design', #27107, 'design' ) ;
#9790 = EDGE_CURVE ( 'NONE', #19469, #5687, #16993, .T. ) ;
#9791 = AXIS2_PLACEMENT_3D ( 'NONE', #9384, #4460, #24809 ) ;
#9792 = ORIENTED_EDGE ( 'NONE', *, *, #7414, .T. ) ;
#9793 = DIRECTION ( 'NONE',  ( 0.000000000000000000, -1.000000000000000000, 0.000000000000000000 ) ) ;
#9794 = EDGE_CURVE ( 'NONE', #12904, #14845, #750, .T. ) ;
#9795 = CIRCLE ( 'NONE', #13993, 12.62506659569710266 ) ;
#9796 = VERTEX_POINT ( 'NONE', #23721 ) ;
#9797 = ORIENTED_EDGE ( 'NONE', *, *, #5970, .T. ) ;
#9798 = DIRECTION ( 'NONE',  ( 2.779292025043186357E-18, -1.288349127009862211E-17, 1.000000000000000000 ) ) ;
#9799 = CARTESIAN_POINT ( 'NONE',  ( 41.51205063648687599, 11.92558985988973497, -5.803495753465989893 ) ) ;
#9800 = DIRECTION ( 'NONE',  ( -0.000000000000000000, -1.000000000000000000, 0.000000000000000000 ) ) ;
#9801 = PLANE ( 'NONE',  #9062 ) ;
#9802 = CARTESIAN_POINT ( 'NONE',  ( -41.77464577679392477, 3.808795504615560379, 49.04930799450051637 ) ) ;
#9803 = EDGE_LOOP ( 'NONE', ( #20825, #11661 ) ) ;
#9804 = DIRECTION ( 'NONE',  ( -0.000000000000000000, -1.000000000000000000, 0.000000000000000000 ) ) ;
#9805 = ORIENTED_EDGE ( 'NONE', *, *, #12456, .F. ) ;
#9806 = CARTESIAN_POINT ( 'NONE',  ( -33.75433321778603357, -2.003187929803778466, 13.34606976912072618 ) ) ;
#9807 = CARTESIAN_POINT ( 'NONE',  ( 46.04844006429465253, 22.86454579224779948, 44.99211097489548905 ) ) ;
#9808 = VERTEX_POINT ( 'NONE', #10935 ) ;
#9809 = CARTESIAN_POINT ( 'NONE',  ( 21.09785597605719332, 25.76454579224781227, 47.04930799450051637 ) ) ;
#9810 = CARTESIAN_POINT ( 'NONE',  ( 8.732853799281720342, 30.97145308207317171, 47.04930799450051637 ) ) ;
#9811 = FACE_OUTER_BOUND ( 'NONE', #10156, .T. ) ;
#9812 = CARTESIAN_POINT ( 'NONE',  ( 21.09785597605720753, 14.86454579224779948, 47.04930799450052348 ) ) ;
#9813 = FACE_OUTER_BOUND ( 'NONE', #25403, .T. ) ;
#9814 = CARTESIAN_POINT ( 'NONE',  ( 45.79384627280941089, 28.47957786121581591, 49.05938063676249072 ) ) ;
#9815 = DIRECTION ( 'NONE',  ( -1.000000000000000000, 0.000000000000000000, 0.000000000000000000 ) ) ;
#9816 = DIRECTION ( 'NONE',  ( -1.101824276508909887E-16, 1.000000000000000000, -0.000000000000000000 ) ) ;
#9817 = ADVANCED_FACE ( 'NONE', ( #15858 ), #28547, .F. ) ;
#9818 = ORIENTED_EDGE ( 'NONE', *, *, #30903, .F. ) ;
#9819 = CARTESIAN_POINT ( 'NONE',  ( 47.12239238930854413, 29.59960605238285680, 44.98451356130378542 ) ) ;
#9820 = ORIENTED_EDGE ( 'NONE', *, *, #11767, .F. ) ;
#9821 = ADVANCED_FACE ( 'NONE', ( #30962 ), #8777, .T. ) ;
#9822 = CARTESIAN_POINT ( 'NONE',  ( 21.09785597605720042, -52.14605111273580462, 47.04930799450051637 ) ) ;
#9823 = CARTESIAN_POINT ( 'NONE',  ( 8.096071960694297687, 17.16467605102632632, 47.04930799450052348 ) ) ;
#9824 = ORIENTED_EDGE ( 'NONE', *, *, #18018, .F. ) ;
#9825 = ORIENTED_EDGE ( 'NONE', *, *, #19983, .F. ) ;
#9826 = CARTESIAN_POINT ( 'NONE',  ( 21.09992658989239089, 25.34164230456639899, 47.04930799450051637 ) ) ;
#9827 = ADVANCED_FACE ( 'NONE', ( #1227 ), #19079, .T. ) ;
#9828 = AXIS2_PLACEMENT_3D ( 'NONE', #25157, #20067, #24836 ) ;
#9829 = ADVANCED_FACE ( 'NONE', ( #16011 ), #7575, .F. ) ;
#9830 = EDGE_CURVE ( 'NONE', #31580, #21967, #25408, .T. ) ;
#9831 = ORIENTED_EDGE ( 'NONE', *, *, #28980, .F. ) ;
#9832 = AXIS2_PLACEMENT_3D ( 'NONE', #4146, #21862, #22355 ) ;
#9833 = ORIENTED_EDGE ( 'NONE', *, *, #707, .F. ) ;
#9834 = CARTESIAN_POINT ( 'NONE',  ( 45.69268131687783807, 22.99884124225578574, 46.97633003370108185 ) ) ;
#9835 = ADVANCED_FACE ( 'NONE', ( #6323 ), #16325, .F. ) ;
#9836 = EDGE_LOOP ( 'NONE', ( #27006, #24567, #9633, #2075 ) ) ;
#9837 = DIRECTION ( 'NONE',  ( -1.188208965918165239E-16, -1.880121038077813132E-16, -1.000000000000000000 ) ) ;
#9838 = DIRECTION ( 'NONE',  ( -1.101824276508909887E-16, 1.000000000000000000, -0.000000000000000000 ) ) ;
#9839 = CARTESIAN_POINT ( 'NONE',  ( 47.79865503179234310, 9.702389020015065313, 132.0493079945005377 ) ) ;
#9840 = CARTESIAN_POINT ( 'NONE',  ( 49.44739180854976013, 29.43456182964375856, 47.17133137409169308 ) ) ;
#9841 = VERTEX_POINT ( 'NONE', #1390 ) ;
#9842 = CIRCLE ( 'NONE', #31862, 12.36707279061065101 ) ;
#9843 = ORIENTED_EDGE ( 'NONE', *, *, #27936, .T. ) ;
#9844 = TOROIDAL_SURFACE ( 'NONE', #30283, 12.61792373059899397, 0.1249999999999959616 ) ;
#9845 = VERTEX_POINT ( 'NONE', #11405 ) ;
#9846 = CARTESIAN_POINT ( 'NONE',  ( -40.47630348341014184, 7.507564784836493921, 35.32879591952760734 ) ) ;
#9847 = CARTESIAN_POINT ( 'NONE',  ( 21.09785597605720042, -17.03545420775220265, 47.04930799450051637 ) ) ;
#9848 = CARTESIAN_POINT ( 'NONE',  ( 21.09785597605720042, -13.98292989133646103, -11.62287111200335055 ) ) ;
#9849 = CIRCLE ( 'NONE', #12483, 12.98419020052701889 ) ;
#9850 = CARTESIAN_POINT ( 'NONE',  ( 52.70461778898049232, -5.822320178462010887, -11.79187305797365504 ) ) ;
#9851 = CARTESIAN_POINT ( 'NONE',  ( 46.99023568444673060, 27.83791119454915375, 49.12151524109405898 ) ) ;
#9852 = EDGE_CURVE ( 'NONE', #25360, #22418, #13027, .T. ) ;
#9853 = ORIENTED_EDGE ( 'NONE', *, *, #12500, .F. ) ;
#9854 = ORIENTED_EDGE ( 'NONE', *, *, #3517, .T. ) ;
#9855 = CARTESIAN_POINT ( 'NONE',  ( 21.09785597605720753, 14.86454579224779948, 47.04930799450052348 ) ) ;
#9856 = CARTESIAN_POINT ( 'NONE',  ( 45.36511207810799107, 28.73213139976340713, 45.12672418911605376 ) ) ;
#9857 = ADVANCED_FACE ( 'NONE', ( #7260 ), #30235, .T. ) ;
#9858 = CIRCLE ( 'NONE', #15604, 2.500000000000002220 ) ;
#9859 = CARTESIAN_POINT ( 'NONE',  ( 33.46699938050304013, 23.71183152705959429, 47.04930799450051637 ) ) ;
#9860 = ORIENTED_EDGE ( 'NONE', *, *, #26603, .F. ) ;
#9861 = CARTESIAN_POINT ( 'NONE',  ( 47.20547626766765603, 28.27451373492759501, 44.97710074790751378 ) ) ;
#9862 = DIRECTION ( 'NONE',  ( -0.000000000000000000, -1.000000000000000000, -0.000000000000000000 ) ) ;
#9863 = ORIENTED_EDGE ( 'NONE', *, *, #11646, .T. ) ;
#9864 = CARTESIAN_POINT ( 'NONE',  ( 48.46535932150934656, 25.48954579807171328, 49.73005965046827015 ) ) ;
#9865 = EDGE_CURVE ( 'NONE', #21721, #15784, #2374, .T. ) ;
#9866 = CARTESIAN_POINT ( 'NONE',  ( -39.85048242108726413, 2.742214340073605428, 45.04930799450051637 ) ) ;
#9867 = EDGE_CURVE ( 'NONE', #11837, #17879, #32249, .T. ) ;
#9868 = VECTOR ( 'NONE', #11317, 1000.000000000000000 ) ;
#9869 = ORIENTED_EDGE ( 'NONE', *, *, #2990, .T. ) ;
#9870 = VECTOR ( 'NONE', #2502, 1000.000000000000000 ) ;
#9871 = EDGE_LOOP ( 'NONE', ( #25042, #29099 ) ) ;
#9872 = CARTESIAN_POINT ( 'NONE',  ( -37.21204910874187988, -5.721341737285086992, 15.20211895544695757 ) ) ;
#9873 = CARTESIAN_POINT ( 'NONE',  ( 72.66553924771079664, 10.95889540305196519, 71.79150321602543272 ) ) ;
#9874 = CARTESIAN_POINT ( 'NONE',  ( 49.49063479933183629, 25.29951373492760069, 47.17357720316391578 ) ) ;
#9875 = CIRCLE ( 'NONE', #20339, 0.1000000000000007688 ) ;
#9876 = VERTEX_POINT ( 'NONE', #20048 ) ;
#9877 = CARTESIAN_POINT ( 'NONE',  ( -43.64647580959332629, 1.256990871545142774, 60.54930799450051637 ) ) ;
#9878 = LINE ( 'NONE', #20692, #23195 ) ;
#9879 = CARTESIAN_POINT ( 'NONE',  ( 53.93732357960501389, 0.8961463385898192913, -5.505979700512947161 ) ) ;
#9880 = DIRECTION ( 'NONE',  ( 0.000000000000000000, -1.000000000000000000, 0.000000000000000000 ) ) ;
#9881 = CARTESIAN_POINT ( 'NONE',  ( -40.50726676055796105, 7.559560307024983494, 60.44930799450051495 ) ) ;
#9882 = DIRECTION ( 'NONE',  ( 0.4848096202463424986, 0.8746197071393928546, -2.220446049250312834E-16 ) ) ;
#9883 = FACE_OUTER_BOUND ( 'NONE', #6670, .T. ) ;
#9884 = DIRECTION ( 'NONE',  ( -1.101824276508909887E-16, 1.000000000000000000, -0.000000000000000000 ) ) ;
#9885 = LINE ( 'NONE', #3700, #290 ) ;
#9886 = ADVANCED_FACE ( 'NONE', ( #15295 ), #7746, .T. ) ;
#9887 = FACE_OUTER_BOUND ( 'NONE', #16254, .T. ) ;
#9888 =( LENGTH_UNIT ( ) NAMED_UNIT ( * ) SI_UNIT ( .MILLI., .METRE. ) );
#9889 = EDGE_LOOP ( 'NONE', ( #8699, #10280, #627, #25078 ) ) ;
#9890 = ORIENTED_EDGE ( 'NONE', *, *, #5499, .T. ) ;
#9891 = CARTESIAN_POINT ( 'NONE',  ( 21.09785597605720753, 13.86454579224779948, 47.04930799450052348 ) ) ;
#9892 = AXIS2_PLACEMENT_3D ( 'NONE', #18616, #23874, #4345 ) ;
#9893 = LINE ( 'NONE', #14825, #17190 ) ;
#9894 = LINE ( 'NONE', #6942, #25541 ) ;
#9895 = CIRCLE ( 'NONE', #17728, 32.50000000000000000 ) ;
#9896 = VECTOR ( 'NONE', #27905, 1000.000000000000000 ) ;
#9897 = CARTESIAN_POINT ( 'NONE',  ( 54.71965117484201357, -3.543532154952170110, 102.0142634691762709 ) ) ;
#9898 = ORIENTED_EDGE ( 'NONE', *, *, #15958, .T. ) ;
#9899 = CARTESIAN_POINT ( 'NONE',  ( 21.09992658989239089, 27.09184655352419568, 47.04930799450051637 ) ) ;
#9900 = DIRECTION ( 'NONE',  ( 1.000000000000000000, 0.000000000000000000, 0.000000000000000000 ) ) ;
#9901 = FACE_OUTER_BOUND ( 'NONE', #4614, .T. ) ;
#9902 = ORIENTED_EDGE ( 'NONE', *, *, #10857, .F. ) ;
#9903 = VERTEX_POINT ( 'NONE', #22834 ) ;
#9904 = CARTESIAN_POINT ( 'NONE',  ( -43.29088418437023478, 1.073429008971243714, 39.44930799450052916 ) ) ;
#9905 = DIRECTION ( 'NONE',  ( 0.000000000000000000, 0.000000000000000000, -1.000000000000000000 ) ) ;
#9906 = DIRECTION ( 'NONE',  ( -0.000000000000000000, -1.000000000000000000, 0.000000000000000000 ) ) ;
#9907 = EDGE_CURVE ( 'NONE', #25382, #11408, #10213, .T. ) ;
#9908 = CIRCLE ( 'NONE', #18775, 12.36707279061065101 ) ;
#9909 = LINE ( 'NONE', #10241, #14850 ) ;
#9910 = ADVANCED_FACE ( 'NONE', ( #10371, #5289, #27602, #29584, #27766 ), #15974, .T. ) ;
#9911 = ADVANCED_FACE ( 'NONE', ( #7092 ), #30078, .T. ) ;
#9912 = CARTESIAN_POINT ( 'NONE',  ( 72.98472222531829345, 11.92558985988973497, 26.36247558050026640 ) ) ;
#9913 = ORIENTED_EDGE ( 'NONE', *, *, #9263, .T. ) ;
#9914 = ORIENTED_EDGE ( 'NONE', *, *, #4584, .F. ) ;
#9915 = CARTESIAN_POINT ( 'NONE',  ( 5.743216847542398362, 15.11603238453479037, 47.04930799450052348 ) ) ;
#9916 = AXIS2_PLACEMENT_3D ( 'NONE', #9024, #22134, #9191 ) ;
#9917 = AXIS2_PLACEMENT_3D ( 'NONE', #17971, #15359, #25370 ) ;
#9918 = ORIENTED_EDGE ( 'NONE', *, *, #26671, .T. ) ;
#9919 = DIRECTION ( 'NONE',  ( -0.000000000000000000, -1.000000000000000000, 0.000000000000000000 ) ) ;
#9920 = CARTESIAN_POINT ( 'NONE',  ( -9.779715691639985664, -5.937448199248382963, 107.7511683020618420 ) ) ;
#9921 = EDGE_LOOP ( 'NONE', ( #21493, #2190, #15148, #23125, #29047 ) ) ;
#9922 = AXIS2_PLACEMENT_3D ( 'NONE', #18837, #11314, #21302 ) ;
#9923 = CARTESIAN_POINT ( 'NONE',  ( 21.09992658989239089, 29.96664230456641675, 47.04930799450051637 ) ) ;
#9924 = ORIENTED_EDGE ( 'NONE', *, *, #4301, .F. ) ;
#9925 = DIRECTION ( 'NONE',  ( 0.4848096202463627602, 0.8746197071393815303, 0.000000000000000000 ) ) ;
#9926 = AXIS2_PLACEMENT_3D ( 'NONE', #25442, #30541, #17565 ) ;
#9927 = CARTESIAN_POINT ( 'NONE',  ( 40.35612560159030693, 7.881678200673685630, 47.04930799450051637 ) ) ;
#9928 = DIRECTION ( 'NONE',  ( 0.000000000000000000, 0.000000000000000000, -1.000000000000000000 ) ) ;
#9929 = ORIENTED_EDGE ( 'NONE', *, *, #13788, .F. ) ;
#9930 = CARTESIAN_POINT ( 'NONE',  ( 71.74717038377868050, 7.511668073839866011, 75.93045935148319359 ) ) ;
#9931 = CYLINDRICAL_SURFACE ( 'NONE', #17387, 12.62506659569710266 ) ;
#9932 = B_SPLINE_CURVE_WITH_KNOTS ( 'NONE', 3,
 ( #11570, #19258, #18772, #28641, #1717, #26502, #16635, #31597, #26173, #13715, #11733, #19095 ),
 .UNSPECIFIED., .F., .F.,
 ( 4, 2, 2, 2, 2, 4 ),
 ( 0.0003195369756171903726, 0.0003994212195214846047, 0.0004793054634257787826, 0.0005192475853779258445, 0.0005591897073300729605, 0.0006390739512343661085 ),
 .UNSPECIFIED. ) ;
#9933 = CARTESIAN_POINT ( 'NONE',  ( 21.09785597605720753, 14.86454579224779948, 47.04930799450052348 ) ) ;
#9934 = DIRECTION ( 'NONE',  ( 0.000000000000000000, 0.000000000000000000, -1.000000000000000000 ) ) ;
#9935 = CARTESIAN_POINT ( 'NONE',  ( 72.92917568327975175, 6.325917197325471975, 76.79924087496954144 ) ) ;
#9936 = VERTEX_POINT ( 'NONE', #14650 ) ;
#9937 = DIRECTION ( 'NONE',  ( -1.224646799147353207E-16, 0.000000000000000000, -1.000000000000000000 ) ) ;
#9938 = ORIENTED_EDGE ( 'NONE', *, *, #18040, .F. ) ;
#9939 = DIRECTION ( 'NONE',  ( -1.000000000000000000, 0.000000000000000000, 0.000000000000000000 ) ) ;
#9940 = VECTOR ( 'NONE', #23555, 1000.000000000000000 ) ;
#9942 = ADVANCED_FACE ( 'NONE', ( #29917 ), #8143, .T. ) ;
#9941 = TOROIDAL_SURFACE ( 'NONE', #14135, 55.59552431147871232, 1.000000000000000000 ) ;
#9943 = CARTESIAN_POINT ( 'NONE',  ( 21.09992658989238734, 31.59164230456639544, 47.04930799450051637 ) ) ;
#9944 = EDGE_CURVE ( 'NONE', #5139, #3439, #3934, .T. ) ;
#9945 = EDGE_LOOP ( 'NONE', ( #12203, #17606, #4155, #4008 ) ) ;
#9946 = ADVANCED_FACE ( 'NONE', ( #32209 ), #24887, .T. ) ;
#9947 = DIRECTION ( 'NONE',  ( -0.000000000000000000, -1.000000000000000000, -0.000000000000000000 ) ) ;
#9948 = VERTEX_POINT ( 'NONE', #19718 ) ;
#9949 = EDGE_CURVE ( 'NONE', #13157, #8315, #17586, .T. ) ;
#9950 = EDGE_CURVE ( 'NONE', #112, #4576, #29073, .T. ) ;
#9951 = AXIS2_PLACEMENT_3D ( 'NONE', #11236, #3837, #14020 ) ;
#9952 = VERTEX_POINT ( 'NONE', #9881 ) ;
#9953 = AXIS2_PLACEMENT_3D ( 'NONE', #28956, #29113, #8449 ) ;
#9954 = DIRECTION ( 'NONE',  ( 0.000000000000000000, 0.000000000000000000, -1.000000000000000000 ) ) ;
#9955 = CIRCLE ( 'NONE', #12048, 0.1000000000000014905 ) ;
#9956 = AXIS2_PLACEMENT_3D ( 'NONE', #21197, #18577, #1186 ) ;
#9957 = ORIENTED_EDGE ( 'NONE', *, *, #13716, .F. ) ;
#9958 = ORIENTED_EDGE ( 'NONE', *, *, #23868, .T. ) ;
#9959 = CARTESIAN_POINT ( 'NONE',  ( 74.83789960225091420, -1.714651486836151983, 13.37495366749414671 ) ) ;
#9960 = CARTESIAN_POINT ( 'NONE',  ( -44.28695544631906955, -5.935454207752198563, 54.04930799450053058 ) ) ;
#9961 = DIRECTION ( 'NONE',  ( 0.000000000000000000, -0.000000000000000000, -1.000000000000000000 ) ) ;
#9962 = CARTESIAN_POINT ( 'NONE',  ( 48.40423897560355471, 29.16454579224780019, 44.91779129072006072 ) ) ;
#9963 = DIRECTION ( 'NONE',  ( -1.101824276508909887E-16, 1.000000000000000000, -0.000000000000000000 ) ) ;
#9964 = EDGE_CURVE ( 'NONE', #30197, #12497, #9708, .T. ) ;
#9965 = VERTEX_POINT ( 'NONE', #2657 ) ;
#9966 = CARTESIAN_POINT ( 'NONE',  ( -10.12312813457659999, -5.919445383190015342, 104.9138435048736255 ) ) ;
#9967 = ORIENTED_EDGE ( 'NONE', *, *, #4398, .F. ) ;
#9968 = LINE ( 'NONE', #13088, #25931 ) ;
#9969 = LINE ( 'NONE', #30319, #26333 ) ;
#9970 = VERTEX_POINT ( 'NONE', #12688 ) ;
#9971 = CARTESIAN_POINT ( 'NONE',  ( 81.79971628361815306, -5.935345006353228925, 78.03023866733708758 ) ) ;
#9972 = DIRECTION ( 'NONE',  ( 0.000000000000000000, 0.000000000000000000, 1.000000000000000000 ) ) ;
#9973 = AXIS2_PLACEMENT_3D ( 'NONE', #7180, #119, #19314 ) ;
#9974 = AXIS2_PLACEMENT_3D ( 'NONE', #17248, #27264, #14808 ) ;
#9975 = DIRECTION ( 'NONE',  ( -1.000000000000000000, 0.000000000000000000, 0.000000000000000000 ) ) ;
#9976 = DIRECTION ( 'NONE',  ( -1.101824276508909887E-16, 1.000000000000000000, -0.000000000000000000 ) ) ;
#9977 = DIRECTION ( 'NONE',  ( -1.000000000000000000, 0.000000000000000000, 0.000000000000000000 ) ) ;
#9978 = CARTESIAN_POINT ( 'NONE',  ( 45.24946171279598417, 28.42124452788248590, 47.99220971130007030 ) ) ;
#9979 = AXIS2_PLACEMENT_3D ( 'NONE', #30441, #17469, #7958 ) ;
#9980 = DIRECTION ( 'NONE',  ( -1.000000000000000000, 0.000000000000000000, 0.000000000000000000 ) ) ;
#9981 = CARTESIAN_POINT ( 'NONE',  ( 8.698509210239574685, 30.59164230456639544, 47.04930799450051637 ) ) ;
#9982 = ORIENTED_EDGE ( 'NONE', *, *, #31237, .T. ) ;
#9983 = AXIS2_PLACEMENT_3D ( 'NONE', #8578, #28757, #3972 ) ;
#9984 = CARTESIAN_POINT ( 'NONE',  ( 21.09785597605720753, -5.098646251524523443, 47.04930799450052348 ) ) ;
#9985 = AXIS2_PLACEMENT_3D ( 'NONE', #2832, #22699, #27951 ) ;
#9986 = DIRECTION ( 'NONE',  ( -1.000000000000000000, -1.101824276508909887E-16, 0.000000000000000000 ) ) ;
#9987 = ORIENTED_EDGE ( 'NONE', *, *, #21170, .T. ) ;
#9988 = DIRECTION ( 'NONE',  ( -0.9612616959383193382, -0.2756373558169973870, -8.795445018804928853E-19 ) ) ;
#9989 = ORIENTED_EDGE ( 'NONE', *, *, #28441, .F. ) ;
#9990 = EDGE_CURVE ( 'NONE', #18712, #2479, #28577, .T. ) ;
#9991 = ORIENTED_EDGE ( 'NONE', *, *, #12950, .T. ) ;
#9992 = DIRECTION ( 'NONE',  ( -0.2250569586005335410, 0.7848668881104262640, -0.5773502691896259531 ) ) ;
#9993 = EDGE_CURVE ( 'NONE', #14845, #11669, #16512, .T. ) ;
#9994 = CIRCLE ( 'NONE', #31984, 1.142135311067127512 ) ;
#9995 = VERTEX_POINT ( 'NONE', #13646 ) ;
#9996 = AXIS2_PLACEMENT_3D ( 'NONE', #20899, #23041, #10422 ) ;
#9997 = VECTOR ( 'NONE', #14216, 1000.000000000000000 ) ;
#9998 = AXIS2_PLACEMENT_3D ( 'NONE', #31047, #8556, #18545 ) ;
#9999 = ORIENTED_EDGE ( 'NONE', *, *, #18120, .F. ) ;
#10000 = CIRCLE ( 'NONE', #13678, 12.36707279061065101 ) ;
#10001 = CARTESIAN_POINT ( 'NONE',  ( 45.91943065483079778, 23.03451764446789696, 47.32022353109342561 ) ) ;
#10002 = AXIS2_PLACEMENT_3D ( 'NONE', #15751, #28881, #8530 ) ;
#10003 = CIRCLE ( 'NONE', #24664, 54.30000000000000426 ) ;
#10004 = ADVANCED_FACE ( 'NONE', ( #20363 ), #20715, .T. ) ;
#10005 = VERTEX_POINT ( 'NONE', #30881 ) ;
#10006 = CARTESIAN_POINT ( 'NONE',  ( 21.09785597605719332, 7.237299147902269247, 47.04930799450051637 ) ) ;
#10007 = CARTESIAN_POINT ( 'NONE',  ( 21.09992658989239089, 26.34164230456639899, 47.04930799450051637 ) ) ;
#10008 = DIRECTION ( 'NONE',  ( -2.779292025043186742E-18, 1.288349127009862365E-17, -1.000000000000000000 ) ) ;
#10009 = CARTESIAN_POINT ( 'NONE',  ( 49.49063479933183629, 26.61291119454915588, 47.17357720316391578 ) ) ;
#10010 = EDGE_CURVE ( 'NONE', #24256, #14178, #19094, .T. ) ;
#10011 = ORIENTED_EDGE ( 'NONE', *, *, #27073, .T. ) ;
#10012 = EDGE_LOOP ( 'NONE', ( #19434, #16526, #19649, #12978 ) ) ;
#10013 = CARTESIAN_POINT ( 'NONE',  ( -39.85048242108726413, 2.742214340073605428, 49.04930799450051637 ) ) ;
#10014 = AXIS2_PLACEMENT_3D ( 'NONE', #27193, #17176, #29336 ) ;
#10015 = EDGE_CURVE ( 'NONE', #9681, #18953, #12336, .T. ) ;
#10016 = ORIENTED_EDGE ( 'NONE', *, *, #9031, .F. ) ;
#10017 = CARTESIAN_POINT ( 'NONE',  ( 21.09785597605720753, 14.86454579224779948, 47.04930799450052348 ) ) ;
#10018 = DIRECTION ( 'NONE',  ( -1.101824276508909887E-16, 1.000000000000000000, -0.000000000000000000 ) ) ;
#10019 = DIRECTION ( 'NONE',  ( -0.6184495258776567805, 0.3428121700606641120, -0.7071067811865474617 ) ) ;
#10020 = DIRECTION ( 'NONE',  ( -0.2756373558169974980, 0.9612616959383193382, 1.315048337272770589E-17 ) ) ;
#10021 = CARTESIAN_POINT ( 'NONE',  ( 5.821908465877174699, 15.23758267881771111, 47.04930799450052348 ) ) ;
#10022 = ORIENTED_EDGE ( 'NONE', *, *, #23825, .F. ) ;
#10023 = EDGE_LOOP ( 'NONE', ( #366, #19407, #22453, #31264, #31257, #7238 ) ) ;
#10024 = DIRECTION ( 'NONE',  ( -0.000000000000000000, -1.000000000000000000, 0.000000000000000000 ) ) ;
#10025 = LINE ( 'NONE', #19855, #20843 ) ;
#10026 = DIRECTION ( 'NONE',  ( -1.101824276508909887E-16, 1.000000000000000000, -0.000000000000000000 ) ) ;
#10027 = ORIENTED_EDGE ( 'NONE', *, *, #19334, .T. ) ;
#10028 = CARTESIAN_POINT ( 'NONE',  ( 52.14539454897627024, -5.936967987714539596, 107.4238135535513976 ) ) ;
#10029 = VECTOR ( 'NONE', #647, 1000.000000000000000 ) ;
#10030 = ORIENTED_EDGE ( 'NONE', *, *, #29521, .T. ) ;
#10031 = FACE_OUTER_BOUND ( 'NONE', #19331, .T. ) ;
#10032 = AXIS2_PLACEMENT_3D ( 'NONE', #5044, #15052, #5200 ) ;
#10033 = DIRECTION ( 'NONE',  ( 0.000000000000000000, -0.8746197071393925215, -0.4848096202463429982 ) ) ;
#10034 = EDGE_CURVE ( 'NONE', #11721, #3679, #30394, .T. ) ;
#10035 = AXIS2_PLACEMENT_3D ( 'NONE', #32266, #24706, #2223 ) ;
#10036 = DIRECTION ( 'NONE',  ( 0.000000000000000000, 1.000000000000000000, -0.000000000000000000 ) ) ;
#10037 = CIRCLE ( 'NONE', #584, 0.1000000000000006301 ) ;
#10038 = EDGE_LOOP ( 'NONE', ( #3237, #12248, #18229, #25245 ) ) ;
#10039 = VERTEX_POINT ( 'NONE', #5771 ) ;
#10040 = EDGE_CURVE ( 'NONE', #17834, #21141, #11022, .T. ) ;
#10041 = CARTESIAN_POINT ( 'NONE',  ( 21.09992658989239089, 27.97145308207318237, 47.04930799450051637 ) ) ;
#10042 = DIRECTION ( 'NONE',  ( 7.871877887341991227E-17, -0.7660444431189775694, 0.6427876096865398070 ) ) ;
#10043 = CARTESIAN_POINT ( 'NONE',  ( 48.40186567930498285, 26.11618040159426357, 45.03923535223908203 ) ) ;
#10044 = EDGE_CURVE ( 'NONE', #32358, #3661, #25466, .T. ) ;
#10045 = ORIENTED_EDGE ( 'NONE', *, *, #12235, .T. ) ;
#10046 = CIRCLE ( 'NONE', #3208, 0.1000000000000020595 ) ;
#10047 = DIRECTION ( 'NONE',  ( -1.000000000000000000, 0.000000000000000000, 0.000000000000000000 ) ) ;
#10048 = CIRCLE ( 'NONE', #18925, 0.9999999999999956701 ) ;
#10049 = FACE_OUTER_BOUND ( 'NONE', #28338, .T. ) ;
#10050 = DIRECTION ( 'NONE',  ( 0.000000000000000000, 0.000000000000000000, -1.000000000000000000 ) ) ;
#10051 = CARTESIAN_POINT ( 'NONE',  ( 51.92400919103565116, -5.935454207752198563, -11.03616215687537583 ) ) ;
#10052 = ADVANCED_FACE ( 'NONE', ( #3457 ), #25927, .F. ) ;
#10053 = CARTESIAN_POINT ( 'NONE',  ( 45.41653742442152719, 20.36454579224779948, 43.75337596730032175 ) ) ;
#10054 = ADVANCED_FACE ( 'NONE', ( #17913 ), #24356, .F. ) ;
#10055 = DIRECTION ( 'NONE',  ( -0.2756373558169959437, 0.9612616959383197823, 0.000000000000000000 ) ) ;
#10056 = DIRECTION ( 'NONE',  ( -1.000000000000000000, 0.000000000000000000, 0.000000000000000000 ) ) ;
#10057 = DIRECTION ( 'NONE',  ( 0.000000000000000000, 0.000000000000000000, 1.000000000000000000 ) ) ;
#10058 = CARTESIAN_POINT ( 'NONE',  ( 21.09785597605719332, 25.56454579224779167, 47.04930799450051637 ) ) ;
#10059 = FACE_OUTER_BOUND ( 'NONE', #7890, .T. ) ;
#10060 = CARTESIAN_POINT ( 'NONE',  ( 45.84097905237065618, 22.86454579224779948, 48.98672734302541443 ) ) ;
#10061 =( LENGTH_UNIT ( ) NAMED_UNIT ( * ) SI_UNIT ( .MILLI., .METRE. ) );
#10062 = EDGE_LOOP ( 'NONE', ( #16715, #11502, #26600, #2459 ) ) ;
#10063 = EDGE_LOOP ( 'NONE', ( #23895, #16327, #25537, #1102 ) ) ;
#10064 = FACE_OUTER_BOUND ( 'NONE', #12389, .T. ) ;
#10065 = CIRCLE ( 'NONE', #26823, 0.1250000000000001110 ) ;
#10066 = DIRECTION ( 'NONE',  ( 1.000000000000000000, 0.000000000000000000, 0.000000000000000000 ) ) ;
#10067 = CARTESIAN_POINT ( 'NONE',  ( -36.05908242950876286, -5.586586463951790371, 14.92569346413818998 ) ) ;
#10068 = CARTESIAN_POINT ( 'NONE',  ( -40.15225626691278649, 6.735663658092487793, 53.64930799450051779 ) ) ;
#10069 = VERTEX_POINT ( 'NONE', #30723 ) ;
#10070 = CARTESIAN_POINT ( 'NONE',  ( 21.09785597605719332, 30.56554579224779644, 18.54930799450051282 ) ) ;
#10071 = FACE_OUTER_BOUND ( 'NONE', #5003, .T. ) ;
#10072 = CARTESIAN_POINT ( 'NONE',  ( 45.83851142336192908, 10.95964320463250630, -3.629547344415893662 ) ) ;
#10073 = ORIENTED_EDGE ( 'NONE', *, *, #32357, .T. ) ;
#10074 = VERTEX_POINT ( 'NONE', #25782 ) ;
#10075 = FACE_OUTER_BOUND ( 'NONE', #21476, .T. ) ;
#10076 = CARTESIAN_POINT ( 'NONE',  ( 45.35708200440645044, 26.99118040159426357, 45.92000246470679770 ) ) ;
#10077 = CARTESIAN_POINT ( 'NONE',  ( -5.602943079677954685, 9.702389020015065313, -3.351769630585352377 ) ) ;
#10078 = CARTESIAN_POINT ( 'NONE',  ( -41.63422246745999189, 11.51531537899137447, 56.14611646155296398 ) ) ;
#10079 = VECTOR ( 'NONE', #30045, 1000.000000000000000 ) ;
#10080 = AXIS2_PLACEMENT_3D ( 'NONE', #13207, #718, #3163 ) ;
#10081 = DIRECTION ( 'NONE',  ( 0.000000000000000000, -0.000000000000000000, -1.000000000000000000 ) ) ;
#10082 = AXIS2_PLACEMENT_3D ( 'NONE', #24332, #1858, #28953 ) ;
#10083 = ORIENTED_EDGE ( 'NONE', *, *, #3033, .T. ) ;
#10084 = ADVANCED_FACE ( 'NONE', ( #18389 ), #9163, .T. ) ;
#10085 = DIRECTION ( 'NONE',  ( -1.000000000000000000, -1.101824276508909764E-16, 0.000000000000000000 ) ) ;
#10086 = AXIS2_PLACEMENT_3D ( 'NONE', #16975, #21741, #7309 ) ;
#10087 = EDGE_CURVE ( 'NONE', #15339, #31154, #27512, .T. ) ;
#10088 = EDGE_LOOP ( 'NONE', ( #27827, #6093 ) ) ;
#10089 = CIRCLE ( 'NONE', #28430, 72.21005050633880273 ) ;
#10090 = DIRECTION ( 'NONE',  ( -1.101824276508909887E-16, 1.000000000000000000, -0.000000000000000000 ) ) ;
#10091 = CARTESIAN_POINT ( 'NONE',  ( -9.779715691639985664, -5.937448199248382963, 107.4930705127871562 ) ) ;
#10092 = ADVANCED_FACE ( 'NONE', ( #28419 ), #25421, .T. ) ;
#10093 = TOROIDAL_SURFACE ( 'NONE', #135, 12.61792373059899752, 0.1250000000000005274 ) ;
#10094 = ORIENTED_EDGE ( 'NONE', *, *, #17862, .F. ) ;
#10095 = CARTESIAN_POINT ( 'NONE',  ( -40.82429435450200828, 8.450784283921491280, 34.58262810048215385 ) ) ;
#10096 = EDGE_LOOP ( 'NONE', ( #11120, #30438, #30015, #18816 ) ) ;
#10097 = EDGE_CURVE ( 'NONE', #23467, #30184, #11280, .T. ) ;
#10098 = FACE_OUTER_BOUND ( 'NONE', #2920, .T. ) ;
#10099 = CARTESIAN_POINT ( 'NONE',  ( 33.50134396954519644, 31.34164230456639544, 47.04930799450051637 ) ) ;
#10100 = AXIS2_PLACEMENT_3D ( 'NONE', #2437, #8016, #12453 ) ;
#10101 = CARTESIAN_POINT ( 'NONE',  ( -40.69520067770175586, 6.787173244583783571, 39.45492316879074934 ) ) ;
#10102 = ORIENTED_EDGE ( 'NONE', *, *, #18733, .T. ) ;
#10103 = CARTESIAN_POINT ( 'NONE',  ( 72.99627843240752156, 2.793366809690255526, 78.95322653079809072 ) ) ;
#10104 = DIRECTION ( 'NONE',  ( -0.7936353835927094647, 0.4399192766786362285, -0.4202545751282172337 ) ) ;
#10105 = DIRECTION ( 'NONE',  ( 0.2756373558169947779, -0.9612616959383200044, 0.000000000000000000 ) ) ;
#10106 = DIRECTION ( 'NONE',  ( 0.8746197071393925215, -0.4848096202463429982, -8.676864087101708112E-18 ) ) ;
#10107 = DIRECTION ( 'NONE',  ( 0.000000000000000000, 0.000000000000000000, -1.000000000000000000 ) ) ;
#10108 = ORIENTED_EDGE ( 'NONE', *, *, #4991, .T. ) ;
#10109 = CARTESIAN_POINT ( 'NONE',  ( -43.38408989745150990, 1.111547985471240008, 53.64930799450051779 ) ) ;
#10110 = DIRECTION ( 'NONE',  ( -1.000000000000000000, 0.000000000000000000, 0.000000000000000000 ) ) ;
#10111 = ORIENTED_EDGE ( 'NONE', *, *, #22862, .F. ) ;
#10112 = DIRECTION ( 'NONE',  ( -1.101824276508909887E-16, 1.000000000000000000, -0.000000000000000000 ) ) ;
#10113 = DIRECTION ( 'NONE',  ( 0.000000000000000000, 0.000000000000000000, -1.000000000000000000 ) ) ;
#10114 = CIRCLE ( 'NONE', #13755, 5.099019513592789821 ) ;
#10115 = VERTEX_POINT ( 'NONE', #15934 ) ;
#10116 = CARTESIAN_POINT ( 'NONE',  ( 8.823509210239532052, 26.59164230456639899, 47.04930799450051637 ) ) ;
#10117 = VERTEX_POINT ( 'NONE', #30562 ) ;
#10118 = TOROIDAL_SURFACE ( 'NONE', #17973, 39.69941114636694834, 0.3000000000000000444 ) ;
#10119 = ORIENTED_EDGE ( 'NONE', *, *, #11648, .T. ) ;
#10120 = TOROIDAL_SURFACE ( 'NONE', #14309, 20.27643559902816861, 0.2000000000000001499 ) ;
#10121 = CARTESIAN_POINT ( 'NONE',  ( 8.698509210239564027, 29.59164230456639899, 47.04930799450051637 ) ) ;
#10122 = CARTESIAN_POINT ( 'NONE',  ( 21.09785597605719687, 25.56454579224779167, 15.74930799450049257 ) ) ;
#10123 = EDGE_CURVE ( 'NONE', #9745, #16786, #13485, .T. ) ;
#10124 = ORIENTED_EDGE ( 'NONE', *, *, #6591, .F. ) ;
#10125 = ORIENTED_EDGE ( 'NONE', *, *, #20234, .T. ) ;
#10126 = DIRECTION ( 'NONE',  ( -1.000000000000000000, 0.000000000000000000, 0.000000000000000000 ) ) ;
#10127 = EDGE_CURVE ( 'NONE', #28880, #16169, #28563, .T. ) ;
#10128 = CARTESIAN_POINT ( 'NONE',  ( -43.42571077420251413, -4.056638831137751922, 52.04930799450050216 ) ) ;
#10129 = EDGE_CURVE ( 'NONE', #13517, #2319, #30146, .T. ) ;
#10130 = DIRECTION ( 'NONE',  ( -0.000000000000000000, 1.000000000000000000, -0.000000000000000000 ) ) ;
#10131 = DIRECTION ( 'NONE',  ( 1.000000000000000000, 0.000000000000000000, 0.000000000000000000 ) ) ;
#10132 = AXIS2_PLACEMENT_3D ( 'NONE', #30157, #9476, #24399 ) ;
#10133 = CARTESIAN_POINT ( 'NONE',  ( 21.09992658989238734, 32.34143805560860585, 47.04930799450051637 ) ) ;
#10134 = ORIENTED_EDGE ( 'NONE', *, *, #10015, .F. ) ;
#10135 = ORIENTED_EDGE ( 'NONE', *, *, #29541, .T. ) ;
#10136 = CARTESIAN_POINT ( 'NONE',  ( 80.69365197279370250, -5.938447472589718501, 16.00391517297267185 ) ) ;
#10137 = VERTEX_POINT ( 'NONE', #3779 ) ;
#10138 = CARTESIAN_POINT ( 'NONE',  ( 21.09785597605719332, 25.76454579224779806, 60.04930799450051637 ) ) ;
#10139 = CARTESIAN_POINT ( 'NONE',  ( 21.09785597605719332, 13.06454579224779877, 47.04930799450051637 ) ) ;
#10140 = CARTESIAN_POINT ( 'NONE',  ( 8.698509210239516065, 25.09164230456639899, 47.04930799450051637 ) ) ;
#10141 = CARTESIAN_POINT ( 'NONE',  ( -33.00214402394279745, 14.86454579224779948, 47.04930799450052348 ) ) ;
#10142 = DIRECTION ( 'NONE',  ( -0.000000000000000000, -1.000000000000000000, 0.000000000000000000 ) ) ;
#10143 = CARTESIAN_POINT ( 'NONE',  ( 48.40186567930498285, 28.12957786121581805, 45.03923535223908203 ) ) ;
#10144 = TOROIDAL_SURFACE ( 'NONE', #2263, 32.50000000000000000, 1.000000000000000888 ) ;
#10145 =( BOUNDED_CURVE ( )  B_SPLINE_CURVE ( 3, ( #28435, #3637, #11195, #19537 ),
 .UNSPECIFIED., .F., .F. ) 
 B_SPLINE_CURVE_WITH_KNOTS ( ( 4, 4 ),
 ( 4.712388980384698556, 5.497787143782102426 ),
 .UNSPECIFIED. ) 
 CURVE ( )  GEOMETRIC_REPRESENTATION_ITEM ( )  RATIONAL_B_SPLINE_CURVE ( ( 1.000000000000000000, 0.9492530216741968951, 0.9492530216741968951, 1.000000000000000000 ) ) 
 REPRESENTATION_ITEM ( '' )  );
#10146 = CIRCLE ( 'NONE', #19561, 65.75844861871132707 ) ;
#10147 = DIRECTION ( 'NONE',  ( -0.4848096202463430537, -0.8746197071393926326, -9.920727850371701658E-18 ) ) ;
#10148 = CARTESIAN_POINT ( 'NONE',  ( 8.698509210239571132, 30.34164230456639544, 47.04930799450051637 ) ) ;
#10149 = VERTEX_POINT ( 'NONE', #4272 ) ;
#10150 = CARTESIAN_POINT ( 'NONE',  ( 21.09992658989239089, 26.09164230456639899, 47.04930799450051637 ) ) ;
#10151 = ORIENTED_EDGE ( 'NONE', *, *, #30846, .T. ) ;
#10152 = CARTESIAN_POINT ( 'NONE',  ( 21.09785597605720753, 14.86454579224779948, 47.04930799450052348 ) ) ;
#10153 = EDGE_LOOP ( 'NONE', ( #4529, #24495 ) ) ;
#10154 = ORIENTED_EDGE ( 'NONE', *, *, #22616, .F. ) ;
#10155 = DIRECTION ( 'NONE',  ( -0.000000000000000000, -1.000000000000000000, 0.000000000000000000 ) ) ;
#10156 = EDGE_LOOP ( 'NONE', ( #7692, #3702, #32112, #18463 ) ) ;
#10157 = TOROIDAL_SURFACE ( 'NONE', #16950, 12.40141737965280022, 0.1249999999999992228 ) ;
#10158 = EDGE_CURVE ( 'NONE', #5208, #26617, #14417, .T. ) ;
#10159 =( REPRESENTATION_RELATIONSHIP ('NONE','NONE', #20382, #5723 ) REPRESENTATION_RELATIONSHIP_WITH_TRANSFORMATION ( #23767 )SHAPE_REPRESENTATION_RELATIONSHIP( ) );
#10160 = CIRCLE ( 'NONE', #31639, 12.62506659569710266 ) ;
#10161 = AXIS2_PLACEMENT_3D ( 'NONE', #15544, #17522, #32306 ) ;
#10162 = EDGE_LOOP ( 'NONE', ( #16315, #27576, #17215, #30624 ) ) ;
#10163 = CARTESIAN_POINT ( 'NONE',  ( 46.33206787849857022, 22.99884124225578574, 48.22973596570440691 ) ) ;
#10164 = ORIENTED_EDGE ( 'NONE', *, *, #3362, .F. ) ;
#10165 = EDGE_CURVE ( 'NONE', #4564, #5895, #19648, .T. ) ;
#10166 = EDGE_CURVE ( 'NONE', #4643, #15925, #259, .T. ) ;
#10167 = EDGE_CURVE ( 'NONE', #29811, #10189, #22790, .T. ) ;
#10168 = CIRCLE ( 'NONE', #28521, 0.1000000000000018235 ) ;
#10169 = CARTESIAN_POINT ( 'NONE',  ( -40.11967773290336226, 9.763195579837789850, 35.54930799450052348 ) ) ;
#10170 = CARTESIAN_POINT ( 'NONE',  ( -9.884435415115211399, -5.935653941159259261, -13.43318508042229098 ) ) ;
#10171 = ADVANCED_FACE ( 'NONE', ( #31363, #11491, #29056, #4098, #29381, #11829 ), #11664, .F. ) ;
#10172 = CARTESIAN_POINT ( 'NONE',  ( 48.83862994770794330, 27.25457786121581805, 48.17861352429476796 ) ) ;
#10173 = ORIENTED_EDGE ( 'NONE', *, *, #9225, .T. ) ;
#10174 = ADVANCED_FACE ( 'NONE', ( #31527 ), #18865, .F. ) ;
#10175 = VERTEX_POINT ( 'NONE', #13802 ) ;
#10176 = LINE ( 'NONE', #25266, #12724 ) ;
#10177 = VERTEX_POINT ( 'NONE', #31204 ) ;
#10178 = DIRECTION ( 'NONE',  ( -0.1949050434465268433, 0.6797146636928677044, 0.7071067811865470176 ) ) ;
#10179 = FACE_OUTER_BOUND ( 'NONE', #14129, .T. ) ;
#10180 = CARTESIAN_POINT ( 'NONE',  ( 51.92400919103565116, -5.935454207752198563, -12.64839579672098679 ) ) ;
#10181 = CARTESIAN_POINT ( 'NONE',  ( 52.46847310473540915, -5.884593569754288822, -12.16357552036296141 ) ) ;
#10182 = CARTESIAN_POINT ( 'NONE',  ( 45.35708200440645044, 25.50457786121582515, 45.92000246470680480 ) ) ;
#10183 = APPLICATION_PROTOCOL_DEFINITION ( 'draft international standard', 'automotive_design', 1998, #23750 ) ;
#10184 = ORIENTED_EDGE ( 'NONE', *, *, #2716, .F. ) ;
#10185 = ORIENTED_EDGE ( 'NONE', *, *, #27616, .F. ) ;
#10186 = DIRECTION ( 'NONE',  ( -0.4544104193609937448, 0.000000000000000000, -0.8907924397839072084 ) ) ;
#10187 = CARTESIAN_POINT ( 'NONE',  ( 48.23388202445966044, 29.05087065737811969, 49.27628909396056400 ) ) ;
#10188 = CARTESIAN_POINT ( 'NONE',  ( -9.728297238921257417, -5.935454207752202116, 107.6607613508313648 ) ) ;
#10189 = VERTEX_POINT ( 'NONE', #8711 ) ;
#10190 = CARTESIAN_POINT ( 'NONE',  ( 48.40186567930497574, 28.21618040159426499, 45.03923535223908203 ) ) ;
#10191 = ORIENTED_EDGE ( 'NONE', *, *, #28606, .F. ) ;
#10192 = DIRECTION ( 'NONE',  ( -1.000000000000000000, 0.000000000000000000, 0.000000000000000000 ) ) ;
#10193 = LINE ( 'NONE', #12668, #12530 ) ;
#10194 = CARTESIAN_POINT ( 'NONE',  ( 33.46699938050303302, 38.56284415653841791, 47.04930799450051637 ) ) ;
#10195 = EDGE_CURVE ( 'NONE', #18016, #17431, #28544, .T. ) ;
#10196 = EDGE_CURVE ( 'NONE', #2614, #30294, #2837, .T. ) ;
#10197 = ORIENTED_EDGE ( 'NONE', *, *, #11653, .F. ) ;
#10198 = AXIS2_PLACEMENT_3D ( 'NONE', #11695, #29243, #21350 ) ;
#10199 = ORIENTED_EDGE ( 'NONE', *, *, #12260, .F. ) ;
#10200 = AXIS2_PLACEMENT_3D ( 'NONE', #23401, #20930, #31278 ) ;
#10201 = DIRECTION ( 'NONE',  ( 0.000000000000000000, 0.000000000000000000, 1.000000000000000000 ) ) ;
#10202 = CARTESIAN_POINT ( 'NONE',  ( 21.09785597605719687, 24.86454579224780304, 27.04930799450051637 ) ) ;
#10204 = CARTESIAN_POINT ( 'NONE',  ( 46.00908685603034343, 25.53284706826093498, 44.91496614357595263 ) ) ;
#10203 = AXIS2_PLACEMENT_3D ( 'NONE', #20047, #5117, #24976 ) ;
#10205 = AXIS2_PLACEMENT_3D ( 'NONE', #12831, #22823, #30382 ) ;
#10206 = ORIENTED_EDGE ( 'NONE', *, *, #22890, .F. ) ;
#10207 = CARTESIAN_POINT ( 'NONE',  ( -38.65545646816406133, 11.92829597396328012, 69.12115383893792853 ) ) ;
#10208 = DIRECTION ( 'NONE',  ( -1.000000000000000000, 0.000000000000000000, 0.000000000000000000 ) ) ;
#10209 = DIRECTION ( 'NONE',  ( -1.101824276508909887E-16, 1.000000000000000000, -0.000000000000000000 ) ) ;
#10210 = ADVANCED_FACE ( 'NONE', ( #31688 ), #1314, .F. ) ;
#10211 = FACE_OUTER_BOUND ( 'NONE', #379, .T. ) ;
#10212 = CARTESIAN_POINT ( 'NONE',  ( 9.016997203727582288, 34.59164230456639899, 46.73295957419995261 ) ) ;
#10213 = LINE ( 'NONE', #24977, #10746 ) ;
#10214 = CARTESIAN_POINT ( 'NONE',  ( -42.22138300640814634, 14.68176690255379313, 38.09144330556765112 ) ) ;
#10215 = DIRECTION ( 'NONE',  ( -1.000000000000000000, 0.000000000000000000, 0.000000000000000000 ) ) ;
#10216 = CARTESIAN_POINT ( 'NONE',  ( 21.09785597605720753, 14.36454579224779948, 47.04930799450052348 ) ) ;
#10217 = DIRECTION ( 'NONE',  ( -0.4848096202463429427, -0.8746197071393925215, 2.352477780477436787E-16 ) ) ;
#10218 = CARTESIAN_POINT ( 'NONE',  ( 8.823509210239517842, 25.34164230456639899, 47.04930799450051637 ) ) ;
#10219 = SURFACE_SIDE_STYLE ('',( #354 ) ) ;
#10220 = ORIENTED_EDGE ( 'NONE', *, *, #9674, .T. ) ;
#10221 = ORIENTED_EDGE ( 'NONE', *, *, #2248, .T. ) ;
#10222 = DIRECTION ( 'NONE',  ( -1.101824276508909887E-16, 1.000000000000000000, -0.000000000000000000 ) ) ;
#10223 = CARTESIAN_POINT ( 'NONE',  ( 48.28307451434712760, 25.08930407213309977, 44.81510409515678361 ) ) ;
#10224 = CARTESIAN_POINT ( 'NONE',  ( -40.18454328187963398, 7.548069831825862330, 53.80788663826320573 ) ) ;
#10225 = CARTESIAN_POINT ( 'NONE',  ( 49.10800547237058566, 8.510833471476312084, 97.55326967204440791 ) ) ;
#10226 = AXIS2_PLACEMENT_3D ( 'NONE', #3774, #14118, #29049 ) ;
#10227 = ORIENTED_EDGE ( 'NONE', *, *, #12686, .F. ) ;
#10228 = DIRECTION ( 'NONE',  ( 0.9612616959383221138, 0.2756373558169876170, 0.000000000000000000 ) ) ;
#10229 = CARTESIAN_POINT ( 'NONE',  ( 8.474859994195286461, 29.09184655352418858, 47.04930799450051637 ) ) ;
#10230 = CARTESIAN_POINT ( 'NONE',  ( 33.37634396954526750, 24.59164230456639544, 47.04930799450051637 ) ) ;
#10231 = EDGE_CURVE ( 'NONE', #15416, #13009, #29096, .T. ) ;
#10232 = ORIENTED_EDGE ( 'NONE', *, *, #24192, .T. ) ;
#10233 = ORIENTED_EDGE ( 'NONE', *, *, #24724, .F. ) ;
#10235 = AXIS2_PLACEMENT_3D ( 'NONE', #7431, #14974, #17423 ) ;
#10234 = LINE ( 'NONE', #13018, #24637 ) ;
#10236 = CARTESIAN_POINT ( 'NONE',  ( 47.20547626766766314, 25.47451373492760140, 44.97710074790751378 ) ) ;
#10237 = CIRCLE ( 'NONE', #2360, 30.00000000000000000 ) ;
#10238 = CIRCLE ( 'NONE', #18062, 0.1250000000000001110 ) ;
#10239 = DIRECTION ( 'NONE',  ( 0.8746197071393926326, -0.4848096202463430537, -8.676864087101709653E-18 ) ) ;
#10240 = ADVANCED_FACE ( 'NONE', ( #16410 ), #21489, .T. ) ;
#10241 = CARTESIAN_POINT ( 'NONE',  ( 21.09785597605719332, 25.56454579224779167, 60.04930799450051637 ) ) ;
#10242 = AXIS2_PLACEMENT_3D ( 'NONE', #19341, #2121, #29538 ) ;
#10243 = CARTESIAN_POINT ( 'NONE',  ( 21.09785597605719332, -9.935454207752199451, -20.95069200549946231 ) ) ;
#10244 = EDGE_CURVE ( 'NONE', #30572, #11324, #1641, .T. ) ;
#10245 = ADVANCED_FACE ( 'NONE', ( #9197 ), #24288, .F. ) ;
#10246 = ORIENTED_EDGE ( 'NONE', *, *, #10487, .F. ) ;
#10247 = EDGE_CURVE ( 'NONE', #14930, #7136, #8601, .T. ) ;
#10248 = CARTESIAN_POINT ( 'NONE',  ( -42.66751614955960292, 15.14923148629343430, 38.54930799450052348 ) ) ;
#10249 = ORIENTED_EDGE ( 'NONE', *, *, #26494, .F. ) ;
#10250 = CIRCLE ( 'NONE', #5540, 12.27641737965286062 ) ;
#10251 = CARTESIAN_POINT ( 'NONE',  ( -40.69343167531472005, 8.234387981831401859, 54.54930799450051637 ) ) ;
#10252 = DIRECTION ( 'NONE',  ( -1.101824276508909887E-16, 1.000000000000000000, -0.000000000000000000 ) ) ;
#10253 = VECTOR ( 'NONE', #28691, 1000.000000000000000 ) ;
#10254 = ADVANCED_FACE ( 'NONE', ( #2135 ), #19847, .F. ) ;
#10255 = TOROIDAL_SURFACE ( 'NONE', #2883, 12.61792373059858896, 0.1250000000000002220 ) ;
#10256 = AXIS2_PLACEMENT_3D ( 'NONE', #4799, #31283, #11411 ) ;
#10257 = ORIENTED_EDGE ( 'NONE', *, *, #8447, .T. ) ;
#10258 = CARTESIAN_POINT ( 'NONE',  ( -42.50976151518962354, 14.59907569580870224, 38.09144330556765112 ) ) ;
#10259 = VERTEX_POINT ( 'NONE', #17553 ) ;
#10260 = VECTOR ( 'NONE', #21199, 1000.000000000000114 ) ;
#10261 = CARTESIAN_POINT ( 'NONE',  ( 80.79555976727768041, -5.935454207752198563, 77.87546120947919803 ) ) ;
#10262 = CARTESIAN_POINT ( 'NONE',  ( -41.88090303775678791, 13.82677487427666385, 59.46671529104048659 ) ) ;
#10263 = CARTESIAN_POINT ( 'NONE',  ( 21.09992658989238734, 38.56284415653841791, 47.04930799450051637 ) ) ;
#10264 = CARTESIAN_POINT ( 'NONE',  ( -40.69575244446413365, 6.786495028291348319, 39.45034024385534366 ) ) ;
#10265 = ORIENTED_EDGE ( 'NONE', *, *, #13638, .F. ) ;
#10266 = LINE ( 'NONE', #31087, #24405 ) ;
#10267 = FACE_OUTER_BOUND ( 'NONE', #9632, .T. ) ;
#10268 = CARTESIAN_POINT ( 'NONE',  ( 81.65601105638101842, -5.935667572904986145, 77.88056461575189360 ) ) ;
#10269 = CARTESIAN_POINT ( 'NONE',  ( 21.09992658989239089, 29.84143805560861296, 47.04930799450051637 ) ) ;
#10270 = DIRECTION ( 'NONE',  ( -1.188208965918165239E-16, -1.880121038077813132E-16, -1.000000000000000000 ) ) ;
#10271 = ORIENTED_EDGE ( 'NONE', *, *, #3520, .T. ) ;
#10272 = DIRECTION ( 'NONE',  ( -0.000000000000000000, -1.000000000000000000, -0.000000000000000000 ) ) ;
#10273 = DIRECTION ( 'NONE',  ( 0.000000000000000000, 0.000000000000000000, 1.000000000000000000 ) ) ;
#10274 = EDGE_CURVE ( 'NONE', #24129, #18133, #17060, .T. ) ;
#10275 = EDGE_LOOP ( 'NONE', ( #8691, #2686, #8339, #9957, #23919, #28231 ) ) ;
#10276 = LINE ( 'NONE', #8284, #15201 ) ;
#10277 = DIRECTION ( 'NONE',  ( -1.101824276508909887E-16, 1.000000000000000000, -0.000000000000000000 ) ) ;
#10278 = EDGE_CURVE ( 'NONE', #4416, #3138, #11812, .T. ) ;
#10279 = CARTESIAN_POINT ( 'NONE',  ( 21.09992658989238734, 38.56284415653841791, 47.04930799450051637 ) ) ;
#10280 = ORIENTED_EDGE ( 'NONE', *, *, #30512, .F. ) ;
#10281 = CARTESIAN_POINT ( 'NONE',  ( -40.61178118339597631, 9.038025460530262123, 57.95249952744806166 ) ) ;
#10282 = ORIENTED_EDGE ( 'NONE', *, *, #15268, .F. ) ;
#10283 = AXIS2_PLACEMENT_3D ( 'NONE', #16776, #26799, #4314 ) ;
#10284 = STYLED_ITEM ( 'NONE', ( #16126 ), #11641 ) ;
#10285 = EDGE_CURVE ( 'NONE', #11145, #16663, #4407, .T. ) ;
#10286 = ORIENTED_EDGE ( 'NONE', *, *, #29293, .F. ) ;
#10287 = EDGE_CURVE ( 'NONE', #8655, #1157, #4999, .T. ) ;
#10288 = CIRCLE ( 'NONE', #30714, 84.21005050633887379 ) ;
#10289 = DIRECTION ( 'NONE',  ( 0.000000000000000000, 0.000000000000000000, -1.000000000000000000 ) ) ;
#10290 = CARTESIAN_POINT ( 'NONE',  ( 21.09785597605719332, 24.86454579224779948, 21.04930799450051282 ) ) ;
#10291 = ORIENTED_EDGE ( 'NONE', *, *, #22667, .T. ) ;
#10292 = ORIENTED_EDGE ( 'NONE', *, *, #17290, .T. ) ;
#10293 = CARTESIAN_POINT ( 'NONE',  ( 33.71785032049138664, 24.21664230456639899, 47.04930799450051637 ) ) ;
#10294 = DIRECTION ( 'NONE',  ( 1.234978253042719660E-16, -1.000000000000000000, -1.109335647967047851E-31 ) ) ;
#10295 = CARTESIAN_POINT ( 'NONE',  ( -30.86343899296553417, 11.58330661098384695, 70.11433744979635208 ) ) ;
#10296 = DIRECTION ( 'NONE',  ( -1.000000000000000000, 0.000000000000000000, 0.000000000000000000 ) ) ;
#10297 = ORIENTED_EDGE ( 'NONE', *, *, #6214, .T. ) ;
#10298 = FACE_OUTER_BOUND ( 'NONE', #1083, .T. ) ;
#10299 = ORIENTED_EDGE ( 'NONE', *, *, #26494, .T. ) ;
#10300 = CARTESIAN_POINT ( 'NONE',  ( 21.09785597605720042, -14.24176827912842391, 47.04930799450051637 ) ) ;
#10302 = CARTESIAN_POINT ( 'NONE',  ( 21.09785597605720753, 13.80129159329807287, 47.04930799450052348 ) ) ;
#10301 = AXIS2_PLACEMENT_3D ( 'NONE', #25316, #25150, #2668 ) ;
#10303 = ORIENTED_EDGE ( 'NONE', *, *, #4339, .T. ) ;
#10304 = CARTESIAN_POINT ( 'NONE',  ( 48.01680169312756874, 22.93807716476589675, 45.63279442905646022 ) ) ;
#10305 = DIRECTION ( 'NONE',  ( 0.9612616959383207815, 0.2756373558169926685, 8.795445018804289444E-19 ) ) ;
#10306 = DIRECTION ( 'NONE',  ( 0.000000000000000000, -8.673617379884027583E-16, -1.000000000000000000 ) ) ;
#10307 = FACE_OUTER_BOUND ( 'NONE', #18735, .T. ) ;
#10308 = CARTESIAN_POINT ( 'NONE',  ( 49.49063479933183629, 26.61291119454915588, 47.17357720316391578 ) ) ;
#10309 = DIRECTION ( 'NONE',  ( 2.779292025043186357E-18, -1.288349127009862211E-17, 1.000000000000000000 ) ) ;
#10310 = DIRECTION ( 'NONE',  ( -1.000000000000000000, 0.000000000000000000, 0.000000000000000000 ) ) ;
#10311 = VERTEX_POINT ( 'NONE', #9689 ) ;
#10312 = FACE_OUTER_BOUND ( 'NONE', #16966, .T. ) ;
#10313 = VERTEX_POINT ( 'NONE', #2619 ) ;
#10314 = AXIS2_PLACEMENT_3D ( 'NONE', #13871, #16803, #6315 ) ;
#10315 = DIRECTION ( 'NONE',  ( -0.000000000000000000, -1.000000000000000000, 0.000000000000000000 ) ) ;
#10316 = ORIENTED_EDGE ( 'NONE', *, *, #14277, .F. ) ;
#10317 = ORIENTED_EDGE ( 'NONE', *, *, #16585, .T. ) ;
#10318 = DIRECTION ( 'NONE',  ( -0.000000000000000000, -1.000000000000000000, -0.000000000000000000 ) ) ;
#10319 = ADVANCED_FACE ( 'NONE', ( #12649 ), #17572, .T. ) ;
#10320 = EDGE_LOOP ( 'NONE', ( #3960, #12972, #9694, #27169 ) ) ;
#10321 = EDGE_CURVE ( 'NONE', #13009, #20809, #7098, .T. ) ;
#10322 = AXIS2_PLACEMENT_3D ( 'NONE', #18194, #3270, #28066 ) ;
#10323 = ORIENTED_EDGE ( 'NONE', *, *, #20200, .T. ) ;
#10324 = CARTESIAN_POINT ( 'NONE',  ( 45.37383841111020644, 22.88065857334295217, 47.92876263475718446 ) ) ;
#10325 = AXIS2_PLACEMENT_3D ( 'NONE', #7578, #15123, #6921 ) ;
#10326 = ORIENTED_EDGE ( 'NONE', *, *, #16847, .T. ) ;
#10327 =( BOUNDED_CURVE ( )  B_SPLINE_CURVE ( 3, ( #26983, #27141, #21883, #4659 ),
 .UNSPECIFIED., .F., .F. ) 
 B_SPLINE_CURVE_WITH_KNOTS ( ( 4, 4 ),
 ( 3.141592653589793116, 3.657989679900455648 ),
 .UNSPECIFIED. ) 
 CURVE ( )  GEOMETRIC_REPRESENTATION_ITEM ( )  RATIONAL_B_SPLINE_CURVE ( ( 1.000000000000000000, 0.9779010246516581795, 0.9779010246516581795, 1.000000000000000000 ) ) 
 REPRESENTATION_ITEM ( '' )  );
#10328 = DIRECTION ( 'NONE',  ( -0.2756373558169932236, 0.9612616959383205595, 2.536267806945839542E-31 ) ) ;
#10329 = DIRECTION ( 'NONE',  ( -1.101824276508909887E-16, 1.000000000000000000, -0.000000000000000000 ) ) ;
#10330 = CARTESIAN_POINT ( 'NONE',  ( 45.35708200440645044, 26.20457786121582444, 45.92000246470679770 ) ) ;
#10331 = ORIENTED_EDGE ( 'NONE', *, *, #9667, .F. ) ;
#10332 = ORIENTED_EDGE ( 'NONE', *, *, #28084, .F. ) ;
#10333 = CARTESIAN_POINT ( 'NONE',  ( 47.09785597605719687, 25.56454579224779877, 47.04930799450042400 ) ) ;
#10334 = ORIENTED_EDGE ( 'NONE', *, *, #16842, .T. ) ;
#10335 = LINE ( 'NONE', #8517, #12084 ) ;
#10336 = CARTESIAN_POINT ( 'NONE',  ( 48.12516263684333495, 9.438446991585321300, 98.40972204454067196 ) ) ;
#10337 = PLANE ( 'NONE',  #28447 ) ;
#10338 = CARTESIAN_POINT ( 'NONE',  ( 21.09785597605719332, 44.06454579224779877, 48.04930799450048795 ) ) ;
#10339 = CARTESIAN_POINT ( 'NONE',  ( 46.17891025898683921, 22.93807716476589675, 48.46582155994513386 ) ) ;
#10340 = APPLICATION_PROTOCOL_DEFINITION ( 'draft international standard', 'automotive_design', 1998, #30906 ) ;
#10341 = ORIENTED_EDGE ( 'NONE', *, *, #10654, .T. ) ;
#10342 = CARTESIAN_POINT ( 'NONE',  ( -41.88090303775678080, 13.82677487427665675, 54.54930799450051637 ) ) ;
#10343 = CIRCLE ( 'NONE', #27100, 2.500000000000002220 ) ;
#10344 = DIRECTION ( 'NONE',  ( -1.000000000000000000, 0.000000000000000000, 0.000000000000000000 ) ) ;
#10345 = CARTESIAN_POINT ( 'NONE',  ( -9.880269301913145341, -5.935454207809699234, 107.5832060159989965 ) ) ;
#10346 = CARTESIAN_POINT ( 'NONE',  ( 48.18662509608405031, 28.68284706826093000, 49.18364984542562013 ) ) ;
#10347 = ORIENTED_EDGE ( 'NONE', *, *, #20239, .F. ) ;
#10348 = CARTESIAN_POINT ( 'NONE',  ( 8.698509210239569356, 30.09164230456639544, 47.04930799450051637 ) ) ;
#10349 = CARTESIAN_POINT ( 'NONE',  ( -40.60330327974818942, 7.565477138576675920, 53.88146687024393344 ) ) ;
#10350 = CARTESIAN_POINT ( 'NONE',  ( 8.474859994195281132, 31.59143805560860585, 47.04930799450051637 ) ) ;
#10351 = EDGE_CURVE ( 'NONE', #9452, #12894, #7394, .T. ) ;
#10352 = ADVANCED_FACE ( 'NONE', ( #15259 ), #7220, .F. ) ;
#10353 = ADVANCED_FACE ( 'NONE', ( #17221 ), #13394, .T. ) ;
#10354 = ADVANCED_FACE ( 'NONE', ( #10179 ), #30200, .F. ) ;
#10355 = EDGE_LOOP ( 'NONE', ( #10732, #12402, #16198, #8575 ) ) ;
#10356 = VECTOR ( 'NONE', #16087, 1000.000000000000000 ) ;
#10357 = VERTEX_POINT ( 'NONE', #7710 ) ;
#10358 = FACE_OUTER_BOUND ( 'NONE', #11483, .T. ) ;
#10359 = AXIS2_PLACEMENT_3D ( 'NONE', #28741, #693, #23178 ) ;
#10360 = CARTESIAN_POINT ( 'NONE',  ( -44.16105795751995799, -3.935454207752183020, 52.04930799450050927 ) ) ;
#10361 = DIRECTION ( 'NONE',  ( -1.101824276508909887E-16, 1.000000000000000000, -0.000000000000000000 ) ) ;
#10362 = TOROIDAL_SURFACE ( 'NONE', #18718, 1.899999999999999467, 0.1000000000000000056 ) ;
#10363 = EDGE_LOOP ( 'NONE', ( #27836, #12744 ) ) ;
#10364 = CARTESIAN_POINT ( 'NONE',  ( -42.37913764077812573, 15.23192269303852875, 35.64930799450052490 ) ) ;
#10365 = VECTOR ( 'NONE', #18591, 1000.000000000000000 ) ;
#10366 = CARTESIAN_POINT ( 'NONE',  ( 7.896071960694297509, 17.16467605102632632, 47.04930799450052348 ) ) ;
#10367 = LINE ( 'NONE', #27926, #6190 ) ;
#10368 = DIRECTION ( 'NONE',  ( -1.000000000000000000, 0.000000000000000000, 0.000000000000000000 ) ) ;
#10369 = CARTESIAN_POINT ( 'NONE',  ( 21.09785597605720042, -16.73545420775220194, 47.04930799450051637 ) ) ;
#10370 = CIRCLE ( 'NONE', #409, 12.62506659569710266 ) ;
#10371 = FACE_BOUND ( 'NONE', #11053, .T. ) ;
#10372 = CARTESIAN_POINT ( 'NONE',  ( -40.58856461370174173, 7.499380836222957925, 60.14930799450051069 ) ) ;
#10373 = CARTESIAN_POINT ( 'NONE',  ( 45.29931651390019454, 22.86454579224779948, 47.92489232862990889 ) ) ;
#10374 = DIRECTION ( 'NONE',  ( 0.000000000000000000, 0.000000000000000000, -1.000000000000000000 ) ) ;
#10375 = FACE_OUTER_BOUND ( 'NONE', #13611, .T. ) ;
#10376 =( NAMED_UNIT ( * ) PLANE_ANGLE_UNIT ( ) SI_UNIT ( $, .RADIAN. ) );
#10377 = EDGE_LOOP ( 'NONE', ( #4757, #20206, #15068, #22264 ) ) ;
#10378 = ORIENTED_EDGE ( 'NONE', *, *, #10404, .T. ) ;
#10379 = ADVANCED_FACE ( 'NONE', ( #7554 ), #15998, .T. ) ;
#10380 = DIRECTION ( 'NONE',  ( 0.8746197071393926326, -0.4848096202463430537, -8.676864087101709653E-18 ) ) ;
#10381 = CARTESIAN_POINT ( 'NONE',  ( 49.65101332465108186, 24.93501648625822398, 46.52608845888364186 ) ) ;
#10382 = CARTESIAN_POINT ( 'NONE',  ( -36.59584142669144313, -5.867400066089301980, 15.57347139224829213 ) ) ;
#10383 = CARTESIAN_POINT ( 'NONE',  ( 21.09992658989239089, 28.21664230456639899, 47.04930799450051637 ) ) ;
#10384 = ORIENTED_EDGE ( 'NONE', *, *, #12418, .T. ) ;
#10385 = CARTESIAN_POINT ( 'NONE',  ( 8.698509210239542710, 27.59164230456639544, 47.04930799450051637 ) ) ;
#10386 = CARTESIAN_POINT ( 'NONE',  ( 48.22193606911519481, 23.04411619146717882, 47.10768726602483980 ) ) ;
#10387 = CARTESIAN_POINT ( 'NONE',  ( -40.12099660621118602, 7.356848571226523248, 38.85576968460465963 ) ) ;
#10388 = ORIENTED_EDGE ( 'NONE', *, *, #22025, .T. ) ;
#10389 = ORIENTED_EDGE ( 'NONE', *, *, #13581, .F. ) ;
#10390 = DIRECTION ( 'NONE',  ( 0.000000000000000000, 0.000000000000000000, -1.000000000000000000 ) ) ;
#10391 = CARTESIAN_POINT ( 'NONE',  ( 46.99023568444673060, 28.62451373492759643, 49.12151524109405898 ) ) ;
#10392 = CIRCLE ( 'NONE', #17701, 0.6999999999999992895 ) ;
#10393 = CARTESIAN_POINT ( 'NONE',  ( 48.83862994770794330, 28.65457786121581663, 48.17861352429476796 ) ) ;
#10394 = CIRCLE ( 'NONE', #28720, 12.62506659569710266 ) ;
#10395 = DIRECTION ( 'NONE',  ( 0.000000000000000000, -1.000000000000000000, 0.000000000000000000 ) ) ;
#10396 = TOROIDAL_SURFACE ( 'NONE', #28722, 12.61792373059858541, 0.1250000000000004996 ) ;
#10397 = DIRECTION ( 'NONE',  ( -1.101824276508909887E-16, 1.000000000000000000, -0.000000000000000000 ) ) ;
#10398 = AXIS2_PLACEMENT_3D ( 'NONE', #26560, #14261, #9002 ) ;
#10399 = ADVANCED_FACE ( 'NONE', ( #27732 ), #1330, .T. ) ;
#10400 = VECTOR ( 'NONE', #23991, 1000.000000000000114 ) ;
#10401 = ORIENTED_EDGE ( 'NONE', *, *, #2228, .T. ) ;
#10402 = CARTESIAN_POINT ( 'NONE',  ( 21.09992658989239089, 24.59164230456639544, 47.04930799450051637 ) ) ;
#10403 = VERTEX_POINT ( 'NONE', #32338 ) ;
#10404 = EDGE_CURVE ( 'NONE', #16051, #10149, #27340, .T. ) ;
#10405 = CARTESIAN_POINT ( 'NONE',  ( 21.09785597605720397, -19.93545420775220123, -37.25069200549950210 ) ) ;
#10406 = FACE_OUTER_BOUND ( 'NONE', #29476, .T. ) ;
#10407 = AXIS2_PLACEMENT_3D ( 'NONE', #25651, #20396, #7777 ) ;
#10408 = CIRCLE ( 'NONE', #3063, 31.00000000000000000 ) ;
#10409 = EDGE_CURVE ( 'NONE', #31613, #29876, #3414, .T. ) ;
#10410 = AXIS2_PLACEMENT_3D ( 'NONE', #30058, #25123, #5265 ) ;
#10411 = EDGE_LOOP ( 'NONE', ( #14693, #29571 ) ) ;
#10412 = DIRECTION ( 'NONE',  ( -1.101824276508909887E-16, 1.000000000000000000, -0.000000000000000000 ) ) ;
#10413 = AXIS2_PLACEMENT_3D ( 'NONE', #24787, #11835, #4441 ) ;
#10414 = CARTESIAN_POINT ( 'NONE',  ( 21.09785597605720753, 15.23835801850285776, 47.04930799450052348 ) ) ;
#10415 = CARTESIAN_POINT ( 'NONE',  ( 8.698509210239501854, 23.59164230456639544, 47.04930799450051637 ) ) ;
#10416 = CIRCLE ( 'NONE', #21391, 19.00000000000000000 ) ;
#10417 = CARTESIAN_POINT ( 'NONE',  ( -4.667471018111241321, 10.39302479005550239, -3.469166095471690969 ) ) ;
#10418 = LINE ( 'NONE', #30605, #7079 ) ;
#10419 = ORIENTED_EDGE ( 'NONE', *, *, #32056, .F. ) ;
#10420 = EDGE_CURVE ( 'NONE', #414, #17658, #22743, .T. ) ;
#10421 = CARTESIAN_POINT ( 'NONE',  ( 72.06126861588310817, 6.094407115496644600, 76.95590581573344480 ) ) ;
#10422 = DIRECTION ( 'NONE',  ( -1.000000000000000000, 0.000000000000000000, 0.000000000000000000 ) ) ;
#10423 = EDGE_CURVE ( 'NONE', #32103, #1121, #11225, .T. ) ;
#10424 = DIRECTION ( 'NONE',  ( -0.000000000000000000, -1.000000000000000000, 0.000000000000000000 ) ) ;
#10425 = CARTESIAN_POINT ( 'NONE',  ( -40.47970302497625994, 7.463434137431151250, 60.54930799450051637 ) ) ;
#10426 = AXIS2_PLACEMENT_3D ( 'NONE', #25321, #5616, #23336 ) ;
#10427 = CARTESIAN_POINT ( 'NONE',  ( 48.66895200406656841, 26.36155426599985674, 44.62753372671560470 ) ) ;
#10428 = ORIENTED_EDGE ( 'NONE', *, *, #20755, .T. ) ;
#10429 = DIRECTION ( 'NONE',  ( 0.000000000000000000, 0.000000000000000000, -1.000000000000000000 ) ) ;
#10430 = CARTESIAN_POINT ( 'NONE',  ( 21.09785597605719332, 13.74476430820393347, 101.3493079945005064 ) ) ;
#10431 = ORIENTED_EDGE ( 'NONE', *, *, #10542, .F. ) ;
#10432 = CARTESIAN_POINT ( 'NONE',  ( 21.09785597605720042, -13.87844638871996850, -12.39237876099712210 ) ) ;
#10433 = DIRECTION ( 'NONE',  ( 1.234978253042719660E-16, -1.000000000000000000, -1.109335647967047851E-31 ) ) ;
#10434 = CARTESIAN_POINT ( 'NONE',  ( 21.09785597605720753, 13.86454579224779948, 47.04930799450052348 ) ) ;
#10435 = FACE_OUTER_BOUND ( 'NONE', #8198, .T. ) ;
#10436 = ORIENTED_EDGE ( 'NONE', *, *, #19337, .F. ) ;
#10437 = DIRECTION ( 'NONE',  ( -1.000000000000000000, -1.101824276508909887E-16, 0.000000000000000000 ) ) ;
#10438 = VERTEX_POINT ( 'NONE', #25431 ) ;
#10439 = EDGE_CURVE ( 'NONE', #21770, #13402, #31151, .T. ) ;
#10440 = TOROIDAL_SURFACE ( 'NONE', #4135, 58.86319174311611846, 0.1999999999999984290 ) ;
#10441 = CIRCLE ( 'NONE', #4661, 11.79999999999997762 ) ;
#10442 = ORIENTED_EDGE ( 'NONE', *, *, #15354, .T. ) ;
#10443 = AXIS2_PLACEMENT_3D ( 'NONE', #16063, #13137, #652 ) ;
#10444 = CIRCLE ( 'NONE', #10980, 2.000000000000001776 ) ;
#10445 = EDGE_CURVE ( 'NONE', #11324, #23543, #19125, .T. ) ;
#10446 = CARTESIAN_POINT ( 'NONE',  ( 21.09785597605719687, 25.56454579224779877, 7.349896848133565364 ) ) ;
#10447 = CARTESIAN_POINT ( 'NONE',  ( -37.42114908093812176, 11.86897798031838391, 60.44930799450051495 ) ) ;
#10448 = CARTESIAN_POINT ( 'NONE',  ( 21.09785597605720753, -13.98292989133646103, -11.62287111200335055 ) ) ;
#10449 = ADVANCED_FACE ( 'NONE', ( #28061 ), #24918, .T. ) ;
#10450 = ORIENTED_EDGE ( 'NONE', *, *, #32430, .F. ) ;
#10451 = VERTEX_POINT ( 'NONE', #25586 ) ;
#10452 = CYLINDRICAL_SURFACE ( 'NONE', #8874, 12.36707279061065101 ) ;
#10453 = FACE_OUTER_BOUND ( 'NONE', #18636, .T. ) ;
#10454 = DIRECTION ( 'NONE',  ( -1.101824276508909887E-16, 1.000000000000000000, -0.000000000000000000 ) ) ;
#10455 = DIRECTION ( 'NONE',  ( -1.224646799147353207E-16, -1.349345573449484691E-32, 1.000000000000000000 ) ) ;
#10456 = ORIENTED_EDGE ( 'NONE', *, *, #15069, .F. ) ;
#10457 = CARTESIAN_POINT ( 'NONE',  ( -12.51953758373980463, -1.428409478025985280, 100.6377223385756565 ) ) ;
#10458 = DIRECTION ( 'NONE',  ( -1.101824276508909887E-16, 1.000000000000000000, -0.000000000000000000 ) ) ;
#10459 = CARTESIAN_POINT ( 'NONE',  ( -42.38687957179149635, 4.148162238787999279, 37.04930799450052348 ) ) ;
#10460 = CARTESIAN_POINT ( 'NONE',  ( -6.912293520256177715, 8.510833471476315637, -3.454653683043350743 ) ) ;
#10461 = AXIS2_PLACEMENT_3D ( 'NONE', #19301, #1754, #18811 ) ;
#10462 = ADVANCED_FACE ( 'NONE', ( #13298 ), #795, .F. ) ;
#10463 = ORIENTED_EDGE ( 'NONE', *, *, #10010, .F. ) ;
#10464 = CARTESIAN_POINT ( 'NONE',  ( 46.58637386172244277, 23.04411619146718238, 46.04663644226216945 ) ) ;
#10465 = AXIS2_PLACEMENT_3D ( 'NONE', #28785, #16467, #8921 ) ;
#10466 = CARTESIAN_POINT ( 'NONE',  ( 81.63177831856063449, -5.935454207752202116, 16.07118271501079576 ) ) ;
#10467 = DIRECTION ( 'NONE',  ( 0.000000000000000000, 0.000000000000000000, -1.000000000000000000 ) ) ;
#10468 = CARTESIAN_POINT ( 'NONE',  ( 21.09785597605719332, -15.93545420775219945, 47.04930799450051637 ) ) ;
#10469 = EDGE_CURVE ( 'NONE', #5512, #1774, #18352, .T. ) ;
#10470 = CARTESIAN_POINT ( 'NONE',  ( 45.79384627280941089, 24.97957786121582302, 49.05938063676249072 ) ) ;
#10471 = LINE ( 'NONE', #17521, #5321 ) ;
#10472 = CARTESIAN_POINT ( 'NONE',  ( 47.09785597605719687, 20.36454579224780304, 47.04930799450078638 ) ) ;
#10473 = VERTEX_POINT ( 'NONE', #16689 ) ;
#10474 = DIRECTION ( 'NONE',  ( -1.101824276508909887E-16, 1.000000000000000000, -0.000000000000000000 ) ) ;
#10475 = EDGE_LOOP ( 'NONE', ( #10943, #7638, #20279, #11380 ) ) ;
#10476 = AXIS2_PLACEMENT_3D ( 'NONE', #25799, #8093, #26115 ) ;
#10477 = AXIS2_PLACEMENT_3D ( 'NONE', #5835, #13064, #30940 ) ;
#10478 = LINE ( 'NONE', #22929, #13772 ) ;
#10479 = ORIENTED_EDGE ( 'NONE', *, *, #13638, .T. ) ;
#10480 = TOROIDAL_SURFACE ( 'NONE', #7326, 12.40141737965281266, 0.1249999999999994865 ) ;
#10481 = ORIENTED_EDGE ( 'NONE', *, *, #18, .T. ) ;
#10482 = DIRECTION ( 'NONE',  ( -1.101824276508909887E-16, 1.000000000000000000, -0.000000000000000000 ) ) ;
#10483 = CIRCLE ( 'NONE', #19379, 0.1250000000000001110 ) ;
#10484 = EDGE_LOOP ( 'NONE', ( #17343, #10045, #13259, #26021 ) ) ;
#10485 = AXIS2_PLACEMENT_3D ( 'NONE', #28139, #15335, #3006 ) ;
#10486 = ORIENTED_EDGE ( 'NONE', *, *, #26716, .F. ) ;
#10487 = EDGE_CURVE ( 'NONE', #9009, #13651, #7626, .T. ) ;
#10488 = CARTESIAN_POINT ( 'NONE',  ( 71.49893360114316465, -5.935454207752202116, 16.07118271501076734 ) ) ;
#10489 = CIRCLE ( 'NONE', #9973, 12.36707279061065101 ) ;
#10490 = TOROIDAL_SURFACE ( 'NONE', #13116, 56.00000000000000000, 1.000000000000000000 ) ;
#10491 = ORIENTED_EDGE ( 'NONE', *, *, #15523, .F. ) ;
#10492 = FACE_OUTER_BOUND ( 'NONE', #23481, .T. ) ;
#10493 = VECTOR ( 'NONE', #20408, 1000.000000000000114 ) ;
#10494 = DIRECTION ( 'NONE',  ( -1.000000000000000000, 0.000000000000000000, 0.000000000000000000 ) ) ;
#10495 = DIRECTION ( 'NONE',  ( -1.000000000000000000, 0.000000000000000000, 0.000000000000000000 ) ) ;
#10496 = CARTESIAN_POINT ( 'NONE',  ( 48.37829923888483563, 28.15122849631042712, 45.07556196625585443 ) ) ;
#10497 = TOROIDAL_SURFACE ( 'NONE', #14690, 12.61792373059893713, 0.1249999999999992506 ) ;
#10498 = TOROIDAL_SURFACE ( 'NONE', #31993, 12.40141737965287305, 0.1250000000000000833 ) ;
#10499 = ORIENTED_EDGE ( 'NONE', *, *, #13989, .T. ) ;
#10500 = EDGE_LOOP ( 'NONE', ( #27325, #27178, #945 ) ) ;
#10501 = CARTESIAN_POINT ( 'NONE',  ( 21.09992658989239089, 25.34164230456639899, 47.04930799450051637 ) ) ;
#10502 = EDGE_CURVE ( 'NONE', #27701, #30925, #26232, .T. ) ;
#10503 = ORIENTED_EDGE ( 'NONE', *, *, #9375, .T. ) ;
#10504 = CARTESIAN_POINT ( 'NONE',  ( 49.84415473660248352, 24.82319976284615137, 47.19193729663540893 ) ) ;
#10505 = CARTESIAN_POINT ( 'NONE',  ( 50.12193823907599466, 7.326690775934355138, 98.65510655449794797 ) ) ;
#10506 = CARTESIAN_POINT ( 'NONE',  ( -39.58809650894544774, 2.596771453999702661, 49.04930799450051637 ) ) ;
#10507 = CARTESIAN_POINT ( 'NONE',  ( 47.47194490827082092, 22.91413368675619111, 45.28548791484912783 ) ) ;
#10508 = DIRECTION ( 'NONE',  ( 0.000000000000000000, 0.000000000000000000, 1.000000000000000000 ) ) ;
#10509 = APPLICATION_PROTOCOL_DEFINITION ( 'draft international standard', 'automotive_design', 1998, #27107 ) ;
#10510 = ORIENTED_EDGE ( 'NONE', *, *, #3887, .T. ) ;
#10511 = FACE_OUTER_BOUND ( 'NONE', #8066, .T. ) ;
#10512 = VECTOR ( 'NONE', #19396, 999.9999999999998863 ) ;
#10513 = DIRECTION ( 'NONE',  ( -1.000000000000000000, 0.000000000000000000, 0.000000000000000000 ) ) ;
#10514 = CARTESIAN_POINT ( 'NONE',  ( 58.09785597605721108, 14.86454579224779948, 47.04930799450051637 ) ) ;
#10515 = DIRECTION ( 'NONE',  ( -1.000000000000000000, 0.000000000000000000, 0.000000000000000000 ) ) ;
#10516 = ORIENTED_EDGE ( 'NONE', *, *, #27802, .F. ) ;
#10517 = DIRECTION ( 'NONE',  ( 1.234978253042719660E-16, -1.000000000000000000, -1.109335647967047851E-31 ) ) ;
#10518 = CYLINDRICAL_SURFACE ( 'NONE', #13039, 12.62506659569710266 ) ;
#10519 = CIRCLE ( 'NONE', #24106, 22.64135752993680484 ) ;
#10520 = AXIS2_PLACEMENT_3D ( 'NONE', #10447, #3039, #1950 ) ;
#10521 = CARTESIAN_POINT ( 'NONE',  ( 46.09785597605720397, -5.098646251524523443, 47.04930799450052348 ) ) ;
#10522 = ORIENTED_EDGE ( 'NONE', *, *, #10195, .F. ) ;
#10523 = AXIS2_PLACEMENT_3D ( 'NONE', #23801, #15780, #13648 ) ;
#10524 = AXIS2_PLACEMENT_3D ( 'NONE', #8790, #23731, #6021 ) ;
#10525 = AXIS2_PLACEMENT_3D ( 'NONE', #14306, #24139, #11841 ) ;
#10526 = VECTOR ( 'NONE', #14054, 1000.000000000000000 ) ;
#10527 = ORIENTED_EDGE ( 'NONE', *, *, #15821, .F. ) ;
#10528 = ORIENTED_EDGE ( 'NONE', *, *, #12619, .T. ) ;
#10529 = DIRECTION ( 'NONE',  ( 0.000000000000000000, 0.000000000000000000, 1.000000000000000000 ) ) ;
#10530 = DIRECTION ( 'NONE',  ( -1.101824276508909887E-16, 1.000000000000000000, -0.000000000000000000 ) ) ;
#10531 = AXIS2_PLACEMENT_3D ( 'NONE', #17916, #20698, #25784 ) ;
#10532 = EDGE_LOOP ( 'NONE', ( #4376, #11335, #24039, #6846, #18337 ) ) ;
#10533 = DIRECTION ( 'NONE',  ( 0.000000000000000000, 0.000000000000000000, -1.000000000000000000 ) ) ;
#10534 = LINE ( 'NONE', #30558, #1825 ) ;
#10535 = LINE ( 'NONE', #13480, #31075 ) ;
#10536 = DIRECTION ( 'NONE',  ( -1.000000000000000000, 0.000000000000000000, 0.000000000000000000 ) ) ;
#10537 = ADVANCED_FACE ( 'NONE', ( #6208 ), #31653, .F. ) ;
#10538 = CIRCLE ( 'NONE', #14708, 12.36707279061065279 ) ;
#10539 = DIRECTION ( 'NONE',  ( 0.000000000000000000, -1.000000000000000000, 0.000000000000000000 ) ) ;
#10540 = DIRECTION ( 'NONE',  ( 0.000000000000000000, 0.000000000000000000, -1.000000000000000000 ) ) ;
#10541 = CARTESIAN_POINT ( 'NONE',  ( -40.58117736050017754, 7.466252321088952648, 60.18657739374794602 ) ) ;
#10542 = EDGE_CURVE ( 'NONE', #27140, #28668, #3744, .T. ) ;
#10543 = DIRECTION ( 'NONE',  ( 0.000000000000000000, 0.000000000000000000, -1.000000000000000000 ) ) ;
#10545 = EDGE_CURVE ( 'NONE', #27609, #9365, #4189, .T. ) ;
#10544 = DIRECTION ( 'NONE',  ( -1.000000000000000000, 0.000000000000000000, 0.000000000000000000 ) ) ;
#10546 = EDGE_CURVE ( 'NONE', #18781, #1013, #12883, .T. ) ;
#10547 = AXIS2_PLACEMENT_3D ( 'NONE', #19320, #11790, #2095 ) ;
#10548 = AXIS2_PLACEMENT_3D ( 'NONE', #23158, #25464, #15602 ) ;
#10549 = DIRECTION ( 'NONE',  ( -1.000000000000000000, -1.101824276508910010E-16, 0.000000000000000000 ) ) ;
#10550 = CARTESIAN_POINT ( 'NONE',  ( 50.10320668408830613, 28.40621246473837402, 47.20539118556276037 ) ) ;
#10551 = AXIS2_PLACEMENT_3D ( 'NONE', #31602, #6324, #28973 ) ;
#10552 = ORIENTED_EDGE ( 'NONE', *, *, #18773, .T. ) ;
#10553 = EDGE_LOOP ( 'NONE', ( #10094, #6881, #20984, #3043 ) ) ;
#10554 = DIRECTION ( 'NONE',  ( 0.8746197071393925215, -0.4848096202463429982, -8.676864087101708112E-18 ) ) ;
#10555 = EDGE_CURVE ( 'NONE', #18375, #28679, #2909, .T. ) ;
#10556 = AXIS2_PLACEMENT_3D ( 'NONE', #30930, #27982, #3500 ) ;
#10557 = FACE_OUTER_BOUND ( 'NONE', #16144, .T. ) ;
#10558 = ORIENTED_EDGE ( 'NONE', *, *, #25932, .F. ) ;
#10559 = CARTESIAN_POINT ( 'NONE',  ( -39.46038060626020894, -5.935454093830753841, 77.98462090466851748 ) ) ;
#10560 = CARTESIAN_POINT ( 'NONE',  ( 48.79245099466763946, 22.93807716476589675, 46.97542197481624271 ) ) ;
#10561 = ORIENTED_EDGE ( 'NONE', *, *, #8853, .T. ) ;
#10562 = VERTEX_POINT ( 'NONE', #11303 ) ;
#10563 = DIRECTION ( 'NONE',  ( 0.000000000000000000, -1.000000000000000000, 0.000000000000000000 ) ) ;
#10564 = CARTESIAN_POINT ( 'NONE',  ( 45.24946171279598417, 27.10784706826093071, 47.99220971130007030 ) ) ;
#10565 = TOROIDAL_SURFACE ( 'NONE', #19988, 12.40141737965285706, 0.1250000000000007494 ) ;
#10566 = CARTESIAN_POINT ( 'NONE',  ( 48.18662509608405031, 27.89624452788248377, 49.18364984542562013 ) ) ;
#10567 = CARTESIAN_POINT ( 'NONE',  ( -39.40755539011571784, -5.935795008504334724, 77.96850645159442195 ) ) ;
#10568 = VERTEX_POINT ( 'NONE', #29180 ) ;
#10569 = CIRCLE ( 'NONE', #14236, 12.36707279061065101 ) ;
#10570 = AXIS2_PLACEMENT_3D ( 'NONE', #10263, #20411, #20250 ) ;
#10571 = FACE_OUTER_BOUND ( 'NONE', #568, .T. ) ;
#10572 = EDGE_CURVE ( 'NONE', #23334, #19780, #11293, .T. ) ;
#10573 = DIRECTION ( 'NONE',  ( -1.224646799147353207E-16, 0.000000000000000000, -1.000000000000000000 ) ) ;
#10574 = VECTOR ( 'NONE', #2092, 1000.000000000000114 ) ;
#10575 = ORIENTED_EDGE ( 'NONE', *, *, #8258, .F. ) ;
#10576 = DIRECTION ( 'NONE',  ( 1.000000000000000000, 0.000000000000000000, 0.000000000000000000 ) ) ;
#10577 = CARTESIAN_POINT ( 'NONE',  ( 33.46699938050304013, 23.72145308207319658, 47.04930799450050927 ) ) ;
#10578 = CIRCLE ( 'NONE', #7982, 12.62506659569710266 ) ;
#10579 = VERTEX_POINT ( 'NONE', #26060 ) ;
#10580 = CARTESIAN_POINT ( 'NONE',  ( -40.34207605779958072, 7.502898035225042506, 60.44930799450051495 ) ) ;
#10581 = EDGE_CURVE ( 'NONE', #26808, #16322, #16970, .T. ) ;
#10582 = CARTESIAN_POINT ( 'NONE',  ( -42.73182147790732444, -0.8057266458565844891, 61.94930799450052206 ) ) ;
#10584 = EDGE_CURVE ( 'NONE', #32232, #1639, #20515, .T. ) ;
#10583 = CYLINDRICAL_SURFACE ( 'NONE', #18844, 2.000000000000001776 ) ;
#10585 = ADVANCED_FACE ( 'NONE', ( #8828 ), #31163, .F. ) ;
#10586 = FACE_OUTER_BOUND ( 'NONE', #10823, .T. ) ;
#10587 = EDGE_CURVE ( 'NONE', #22169, #154, #26395, .T. ) ;
#10588 = FACE_OUTER_BOUND ( 'NONE', #26435, .T. ) ;
#10589 = EDGE_LOOP ( 'NONE', ( #4231, #32243, #8476, #15110 ) ) ;
#10590 = CARTESIAN_POINT ( 'NONE',  ( 8.732853799281729223, 26.47145308207318593, 47.04930799450051637 ) ) ;
#10592 = ADVANCED_FACE ( 'NONE', ( #21451 ), #31487, .F. ) ;
#10591 = LINE ( 'NONE', #30928, #2707 ) ;
#10593 = PLANE ( 'NONE',  #29261 ) ;
#10594 = DIRECTION ( 'NONE',  ( -0.8746197071393926326, 0.4848096202463430537, 8.676864087101709653E-18 ) ) ;
#10595 = AXIS2_PLACEMENT_3D ( 'NONE', #28503, #8160, #6017 ) ;
#10596 = CARTESIAN_POINT ( 'NONE',  ( 48.23388202445966044, 26.12822092656774586, 49.27628909396054979 ) ) ;
#10597 = ORIENTED_EDGE ( 'NONE', *, *, #11602, .T. ) ;
#10598 = CIRCLE ( 'NONE', #26833, 0.1250000000000001110 ) ;
#10599 = DIRECTION ( 'NONE',  ( -1.000000000000000000, 0.000000000000000000, 0.000000000000000000 ) ) ;
#10600 = CARTESIAN_POINT ( 'NONE',  ( -40.61197514715824752, 6.966360136513626955, 39.01065621547813578 ) ) ;
#10601 = CARTESIAN_POINT ( 'NONE',  ( 21.09785597605719332, 15.06454579224778456, 47.04930799450051637 ) ) ;
#10602 = VERTEX_POINT ( 'NONE', #26553 ) ;
#10603 = CARTESIAN_POINT ( 'NONE',  ( 80.79555976727768041, -5.935454207752198563, 77.87546120947919803 ) ) ;
#10604 = DIRECTION ( 'NONE',  ( -1.000000000000000000, -1.101824276508909887E-16, 0.000000000000000000 ) ) ;
#10605 = FACE_OUTER_BOUND ( 'NONE', #26138, .T. ) ;
#10606 = CARTESIAN_POINT ( 'NONE',  ( 21.09785597605719332, 30.56554579224779644, 23.54930799450051282 ) ) ;
#10607 = ORIENTED_EDGE ( 'NONE', *, *, #22624, .F. ) ;
#10608 = LINE ( 'NONE', #7809, #18288 ) ;
#10609 = VERTEX_POINT ( 'NONE', #14089 ) ;
#10610 = VECTOR ( 'NONE', #19933, 1000.000000000000000 ) ;
#10611 = ORIENTED_EDGE ( 'NONE', *, *, #18447, .T. ) ;
#10612 = AXIS2_PLACEMENT_3D ( 'NONE', #9395, #32210, #14324 ) ;
#10613 = ADVANCED_FACE ( 'NONE', ( #1603 ), #11624, .F. ) ;
#10614 = EDGE_CURVE ( 'NONE', #17055, #31760, #13123, .T. ) ;
#10615 =( GEOMETRIC_REPRESENTATION_CONTEXT ( 3 ) GLOBAL_UNCERTAINTY_ASSIGNED_CONTEXT ( ( #3883 ) ) GLOBAL_UNIT_ASSIGNED_CONTEXT ( ( #21486, #31840, #24445 ) ) REPRESENTATION_CONTEXT ( 'NONE', 'WORKASPACE' ) );
#10616 = TOROIDAL_SURFACE ( 'NONE', #23713, 12.40141737965282154, 0.1250000000000006939 ) ;
#10617 = CARTESIAN_POINT ( 'NONE',  ( 48.66895200406656841, 27.76155426599985176, 44.62753372671560470 ) ) ;
#10618 = CARTESIAN_POINT ( 'NONE',  ( 21.09992658989238734, 31.09164230456639544, 47.04930799450051637 ) ) ;
#10619 = CYLINDRICAL_SURFACE ( 'NONE', #418, 2.500000000000002220 ) ;
#10620 = VERTEX_POINT ( 'NONE', #10141 ) ;
#10621 = CARTESIAN_POINT ( 'NONE',  ( 33.72499318558949000, 38.56284415653841791, 47.04930799450051637 ) ) ;
#10622 = ORIENTED_EDGE ( 'NONE', *, *, #2214, .T. ) ;
#10623 = CARTESIAN_POINT ( 'NONE',  ( -10.97410526921440521, -5.983766253076979069, 106.8025418868326284 ) ) ;
#10624 = CARTESIAN_POINT ( 'NONE',  ( 21.09785597605719332, 25.56454579224780232, 128.7593585008393973 ) ) ;
#10625 = CARTESIAN_POINT ( 'NONE',  ( -30.29077459323982424, 10.19186367684678984, 73.11371490948231155 ) ) ;
#10626 = DIRECTION ( 'NONE',  ( -1.000000000000000000, 0.000000000000000000, 0.000000000000000000 ) ) ;
#10627 = EDGE_CURVE ( 'NONE', #23399, #7831, #19457, .T. ) ;
#10628 = EDGE_LOOP ( 'NONE', ( #22164, #8448, #12909, #15941, #32487 ) ) ;
#10629 = CARTESIAN_POINT ( 'NONE',  ( 21.09992658989239089, 29.21664230456640254, 47.04930799450051637 ) ) ;
#10630 = DIRECTION ( 'NONE',  ( -0.000000000000000000, -1.000000000000000000, -0.000000000000000000 ) ) ;
#10631 = DIRECTION ( 'NONE',  ( -1.234978253042719660E-16, 1.000000000000000000, 1.170965406187439618E-31 ) ) ;
#10632 = CARTESIAN_POINT ( 'NONE',  ( 45.64214785356322324, 22.86454579224779593, 45.61839217665156809 ) ) ;
#10633 = ORIENTED_EDGE ( 'NONE', *, *, #27914, .T. ) ;
#10634 = CARTESIAN_POINT ( 'NONE',  ( 47.09785597605719687, 23.12036939723557083, 47.04930799450080059 ) ) ;
#10635 = CARTESIAN_POINT ( 'NONE',  ( 81.61462554241957434, -5.935651417315360057, 15.94210079323268836 ) ) ;
#10636 = DIRECTION ( 'NONE',  ( -0.000000000000000000, -1.000000000000000000, -0.000000000000000000 ) ) ;
#10637 = DIRECTION ( 'NONE',  ( -1.431146867680865853E-17, -2.558717127065790464E-17, -1.000000000000000000 ) ) ;
#10638 = AXIS2_PLACEMENT_3D ( 'NONE', #5606, #20537, #28733 ) ;
#10639 = LINE ( 'NONE', #18317, #27288 ) ;
#10640 = DIRECTION ( 'NONE',  ( -1.000000000000000000, 0.000000000000000000, 0.000000000000000000 ) ) ;
#10641 = CARTESIAN_POINT ( 'NONE',  ( -40.64522151305507691, 6.818818762547660839, 34.57215670535448027 ) ) ;
#10642 = AXIS2_PLACEMENT_3D ( 'NONE', #14771, #12472, #29869 ) ;
#10643 = EDGE_LOOP ( 'NONE', ( #9914, #24050, #1133, #6024 ) ) ;
#10644 = DIRECTION ( 'NONE',  ( 0.2756373558170018279, -0.9612616959383181170, 0.000000000000000000 ) ) ;
#10645 = AXIS2_PLACEMENT_3D ( 'NONE', #3380, #21253, #30800 ) ;
#10646 = LINE ( 'NONE', #15711, #31082 ) ;
#10647 = ORIENTED_EDGE ( 'NONE', *, *, #27239, .T. ) ;
#10648 = CIRCLE ( 'NONE', #28966, 1.899999999999999023 ) ;
#10649 = ADVANCED_FACE ( 'NONE', ( #4554 ), #120, .F. ) ;
#10650 = ORIENTED_EDGE ( 'NONE', *, *, #19336, .F. ) ;
#10651 = CARTESIAN_POINT ( 'NONE',  ( -10.95189920273699613, 2.529769287487948048, 99.96717447621844599 ) ) ;
#10652 = ADVANCED_FACE ( 'NONE', ( #14740 ), #7517, .F. ) ;
#10653 = VERTEX_POINT ( 'NONE', #24575 ) ;
#10654 = EDGE_CURVE ( 'NONE', #13496, #5375, #13200, .T. ) ;
#10655 = EDGE_CURVE ( 'NONE', #17361, #1375, #7872, .T. ) ;
#10656 = EDGE_CURVE ( 'NONE', #15237, #777, #10727, .T. ) ;
#10657 = VECTOR ( 'NONE', #281, 1000.000000000000000 ) ;
#10658 = ORIENTED_EDGE ( 'NONE', *, *, #4905, .F. ) ;
#10659 = AXIS2_PLACEMENT_3D ( 'NONE', #28852, #4051, #11443 ) ;
#10660 = DIRECTION ( 'NONE',  ( -1.000000000000000000, 0.000000000000000000, 0.000000000000000000 ) ) ;
#10661 = VERTEX_POINT ( 'NONE', #4392 ) ;
#10662 = DIRECTION ( 'NONE',  ( -0.9612616959383198934, -0.2756373558169956106, 0.000000000000000000 ) ) ;
#10663 = VECTOR ( 'NONE', #17115, 1000.000000000000000 ) ;
#10664 = VECTOR ( 'NONE', #15226, 1000.000000000000227 ) ;
#10665 = DIRECTION ( 'NONE',  ( -0.9612616959383205595, -0.2756373558169931681, 1.660411357259282445E-16 ) ) ;
#10666 = CARTESIAN_POINT ( 'NONE',  ( 21.09992658989239089, 26.96664230456639899, 47.04930799450051637 ) ) ;
#10667 = B_SPLINE_CURVE_WITH_KNOTS ( 'NONE', 3,
 ( #8473, #13082, #30963, #28172, #25380, #8154, #20450, #8308, #3212, #23077, #428, #13407, #30481, #18468, #12922, #23244, #28496, #20282, #17989, #598, #15210, #25223, #18144, #28336, #28010, #3373, #760, #20776, #2735, #22753, #5525, #5371, #12763, #10625, #18303, #5857, #15859, #10295, #23402, #30313, #20616, #7827 ),
 .UNSPECIFIED., .F., .F.,
 ( 4, 2, 2, 2, 2, 2, 2, 2, 2, 2, 2, 2, 2, 2, 2, 2, 2, 2, 2, 2, 4 ),
 ( 4.632855027873337708E-15, 0.0008474535421348709232, 0.001694907084265108834, 0.002542360626395347070, 0.003389814168525585088, 0.004237267710655822674, 0.005084721252786060693, 0.005932174794916298712, 0.006779628337046536730, 0.007627081879176774749, 0.008474535421307013636, 0.01016944250556750529, 0.01355925667408848338, 0.01525416375834898371, 0.01694907084260948230, 0.01864397792686998262, 0.02033888501113048294, 0.02203379209539098327, 0.02372869917965148012, 0.02542360626391198045, 0.02711851334817248771 ),
 .UNSPECIFIED. ) ;
#10668 = CARTESIAN_POINT ( 'NONE',  ( 49.44739180854976013, 25.93456182964376566, 47.17133137409169308 ) ) ;
#10669 = EDGE_CURVE ( 'NONE', #5852, #1546, #14411, .T. ) ;
#10670 = ORIENTED_EDGE ( 'NONE', *, *, #20568, .T. ) ;
#10671 = EDGE_LOOP ( 'NONE', ( #27517, #1020, #18088, #12924 ) ) ;
#10672 = DIRECTION ( 'NONE',  ( -0.4848096202463636484, -0.8746197071393810862, 0.000000000000000000 ) ) ;
#10673 = ORIENTED_EDGE ( 'NONE', *, *, #9539, .F. ) ;
#10674 = CARTESIAN_POINT ( 'NONE',  ( 47.34391502529295082, 10.06999148276586808, 98.42128873206745254 ) ) ;
#10675 = DIRECTION ( 'NONE',  ( -1.000000000000000000, 0.000000000000000000, 0.000000000000000000 ) ) ;
#10676 = CARTESIAN_POINT ( 'NONE',  ( 46.76672225489305390, 14.98691807112499141, 47.55973575893985839 ) ) ;
#10677 = LINE ( 'NONE', #20663, #6337 ) ;
#10678 = CARTESIAN_POINT ( 'NONE',  ( 45.24946171279598417, 25.62124452788248874, 47.99220971130007740 ) ) ;
#10679 = ORIENTED_EDGE ( 'NONE', *, *, #15375, .F. ) ;
#10680 = DIRECTION ( 'NONE',  ( -1.101824276508909887E-16, 1.000000000000000000, -0.000000000000000000 ) ) ;
#10681 = CARTESIAN_POINT ( 'NONE',  ( 8.698509210239560474, 29.34164230456639899, 47.04930799450051637 ) ) ;
#10682 = DIRECTION ( 'NONE',  ( 0.000000000000000000, 0.000000000000000000, -1.000000000000000000 ) ) ;
#10683 = CONICAL_SURFACE ( 'NONE', #16411, 67.17122696227043832, 1.291543646476234874 ) ;
#10684 = CARTESIAN_POINT ( 'NONE',  ( 8.698509210239555145, 28.84164230456639544, 47.04930799450051637 ) ) ;
#10685 = AXIS2_PLACEMENT_3D ( 'NONE', #22345, #22505, #12844 ) ;
#10686 = EDGE_CURVE ( 'NONE', #28686, #10826, #22108, .T. ) ;
#10687 = VERTEX_POINT ( 'NONE', #29675 ) ;
#10688 = CARTESIAN_POINT ( 'NONE',  ( -40.14651252454546437, 6.746025643617127088, 39.44930799450052206 ) ) ;
#10689 = CARTESIAN_POINT ( 'NONE',  ( 8.732853799281734553, 38.56284415653841791, 47.04930799450051637 ) ) ;
#10690 = ADVANCED_FACE ( 'NONE', ( #2581 ), #29899, .T. ) ;
#10691 = DIRECTION ( 'NONE',  ( 0.000000000000000000, 1.000000000000000000, 0.000000000000000000 ) ) ;
#10692 = CIRCLE ( 'NONE', #11207, 0.1250000000000001110 ) ;
#10693 = EDGE_LOOP ( 'NONE', ( #29968, #5521, #5395, #28759 ) ) ;
#10694 = VECTOR ( 'NONE', #24309, 1000.000000000000000 ) ;
#10695 = CIRCLE ( 'NONE', #16427, 47.39944366991822733 ) ;
#10696 = EDGE_CURVE ( 'NONE', #18648, #10357, #27265, .T. ) ;
#10697 = VERTEX_POINT ( 'NONE', #11944 ) ;
#10698 = ORIENTED_EDGE ( 'NONE', *, *, #1708, .F. ) ;
#10699 = DIRECTION ( 'NONE',  ( -2.779292025043186357E-18, 1.288349127009862211E-17, -1.000000000000000000 ) ) ;
#10700 = DIRECTION ( 'NONE',  ( -1.000000000000000000, 0.000000000000000000, 0.000000000000000000 ) ) ;
#10701 = DIRECTION ( 'NONE',  ( -0.000000000000000000, -1.000000000000000000, -0.000000000000000000 ) ) ;
#10702 = VERTEX_POINT ( 'NONE', #29514 ) ;
#10703 = CARTESIAN_POINT ( 'NONE',  ( -15.78477032795854207, -13.30632128221581389, 89.09797539074716610 ) ) ;
#10704 = LINE ( 'NONE', #13159, #8114 ) ;
#10705 = CARTESIAN_POINT ( 'NONE',  ( 21.09785597605720753, 13.86454579224779948, 47.04930799450052348 ) ) ;
#10706 = CARTESIAN_POINT ( 'NONE',  ( 52.67966335715245663, -5.832427868686510308, -10.56408697093867843 ) ) ;
#10708 = CIRCLE ( 'NONE', #16444, 0.1250000000000001110 ) ;
#10707 = DIRECTION ( 'NONE',  ( -1.101824276508909887E-16, 1.000000000000000000, -0.000000000000000000 ) ) ;
#10709 = CARTESIAN_POINT ( 'NONE',  ( 21.09785597605719332, 15.06454579224778456, -7.950692005499485404 ) ) ;
#10710 = LINE ( 'NONE', #15456, #22553 ) ;
#10711 = CYLINDRICAL_SURFACE ( 'NONE', #6833, 12.62506659569710266 ) ;
#10712 = CARTESIAN_POINT ( 'NONE',  ( 21.09992658989239089, 27.84184655352419568, 47.04930799450051637 ) ) ;
#10713 = ORIENTED_EDGE ( 'NONE', *, *, #27347, .T. ) ;
#10714 = ORIENTED_EDGE ( 'NONE', *, *, #12573, .F. ) ;
#10715 = DIRECTION ( 'NONE',  ( -0.4848096202463429427, -0.8746197071393925215, 2.352477780477436294E-16 ) ) ;
#10716 = DIRECTION ( 'NONE',  ( -1.000000000000000000, -1.101824276508909887E-16, 0.000000000000000000 ) ) ;
#10717 = CARTESIAN_POINT ( 'NONE',  ( 48.14399279324437231, 9.423225080673427456, 97.50315973084107668 ) ) ;
#10718 = VERTEX_POINT ( 'NONE', #12118 ) ;
#10719 = DIRECTION ( 'NONE',  ( -1.101824276508909887E-16, 1.000000000000000000, -0.000000000000000000 ) ) ;
#10720 = CARTESIAN_POINT ( 'NONE',  ( -40.06891218940336330, 7.538004613239522200, 38.80028690913361800 ) ) ;
#10721 = ORIENTED_EDGE ( 'NONE', *, *, #13761, .T. ) ;
#10722 = CARTESIAN_POINT ( 'NONE',  ( 21.09785597605719332, 7.094379510609982731, 47.04930799450051637 ) ) ;
#10723 = CARTESIAN_POINT ( 'NONE',  ( 48.83862994770794330, 28.04118040159426428, 48.17861352429476796 ) ) ;
#10724 = CARTESIAN_POINT ( 'NONE',  ( 45.79384627280941089, 29.17957786121581165, 49.05938063676249072 ) ) ;
#10725 = CARTESIAN_POINT ( 'NONE',  ( -34.42289002669387088, 11.86391215166791113, 53.48663982859374499 ) ) ;
#10726 = TOROIDAL_SURFACE ( 'NONE', #29594, 12.40141737965286772, 0.1250000000000003331 ) ;
#10727 =( BOUNDED_CURVE ( )  B_SPLINE_CURVE ( 3, ( #14903, #26879, #2260, #27040 ),
 .UNSPECIFIED., .F., .F. ) 
 B_SPLINE_CURVE_WITH_KNOTS ( ( 4, 4 ),
 ( 4.652534634851591022, 4.712388980384696779 ),
 .UNSPECIFIED. ) 
 CURVE ( )  GEOMETRIC_REPRESENTATION_ITEM ( )  RATIONAL_B_SPLINE_CURVE ( ( 1.000000000000000000, 0.9997014770583808607, 0.9997014770583808607, 1.000000000000000000 ) ) 
 REPRESENTATION_ITEM ( '' )  );
#10728 = CIRCLE ( 'NONE', #2322, 12.36707279061065279 ) ;
#10729 = CIRCLE ( 'NONE', #15954, 0.1250000000000001110 ) ;
#10730 = EDGE_CURVE ( 'NONE', #13336, #21573, #32137, .T. ) ;
#10731 = CIRCLE ( 'NONE', #9137, 19.99999999999999645 ) ;
#10732 = ORIENTED_EDGE ( 'NONE', *, *, #20720, .F. ) ;
#10733 = EDGE_CURVE ( 'NONE', #17822, #29138, #19806, .T. ) ;
#10734 = CARTESIAN_POINT ( 'NONE',  ( 8.698509210239544487, 27.84164230456639544, 47.04930799450051637 ) ) ;
#10735 = DIRECTION ( 'NONE',  ( 1.000000000000000000, 0.000000000000000000, 0.000000000000000000 ) ) ;
#10736 = VERTEX_POINT ( 'NONE', #22427 ) ;
#10737 = DIRECTION ( 'NONE',  ( -2.779292025043186357E-18, 1.288349127009862211E-17, -1.000000000000000000 ) ) ;
#10738 = CARTESIAN_POINT ( 'NONE',  ( -40.99173213700658636, 9.305078116158226109, 34.54930799450052348 ) ) ;
#10739 = CARTESIAN_POINT ( 'NONE',  ( 8.474859994195286461, 27.84143805560860940, 47.04930799450051637 ) ) ;
#10740 = ORIENTED_EDGE ( 'NONE', *, *, #18692, .T. ) ;
#10741 = LINE ( 'NONE', #11213, #6057 ) ;
#10742 = DIRECTION ( 'NONE',  ( -0.000000000000000000, 1.000000000000000000, -0.000000000000000000 ) ) ;
#10743 = CARTESIAN_POINT ( 'NONE',  ( 21.09785597605719332, 14.77310068074637961, 47.04930799450051637 ) ) ;
#10744 = CIRCLE ( 'NONE', #31188, 0.09999999999999940881 ) ;
#10745 = DIRECTION ( 'NONE',  ( 0.8746197071393926326, -0.4848096202463430537, -8.676864087101709653E-18 ) ) ;
#10746 = VECTOR ( 'NONE', #348, 1000.000000000000000 ) ;
#10747 = CARTESIAN_POINT ( 'NONE',  ( 47.09785597605719687, 19.86454579224779948, 47.04930799450078638 ) ) ;
#10748 = EDGE_LOOP ( 'NONE', ( #14450, #28468, #18628, #27259 ) ) ;
#10749 = CARTESIAN_POINT ( 'NONE',  ( 47.09785597605719687, 23.12036939723557083, 47.04930799450080059 ) ) ;
#10750 = DIRECTION ( 'NONE',  ( -1.224646799147353207E-16, -1.349345573449484691E-32, 1.000000000000000000 ) ) ;
#10751 = VECTOR ( 'NONE', #29831, 1000.000000000000114 ) ;
#10752 = AXIS2_PLACEMENT_3D ( 'NONE', #15113, #12501, #12669 ) ;
#10753 = DIRECTION ( 'NONE',  ( -1.000000000000000000, 0.000000000000000000, 0.000000000000000000 ) ) ;
#10754 = CARTESIAN_POINT ( 'NONE',  ( 33.46699938050303302, 38.56284415653841791, 47.04930799450051637 ) ) ;
#10755 = CIRCLE ( 'NONE', #14937, 65.75844861871138392 ) ;
#10756 = CARTESIAN_POINT ( 'NONE',  ( 21.09785597605720753, -14.04221034894631615, 105.9124997376166277 ) ) ;
#10757 = ORIENTED_EDGE ( 'NONE', *, *, #23846, .T. ) ;
#10758 = CARTESIAN_POINT ( 'NONE',  ( 21.09785597605719332, 15.63322284159649556, 47.04930799450051637 ) ) ;
#10759 = CARTESIAN_POINT ( 'NONE',  ( -40.59758774925371938, 7.567737757495683226, 38.66054537865625917 ) ) ;
#10760 = DIRECTION ( 'NONE',  ( -0.2756373558170082672, 0.9612616959383162296, 0.000000000000000000 ) ) ;
#10761 = ORIENTED_EDGE ( 'NONE', *, *, #25610, .T. ) ;
#10762 = LINE ( 'NONE', #3023, #12062 ) ;
#10763 = DIRECTION ( 'NONE',  ( 0.000000000000000000, 0.000000000000000000, -1.000000000000000000 ) ) ;
#10764 = DIRECTION ( 'NONE',  ( -0.4848096202463429982, -0.8746197071393925215, -9.920727850371698576E-18 ) ) ;
#10765 = CARTESIAN_POINT ( 'NONE',  ( 48.12593217812826651, 9.437824910247671895, -4.311094662169014491 ) ) ;
#10766 = EDGE_LOOP ( 'NONE', ( #9140, #8729, #24408, #8503 ) ) ;
#10767 = DIRECTION ( 'NONE',  ( 0.2756373558169974980, -0.9612616959383193382, -1.315048337272770589E-17 ) ) ;
#10768 = EDGE_LOOP ( 'NONE', ( #24611, #14453 ) ) ;
#10769 = ORIENTED_EDGE ( 'NONE', *, *, #19661, .F. ) ;
#10770 = ADVANCED_FACE ( 'NONE', ( #2427 ), #10497, .T. ) ;
#10771 = EDGE_CURVE ( 'NONE', #31740, #16313, #3731, .T. ) ;
#10772 = EDGE_CURVE ( 'NONE', #31154, #15339, #8907, .T. ) ;
#10773 = VECTOR ( 'NONE', #21658, 999.9999999999998863 ) ;
#10774 = EDGE_CURVE ( 'NONE', #2302, #456, #5366, .T. ) ;
#10775 = CIRCLE ( 'NONE', #23345, 12.36707279061065101 ) ;
#10776 = DIRECTION ( 'NONE',  ( 0.000000000000000000, 0.000000000000000000, -1.000000000000000000 ) ) ;
#10777 = CARTESIAN_POINT ( 'NONE',  ( 21.09785597605719332, 25.56454579224779877, 47.04930799450051637 ) ) ;
#10778 = DIRECTION ( 'NONE',  ( -0.9612616959383205595, -0.2756373558169931681, 1.660411357259282445E-16 ) ) ;
#10779 = ORIENTED_EDGE ( 'NONE', *, *, #3108, .T. ) ;
#10780 = DIRECTION ( 'NONE',  ( -1.101824276508909887E-16, 1.000000000000000000, -0.000000000000000000 ) ) ;
#10781 = ORIENTED_EDGE ( 'NONE', *, *, #24761, .T. ) ;
#10782 = CARTESIAN_POINT ( 'NONE',  ( -5.602943079677954685, 9.702389020015065313, 97.43646483284780402 ) ) ;
#10783 = CARTESIAN_POINT ( 'NONE',  ( -42.47434154250543514, 4.196643200812633978, 37.04930799450052348 ) ) ;
#10784 = DIRECTION ( 'NONE',  ( 2.779292025043186357E-18, -1.288349127009862211E-17, 1.000000000000000000 ) ) ;
#10785 = CARTESIAN_POINT ( 'NONE',  ( 8.474859994195282908, 38.56284415653841791, 47.04930799450051637 ) ) ;
#10787 = ORIENTED_EDGE ( 'NONE', *, *, #29768, .F. ) ;
#10786 = APPLICATION_CONTEXT ( 'automotive_design' ) ;
#10788 = DIRECTION ( 'NONE',  ( 0.3879443550132459229, 0.6998701428318346851, 0.5997340748914504749 ) ) ;
#10789 = ORIENTED_EDGE ( 'NONE', *, *, #22217, .F. ) ;
#10790 = DIRECTION ( 'NONE',  ( -1.101824276508909887E-16, 1.000000000000000000, -0.000000000000000000 ) ) ;
#10791 = ORIENTED_EDGE ( 'NONE', *, *, #16067, .T. ) ;
#10792 = CARTESIAN_POINT ( 'NONE',  ( 33.72499318558949710, 28.59143805560861296, 47.04930799450051637 ) ) ;
#10793 = CARTESIAN_POINT ( 'NONE',  ( 81.68481246222317793, -5.935668478901866330, 16.06795581775006099 ) ) ;
#10794 = DIRECTION ( 'NONE',  ( -1.000000000000000000, 0.000000000000000000, 0.000000000000000000 ) ) ;
#10795 = DIRECTION ( 'NONE',  ( -0.000000000000000000, -1.000000000000000000, -0.000000000000000000 ) ) ;
#10796 = DIRECTION ( 'NONE',  ( -0.000000000000000000, -1.000000000000000000, 0.000000000000000000 ) ) ;
#10797 = CIRCLE ( 'NONE', #29123, 0.1000000000000014905 ) ;
#10798 = EDGE_LOOP ( 'NONE', ( #13447, #30164, #15207, #19498 ) ) ;
#10799 = DIRECTION ( 'NONE',  ( -0.000000000000000000, -1.000000000000000000, -0.000000000000000000 ) ) ;
#10800 = CARTESIAN_POINT ( 'NONE',  ( -42.50976151518962354, 14.59907569580870224, 35.90717268343339441 ) ) ;
#10801 = VERTEX_POINT ( 'NONE', #7682 ) ;
#10803 = EDGE_CURVE ( 'NONE', #27773, #20495, #5380, .T. ) ;
#10802 = CARTESIAN_POINT ( 'NONE',  ( 21.09785597605719332, 25.56454579224779877, 44.12577010967610391 ) ) ;
#10804 = AXIS2_PLACEMENT_3D ( 'NONE', #15653, #23210, #26312 ) ;
#10805 = EDGE_CURVE ( 'NONE', #4648, #24129, #6359, .T. ) ;
#10806 = CIRCLE ( 'NONE', #25915, 0.4999999999999988343 ) ;
#10807 = DIRECTION ( 'NONE',  ( -1.000000000000000000, 0.000000000000000000, 0.000000000000000000 ) ) ;
#10808 = ORIENTED_EDGE ( 'NONE', *, *, #13669, .T. ) ;
#10809 = EDGE_LOOP ( 'NONE', ( #10757, #27382 ) ) ;
#10810 = CARTESIAN_POINT ( 'NONE',  ( -42.38351229602917414, 14.72295342448899014, 55.13902476097742777 ) ) ;
#10811 = UNCERTAINTY_MEASURE_WITH_UNIT (LENGTH_MEASURE( 1.000000000000000082E-05 ), #14172, 'distance_accuracy_value', 'NONE');
#10812 = AXIS2_PLACEMENT_3D ( 'NONE', #25615, #3117, #13154 ) ;
#10813 = ORIENTED_EDGE ( 'NONE', *, *, #29615, .F. ) ;
#10814 = EDGE_CURVE ( 'NONE', #20369, #3968, #20293, .T. ) ;
#10815 = ORIENTED_EDGE ( 'NONE', *, *, #14277, .T. ) ;
#10816 = DIRECTION ( 'NONE',  ( -1.188208965918165239E-16, -1.880121038077813132E-16, -1.000000000000000000 ) ) ;
#10817 = AXIS2_PLACEMENT_3D ( 'NONE', #31368, #8873, #31693 ) ;
#10818 = ORIENTED_EDGE ( 'NONE', *, *, #19745, .F. ) ;
#10819 = CARTESIAN_POINT ( 'NONE',  ( 47.60933809039193676, 23.04411619146718238, 48.05197954673941751 ) ) ;
#10820 = CARTESIAN_POINT ( 'NONE',  ( 21.09992658989239089, 24.09164230456639544, 47.04930799450051637 ) ) ;
#10821 = EDGE_CURVE ( 'NONE', #3234, #21817, #2098, .T. ) ;
#10822 = CARTESIAN_POINT ( 'NONE',  ( 48.91284552371730143, 27.39289516297709426, 46.12344667017377020 ) ) ;
#10823 = EDGE_LOOP ( 'NONE', ( #16705, #20310, #20252, #8866 ) ) ;
#10824 = ORIENTED_EDGE ( 'NONE', *, *, #3296, .T. ) ;
#10825 = DIRECTION ( 'NONE',  ( 1.000000000000000000, 0.000000000000000000, 0.000000000000000000 ) ) ;
#10826 = VERTEX_POINT ( 'NONE', #27692 ) ;
#10827 = ADVANCED_FACE ( 'NONE', ( #15540 ), #18315, .T. ) ;
#10828 = CIRCLE ( 'NONE', #16560, 0.3000000000000017653 ) ;
#10829 = CARTESIAN_POINT ( 'NONE',  ( 21.09785597605719332, 47.94190058235918173, 27.85932604141070001 ) ) ;
#10830 = CARTESIAN_POINT ( 'NONE',  ( 21.09785597605720753, 16.03967147762300982, 47.04930799450052348 ) ) ;
#10831 = CARTESIAN_POINT ( 'NONE',  ( 21.09992658989239089, 26.84164230456639899, 47.04930799450051637 ) ) ;
#10832 = CARTESIAN_POINT ( 'NONE',  ( 8.823509210239537381, 27.09164230456639899, 47.04930799450051637 ) ) ;
#10833 = DIRECTION ( 'NONE',  ( 0.000000000000000000, -1.000000000000000000, 0.000000000000000000 ) ) ;
#10834 = ORIENTED_EDGE ( 'NONE', *, *, #15281, .F. ) ;
#10835 = CARTESIAN_POINT ( 'NONE',  ( 21.09992658989239089, 30.59164230456639544, 47.04930799450051637 ) ) ;
#10836 = ADVANCED_FACE ( 'NONE', ( #13262 ), #17839, .F. ) ;
#10837 = CARTESIAN_POINT ( 'NONE',  ( 21.09992658989238734, 38.56284415653841791, 47.04930799450051637 ) ) ;
#10838 = EDGE_CURVE ( 'NONE', #15078, #25895, #5213, .T. ) ;
#10839 = CARTESIAN_POINT ( 'NONE',  ( 21.09785597605719332, 30.56554579224779644, 21.04930799450051282 ) ) ;
#10840 = CARTESIAN_POINT ( 'NONE',  ( 47.20547626766764893, 25.47451373492760140, 44.97710074790751378 ) ) ;
#10841 = ORIENTED_EDGE ( 'NONE', *, *, #11394, .F. ) ;
#10842 = DIRECTION ( 'NONE',  ( 0.000000000000000000, 0.000000000000000000, 1.000000000000000000 ) ) ;
#10843 = CARTESIAN_POINT ( 'NONE',  ( -40.58118912560991731, 7.466305082325866316, 53.91209753419874318 ) ) ;
#10844 = TOROIDAL_SURFACE ( 'NONE', #10322, 12.61792373059894601, 0.1249999999999988065 ) ;
#10845 = CYLINDRICAL_SURFACE ( 'NONE', #1730, 7.999999999999999112 ) ;
#10846 = ORIENTED_EDGE ( 'NONE', *, *, #31465, .F. ) ;
#10847 = EDGE_CURVE ( 'NONE', #20651, #15854, #17367, .T. ) ;
#10848 = AXIS2_PLACEMENT_3D ( 'NONE', #22313, #17386, #5084 ) ;
#10849 = ORIENTED_EDGE ( 'NONE', *, *, #21558, .T. ) ;
#10850 = ORIENTED_EDGE ( 'NONE', *, *, #396, .T. ) ;
#10851 = CARTESIAN_POINT ( 'NONE',  ( 48.68948053213853910, 22.89977464660286444, 46.07904489681320115 ) ) ;
#10852 = FACE_OUTER_BOUND ( 'NONE', #7529, .T. ) ;
#10853 = FACE_BOUND ( 'NONE', #19610, .T. ) ;
#10854 = ORIENTED_EDGE ( 'NONE', *, *, #13581, .T. ) ;
#10855 = CARTESIAN_POINT ( 'NONE',  ( 21.09785597605719687, -13.30631372918550959, -8.763520691563154941 ) ) ;
#10856 = FACE_OUTER_BOUND ( 'NONE', #9284, .T. ) ;
#10857 = EDGE_CURVE ( 'NONE', #8335, #253, #532, .T. ) ;
#10858 = AXIS2_PLACEMENT_3D ( 'NONE', #6462, #11381, #15986 ) ;
#10859 = ORIENTED_EDGE ( 'NONE', *, *, #5225, .F. ) ;
#10860 = CARTESIAN_POINT ( 'NONE',  ( 8.474859994195281132, 32.34184655352418503, 47.04930799450051637 ) ) ;
#10861 = EDGE_CURVE ( 'NONE', #21286, #23264, #15119, .T. ) ;
#10862 = CARTESIAN_POINT ( 'NONE',  ( -38.22595157131660670, -5.901281111979422178, 78.33466235588149118 ) ) ;
#10863 = CARTESIAN_POINT ( 'NONE',  ( -39.50554051497144314, 7.696103224718195968, 32.04930799450052348 ) ) ;
#10864 = CARTESIAN_POINT ( 'NONE',  ( -40.02540636251514172, 2.839176264122877047, 58.94930799450051495 ) ) ;
#10865 = DIRECTION ( 'NONE',  ( -1.000000000000000000, -1.101824276508910010E-16, 0.000000000000000000 ) ) ;
#10866 = CARTESIAN_POINT ( 'NONE',  ( -40.63136629056263160, 9.462201496834364178, 38.62930412971698502 ) ) ;
#10867 = CARTESIAN_POINT ( 'NONE',  ( 47.12319097693831793, 23.24793988701932079, 46.08163201552200405 ) ) ;
#10868 = ORIENTED_EDGE ( 'NONE', *, *, #2770, .F. ) ;
#10869 = ORIENTED_EDGE ( 'NONE', *, *, #32245, .T. ) ;
#10870 = CARTESIAN_POINT ( 'NONE',  ( 76.55093444394999835, -13.30632128221581567, 54.35510304470366094 ) ) ;
#10871 = CARTESIAN_POINT ( 'NONE',  ( -63.90214402394282445, 9.925589859889722533, 42.04930799450051637 ) ) ;
#10872 = ADVANCED_FACE ( 'NONE', ( #610 ), #3145, .T. ) ;
#10873 = AXIS2_PLACEMENT_3D ( 'NONE', #21739, #29140, #23725 ) ;
#10874 = ADVANCED_FACE ( 'NONE', ( #15700 ), #15732, .T. ) ;
#10875 = VERTEX_POINT ( 'NONE', #10947 ) ;
#10876 = DIRECTION ( 'NONE',  ( -1.000000000000000000, 0.000000000000000000, 0.000000000000000000 ) ) ;
#10877 = CARTESIAN_POINT ( 'NONE',  ( -40.18126594841541532, 7.055686659394005744, 39.15537800943240399 ) ) ;
#10878 = ORIENTED_EDGE ( 'NONE', *, *, #25498, .F. ) ;
#10879 = DIRECTION ( 'NONE',  ( 0.000000000000000000, 0.000000000000000000, -1.000000000000000000 ) ) ;
#10880 = CARTESIAN_POINT ( 'NONE',  ( 44.77625694075214824, 28.11454579807170617, 48.23360063142255427 ) ) ;
#10881 = CARTESIAN_POINT ( 'NONE',  ( 45.35708200440645044, 27.60457786121581947, 45.92000246470679770 ) ) ;
#10882 = CARTESIAN_POINT ( 'NONE',  ( -39.41803741763551017, -5.935648345809891424, 77.97613421639424303 ) ) ;
#10883 = CIRCLE ( 'NONE', #11918, 0.1249999999999983763 ) ;
#10884 = TOROIDAL_SURFACE ( 'NONE', #11398, 35.50000000000000711, 1.500000000000001332 ) ;
#10885 = ORIENTED_EDGE ( 'NONE', *, *, #19620, .T. ) ;
#10886 = CIRCLE ( 'NONE', #17158, 45.49665035954053138 ) ;
#10887 = CARTESIAN_POINT ( 'NONE',  ( -40.86580004447909431, 8.503105189880379555, 34.64930799450051779 ) ) ;
#10888 = CARTESIAN_POINT ( 'NONE',  ( -41.61831254958298132, 11.12742816935064738, 37.04930799450052348 ) ) ;
#10889 = VERTEX_POINT ( 'NONE', #8004 ) ;
#10890 = CARTESIAN_POINT ( 'NONE',  ( -42.63960953052571767, -0.7425051561549622647, 61.99930799450051921 ) ) ;
#10891 = CYLINDRICAL_SURFACE ( 'NONE', #4620, 12.62506659569710443 ) ;
#10892 = EDGE_CURVE ( 'NONE', #27923, #16423, #13709, .T. ) ;
#10893 = DIRECTION ( 'NONE',  ( -2.779292025043186357E-18, 1.288349127009862211E-17, -1.000000000000000000 ) ) ;
#10894 = ORIENTED_EDGE ( 'NONE', *, *, #24975, .T. ) ;
#10895 = PLANE ( 'NONE',  #30708 ) ;
#10896 = FACE_OUTER_BOUND ( 'NONE', #2159, .T. ) ;
#10897 = DIRECTION ( 'NONE',  ( -0.000000000000000000, -1.000000000000000000, -0.000000000000000000 ) ) ;
#10898 = CARTESIAN_POINT ( 'NONE',  ( -2.055626032295933214, 11.55977609614115842, -4.009591101970203297 ) ) ;
#10899 = ORIENTED_EDGE ( 'NONE', *, *, #22375, .T. ) ;
#10900 = CARTESIAN_POINT ( 'NONE',  ( 46.31918597887777622, 22.99884124225578930, 45.86695323169868033 ) ) ;
#10902 = CARTESIAN_POINT ( 'NONE',  ( 33.50134396954522487, 28.84164230456639544, 47.04930799450051637 ) ) ;
#10901 = AXIS2_PLACEMENT_3D ( 'NONE', #28643, #23718, #23073 ) ;
#10903 = CIRCLE ( 'NONE', #5145, 2.500000000000002220 ) ;
#10904 = DIRECTION ( 'NONE',  ( -1.000000000000000000, 0.000000000000000000, 0.000000000000000000 ) ) ;
#10905 = EDGE_CURVE ( 'NONE', #6106, #13785, #11268, .T. ) ;
#10906 = DIRECTION ( 'NONE',  ( -0.4848096202463431648, -0.8746197071393924105, 0.000000000000000000 ) ) ;
#10907 = CARTESIAN_POINT ( 'NONE',  ( 78.06792761052983565, -4.708525186292313869, 80.13239438898611411 ) ) ;
#10908 = ORIENTED_EDGE ( 'NONE', *, *, #14046, .F. ) ;
#10909 = CARTESIAN_POINT ( 'NONE',  ( 8.474859994195286461, 28.59143805560861296, 47.04930799450051637 ) ) ;
#10910 = CARTESIAN_POINT ( 'NONE',  ( 8.823509210239517842, 25.09164230456639899, 47.04930799450051637 ) ) ;
#10911 = DIRECTION ( 'NONE',  ( 0.000000000000000000, -1.000000000000000000, 0.000000000000000000 ) ) ;
#10912 = CIRCLE ( 'NONE', #11432, 12.36707279061065101 ) ;
#10913 = VERTEX_POINT ( 'NONE', #9118 ) ;
#10914 = DIRECTION ( 'NONE',  ( 0.7141240004913198547, -0.3958453973320100738, -0.5773502691896283956 ) ) ;
#10915 = B_SPLINE_CURVE_WITH_KNOTS ( 'NONE', 3,
 ( #30941, #10765, #18602, #28630, #3356, #23223, #13703, #739, #21224, #3188, #6142, #16143, #26161, #18282, #8760, #8452, #15669, #20756, #18130, #5836, #13387, #15839, #23704, #5509, #25841, #15514, #23054, #1208, #3027, #5990 ),
 .UNSPECIFIED., .F., .F.,
 ( 4, 2, 2, 2, 2, 2, 2, 2, 2, 2, 2, 2, 2, 2, 4 ),
 ( 0.000000000000000000, 0.001249755272498786519, 0.002499510544997573039, 0.003749265817496359558, 0.004999021089995146078, 0.007498531634992704371, 0.009998042179990264400, 0.01249755272498782183, 0.01374730799748660401, 0.01499706326998538446, 0.01562194090623477902, 0.01624681854248417184, 0.01749657381498295750, 0.01874632908748173968, 0.01999608435998052533 ),
 .UNSPECIFIED. ) ;
#10916 = CARTESIAN_POINT ( 'NONE',  ( 47.09785597605719687, 15.77906836436399374, 47.04930799450078638 ) ) ;
#10917 = CARTESIAN_POINT ( 'NONE',  ( 21.09992658989238734, 38.56284415653841791, 47.04930799450051637 ) ) ;
#10918 = CARTESIAN_POINT ( 'NONE',  ( 21.09992658989239089, 28.97145308207318237, 47.04930799450051637 ) ) ;
#10919 = VERTEX_POINT ( 'NONE', #31134 ) ;
#10920 = CARTESIAN_POINT ( 'NONE',  ( -42.59697395963048194, 14.54042610638008526, 37.04930799450052348 ) ) ;
#10921 = ORIENTED_EDGE ( 'NONE', *, *, #22486, .F. ) ;
#10922 = VERTEX_POINT ( 'NONE', #8484 ) ;
#10923 = CIRCLE ( 'NONE', #31377, 12.62506659569710266 ) ;
#10924 = CIRCLE ( 'NONE', #11970, 12.08499999999999552 ) ;
#10925 = CIRCLE ( 'NONE', #4090, 66.44011198581388555 ) ;
#10926 = AXIS2_PLACEMENT_3D ( 'NONE', #5701, #25727, #3233 ) ;
#10927 = CARTESIAN_POINT ( 'NONE',  ( 46.55854765242722948, 27.84696019071910555, 44.51792966461572831 ) ) ;
#10928 = DIRECTION ( 'NONE',  ( 2.779292025043186357E-18, -1.288349127009862211E-17, 1.000000000000000000 ) ) ;
#10929 = CARTESIAN_POINT ( 'NONE',  ( 21.09992658989239089, 24.84164230456639544, 47.04930799450051637 ) ) ;
#10930 = ORIENTED_EDGE ( 'NONE', *, *, #25318, .F. ) ;
#10931 = AXIS2_PLACEMENT_3D ( 'NONE', #13515, #26135, #23196 ) ;
#10932 = CARTESIAN_POINT ( 'NONE',  ( -35.64882101543633297, 9.925589859889722533, 42.04930799450051637 ) ) ;
#10933 = ORIENTED_EDGE ( 'NONE', *, *, #16837, .T. ) ;
#10934 = DIRECTION ( 'NONE',  ( 0.000000000000000000, -0.000000000000000000, -1.000000000000000000 ) ) ;
#10935 = CARTESIAN_POINT ( 'NONE',  ( -34.31970563170440158, 11.92558985988973497, 54.04930799450052348 ) ) ;
#10936 = CARTESIAN_POINT ( 'NONE',  ( 8.474859994195281132, 31.59184655352418503, 47.04930799450051637 ) ) ;
#10937 = FACE_OUTER_BOUND ( 'NONE', #29151, .T. ) ;
#10938 = VERTEX_POINT ( 'NONE', #26353 ) ;
#10939 = CARTESIAN_POINT ( 'NONE',  ( 46.49024570467398121, 14.98691807112498964, 47.01775166214249424 ) ) ;
#10940 = ORIENTED_EDGE ( 'NONE', *, *, #24108, .F. ) ;
#10941 = CARTESIAN_POINT ( 'NONE',  ( 8.573509210239590672, 32.59164230456639899, 47.04930799450051637 ) ) ;
#10942 = FACE_OUTER_BOUND ( 'NONE', #19087, .T. ) ;
#10943 = ORIENTED_EDGE ( 'NONE', *, *, #22450, .F. ) ;
#10944 = CARTESIAN_POINT ( 'NONE',  ( 21.09785597605719687, 30.36454579224777461, 78.54930799450052348 ) ) ;
#10945 = EDGE_CURVE ( 'NONE', #19345, #8205, #6658, .T. ) ;
#10946 = CARTESIAN_POINT ( 'NONE',  ( 21.09992658989238734, 30.97145308207317171, 47.04930799450051637 ) ) ;
#10947 = CARTESIAN_POINT ( 'NONE',  ( 34.29950969015405349, 17.36467600858027183, 47.04930799450052348 ) ) ;
#10948 = FACE_OUTER_BOUND ( 'NONE', #22242, .T. ) ;
#10949 = ADVANCED_FACE ( 'NONE', ( #20943 ), #7946, .T. ) ;
#10950 = CARTESIAN_POINT ( 'NONE',  ( 47.09785597605719687, 29.86454579224779948, 47.04930799450078638 ) ) ;
#10951 = EDGE_CURVE ( 'NONE', #29220, #104, #4795, .T. ) ;
#10952 = EDGE_LOOP ( 'NONE', ( #10978, #24728, #20216, #18278 ) ) ;
#10953 = CARTESIAN_POINT ( 'NONE',  ( 33.72499318558949710, 27.34143805560860940, 47.04930799450051637 ) ) ;
#10954 = EDGE_CURVE ( 'NONE', #23177, #15932, #13734, .T. ) ;
#10955 = ORIENTED_EDGE ( 'NONE', *, *, #29120, .T. ) ;
#10956 = B_SPLINE_CURVE_WITH_KNOTS ( 'NONE', 3,
 ( #16429, #3961, #1329, #26443, #1014, #21337, #8725, #28590, #8409, #31375 ),
 .UNSPECIFIED., .F., .F.,
 ( 4, 3, 3, 4 ),
 ( 0.000000000000000000, 3.349481945380948403E-05, 6.704430007368558935E-05, 7.824643346661451331E-05 ),
 .UNSPECIFIED. ) ;
#10957 = CARTESIAN_POINT ( 'NONE',  ( 81.63177831856063449, -5.935454207752202116, 16.07118271501079576 ) ) ;
#10958 = CIRCLE ( 'NONE', #29256, 0.1250000000000001110 ) ;
#10959 = AXIS2_PLACEMENT_3D ( 'NONE', #487, #28073, #30214 ) ;
#10960 = LINE ( 'NONE', #21108, #27945 ) ;
#10961 = CIRCLE ( 'NONE', #15647, 46.67448298906162307 ) ;
#10962 = ORIENTED_EDGE ( 'NONE', *, *, #16376, .T. ) ;
#10963 = ORIENTED_EDGE ( 'NONE', *, *, #8967, .T. ) ;
#10964 = CARTESIAN_POINT ( 'NONE',  ( -5.602943079677954685, 9.702389020015065313, 98.41455612196619995 ) ) ;
#10965 = AXIS2_PLACEMENT_3D ( 'NONE', #29392, #29562, #11836 ) ;
#10966 = ORIENTED_EDGE ( 'NONE', *, *, #19284, .T. ) ;
#10967 = EDGE_CURVE ( 'NONE', #22393, #30811, #31609, .T. ) ;
#10968 = ORIENTED_EDGE ( 'NONE', *, *, #21322, .T. ) ;
#10969 = CARTESIAN_POINT ( 'NONE',  ( 21.09992658989239089, 27.46183152705960850, 47.04930799450051637 ) ) ;
#10970 = EDGE_CURVE ( 'NONE', #18754, #30781, #21998, .T. ) ;
#10971 = VECTOR ( 'NONE', #25689, 1000.000000000000000 ) ;
#10972 = ORIENTED_EDGE ( 'NONE', *, *, #18961, .T. ) ;
#10973 = CARTESIAN_POINT ( 'NONE',  ( 48.21416462065301545, 23.04411657098542321, 47.25727406314477008 ) ) ;
#10974 = CARTESIAN_POINT ( 'NONE',  ( -40.46271621608484281, 3.081581074246049212, 58.54930799450051637 ) ) ;
#10975 = DIRECTION ( 'NONE',  ( 1.000000000000000000, -0.000000000000000000, 1.224646799147353207E-16 ) ) ;
#10976 = CARTESIAN_POINT ( 'NONE',  ( 48.16694854572211426, 25.81789516297710207, 49.14507740233662503 ) ) ;
#10977 = EDGE_LOOP ( 'NONE', ( #27871, #12803 ) ) ;
#10978 = ORIENTED_EDGE ( 'NONE', *, *, #14168, .F. ) ;
#10979 = EDGE_LOOP ( 'NONE', ( #30626, #4497, #943, #26818, #18126, #20314, #25103, #22210, #24276, #27130, #10834, #16903, #22311, #10227, #10921, #13227 ) ) ;
#10980 = AXIS2_PLACEMENT_3D ( 'NONE', #30537, #23136, #28229 ) ;
#10981 = CARTESIAN_POINT ( 'NONE',  ( 33.37634396954528171, 23.84164230456639544, 47.04930799450051637 ) ) ;
#10982 = CARTESIAN_POINT ( 'NONE',  ( 54.73929935417030634, -1.580002914024320360, 101.6640897793760558 ) ) ;
#10983 = DIRECTION ( 'NONE',  ( -1.000000000000000000, 0.000000000000000000, 0.000000000000000000 ) ) ;
#10984 = ADVANCED_FACE ( 'NONE', ( #26028 ), #11561, .T. ) ;
#10985 = EDGE_CURVE ( 'NONE', #5223, #272, #31477, .T. ) ;
#10986 = CARTESIAN_POINT ( 'NONE',  ( -4.668528339753533984, 10.39233698702945752, -4.365831785235375406 ) ) ;
#10987 = DIRECTION ( 'NONE',  ( -1.224646799147353207E-16, -1.349345573449484691E-32, 1.000000000000000000 ) ) ;
#10988 = EDGE_CURVE ( 'NONE', #20946, #14445, #15229, .T. ) ;
#10989 = CONTEXT_DEPENDENT_SHAPE_REPRESENTATION ( #17487, #18970 ) ;
#10990 = ORIENTED_EDGE ( 'NONE', *, *, #30344, .T. ) ;
#10991 = CARTESIAN_POINT ( 'NONE',  ( 21.09992658989239089, 24.84184655352419213, 47.04930799450051637 ) ) ;
#10992 = CARTESIAN_POINT ( 'NONE',  ( 21.09785597605719332, 25.56454579224779877, 73.04930799450052348 ) ) ;
#10993 = FACE_OUTER_BOUND ( 'NONE', #1222, .T. ) ;
#10994 = CARTESIAN_POINT ( 'NONE',  ( 48.66895200406656841, 25.66155426599986100, 44.62753372671560470 ) ) ;
#10995 = CARTESIAN_POINT ( 'NONE',  ( 47.20547626766765603, 26.87451373492759643, 44.97710074790751378 ) ) ;
#10996 = ORIENTED_EDGE ( 'NONE', *, *, #4018, .T. ) ;
#10997 = DIRECTION ( 'NONE',  ( -0.6184495258776538940, 0.3428121700606627242, 0.7071067811865505703 ) ) ;
#10998 = DIRECTION ( 'NONE',  ( 0.000000000000000000, 0.000000000000000000, -1.000000000000000000 ) ) ;
#10999 = CIRCLE ( 'NONE', #1535, 54.29999999999999716 ) ;
#11000 = AXIS2_PLACEMENT_3D ( 'NONE', #11551, #28957, #31099 ) ;
#11001 = ORIENTED_EDGE ( 'NONE', *, *, #9238, .F. ) ;
#11002 = ADVANCED_FACE ( 'NONE', ( #16177 ), #19921, .F. ) ;
#11003 = AXIS2_PLACEMENT_3D ( 'NONE', #15948, #20385, #3311 ) ;
#11004 = CIRCLE ( 'NONE', #18821, 0.1250000000000001110 ) ;
#11005 = TOROIDAL_SURFACE ( 'NONE', #23034, 44.50000000000000000, 1.499999999999995115 ) ;
#11006 = ORIENTED_EDGE ( 'NONE', *, *, #6044, .F. ) ;
#11007 = CARTESIAN_POINT ( 'NONE',  ( 49.98072202819530219, 25.66753733014356342, 47.19902993264913960 ) ) ;
#11008 = CIRCLE ( 'NONE', #2613, 2.800000000000002043 ) ;
#11009 = ADVANCED_FACE ( 'NONE', ( #16652 ), #18788, .F. ) ;
#11010 = DIRECTION ( 'NONE',  ( -1.000000000000000000, 0.000000000000000000, 0.000000000000000000 ) ) ;
#11011 = FACE_OUTER_BOUND ( 'NONE', #29600, .T. ) ;
#11012 = EDGE_CURVE ( 'NONE', #16025, #28129, #26518, .T. ) ;
#11013 = ORIENTED_EDGE ( 'NONE', *, *, #18640, .F. ) ;
#11014 = CARTESIAN_POINT ( 'NONE',  ( -34.35522249183560461, -13.30632128221581212, 54.35510304470367515 ) ) ;
#11015 = DIRECTION ( 'NONE',  ( 0.000000000000000000, 0.000000000000000000, 1.000000000000000000 ) ) ;
#11016 = FACE_OUTER_BOUND ( 'NONE', #6637, .T. ) ;
#11017 = VERTEX_POINT ( 'NONE', #16336 ) ;
#11018 = FACE_OUTER_BOUND ( 'NONE', #23719, .T. ) ;
#11019 = CONICAL_SURFACE ( 'NONE', #30390, 13.00000000000000533, 0.7853981633974482790 ) ;
#11020 = EDGE_LOOP ( 'NONE', ( #11488, #19697, #21229, #9239 ) ) ;
#11021 = DIRECTION ( 'NONE',  ( -1.000000000000000000, 0.000000000000000000, 0.000000000000000000 ) ) ;
#11022 = LINE ( 'NONE', #5605, #18090 ) ;
#11023 = DIRECTION ( 'NONE',  ( 1.000000000000000000, 0.000000000000000000, 0.000000000000000000 ) ) ;
#11024 = CARTESIAN_POINT ( 'NONE',  ( 33.37634396954523908, 27.34164230456639544, 47.04930799450051637 ) ) ;
#11025 = EDGE_CURVE ( 'NONE', #27059, #22946, #19949, .T. ) ;
#11026 =( NAMED_UNIT ( * ) PLANE_ANGLE_UNIT ( ) SI_UNIT ( $, .RADIAN. ) );
#11027 = ORIENTED_EDGE ( 'NONE', *, *, #27505, .T. ) ;
#11028 = ORIENTED_EDGE ( 'NONE', *, *, #14276, .F. ) ;
#11029 = CARTESIAN_POINT ( 'NONE',  ( 33.72499318558949000, 38.56284415653841791, 47.04930799450051637 ) ) ;
#11030 = CARTESIAN_POINT ( 'NONE',  ( 8.698509210239564027, 29.59164230456639899, 47.04930799450051637 ) ) ;
#11031 = AXIS2_PLACEMENT_3D ( 'NONE', #27369, #26878, #4391 ) ;
#11032 = TOROIDAL_SURFACE ( 'NONE', #9974, 12.61792373059894601, 0.1249999999999988065 ) ;
#11033 = DIRECTION ( 'NONE',  ( -1.101824276508909887E-16, 1.000000000000000000, -0.000000000000000000 ) ) ;
#11034 = ORIENTED_EDGE ( 'NONE', *, *, #19704, .F. ) ;
#11035 = PLANE ( 'NONE',  #18195 ) ;
#11036 = CIRCLE ( 'NONE', #1063, 0.09999999999999795164 ) ;
#11037 = PLANE ( 'NONE',  #10476 ) ;
#11038 = EDGE_LOOP ( 'NONE', ( #25315, #20747, #13087, #213 ) ) ;
#11039 = FACE_OUTER_BOUND ( 'NONE', #28908, .T. ) ;
#11040 = CIRCLE ( 'NONE', #18347, 12.27641737965287838 ) ;
#11041 = CARTESIAN_POINT ( 'NONE',  ( 49.41945501136223839, 27.06454579807170902, 45.86501535757901848 ) ) ;
#11042 = VECTOR ( 'NONE', #18089, 1000.000000000000114 ) ;
#11043 = AXIS2_PLACEMENT_3D ( 'NONE', #26844, #21746, #1240 ) ;
#11044 = CARTESIAN_POINT ( 'NONE',  ( -39.51039602574057596, -5.935454207752198563, 77.87546120947918382 ) ) ;
#11045 = EDGE_CURVE ( 'NONE', #6740, #18267, #2120, .T. ) ;
#11046 = EDGE_CURVE ( 'NONE', #19298, #3553, #3162, .T. ) ;
#11047 = VERTEX_POINT ( 'NONE', #4030 ) ;
#11048 = CARTESIAN_POINT ( 'NONE',  ( 33.72499318558949000, 38.56284415653841791, 47.04930799450051637 ) ) ;
#11049 = EDGE_CURVE ( 'NONE', #14608, #12345, #28326, .T. ) ;
#11050 = LINE ( 'NONE', #5801, #24390 ) ;
#11051 = EDGE_CURVE ( 'NONE', #2200, #2756, #21505, .T. ) ;
#11052 = AXIS2_PLACEMENT_3D ( 'NONE', #17672, #5212, #23089 ) ;
#11053 = EDGE_LOOP ( 'NONE', ( #22104, #25516 ) ) ;
#11054 = ADVANCED_FACE ( 'NONE', ( #19275 ), #14714, .T. ) ;
#11055 = AXIS2_PLACEMENT_3D ( 'NONE', #159, #2463, #17883 ) ;
#11056 = CARTESIAN_POINT ( 'NONE',  ( -40.08841711228579641, 7.575633567407562552, 53.80788663826320573 ) ) ;
#11057 = DIRECTION ( 'NONE',  ( -1.000000000000000000, 0.000000000000000000, 0.000000000000000000 ) ) ;
#11058 = CIRCLE ( 'NONE', #29402, 0.1000000000000011019 ) ;
#11059 = DIRECTION ( 'NONE',  ( 1.000000000000000000, 0.000000000000000000, 0.000000000000000000 ) ) ;
#11060 = VECTOR ( 'NONE', #8279, 1000.000000000000000 ) ;
#11061 = ORIENTED_EDGE ( 'NONE', *, *, #14950, .T. ) ;
#11062 = CARTESIAN_POINT ( 'NONE',  ( -41.95414548415062939, 13.78332541096821373, 54.54930799450052348 ) ) ;
#11063 = CARTESIAN_POINT ( 'NONE',  ( 8.482002859293391595, 23.71664230456639899, 47.04930799450051637 ) ) ;
#11064 = DIRECTION ( 'NONE',  ( 0.000000000000000000, 0.000000000000000000, -1.000000000000000000 ) ) ;
#11065 = CARTESIAN_POINT ( 'NONE',  ( 46.96819297411687444, 28.16988759933318676, 49.54594323136014822 ) ) ;
#11066 = SHAPE_REPRESENTATION_RELATIONSHIP ( 'NONE' , 'NONE' ,  #12446, #26470 ) ;
#11067 = ORIENTED_EDGE ( 'NONE', *, *, #17614, .F. ) ;
#11068 = CARTESIAN_POINT ( 'NONE',  ( 33.72499318558949710, 31.34184655352422766, 47.04930799450051637 ) ) ;
#11069 = CARTESIAN_POINT ( 'NONE',  ( -40.09211399732166115, 9.667069410243959382, 39.44930799450052206 ) ) ;
#11070 = AXIS2_PLACEMENT_3D ( 'NONE', #15060, #2746, #17671 ) ;
#11071 = CARTESIAN_POINT ( 'NONE',  ( -40.38239436982999564, 8.630641782992572786, 34.63740864294511823 ) ) ;
#11072 = DIRECTION ( 'NONE',  ( 0.000000000000000000, 0.000000000000000000, -1.000000000000000000 ) ) ;
#11073 = CARTESIAN_POINT ( 'NONE',  ( 77.52599780128986140, -4.161241697801461470, 80.45688245215025347 ) ) ;
#11074 = VERTEX_POINT ( 'NONE', #6821 ) ;
#11075 = DIRECTION ( 'NONE',  ( -0.000000000000000000, -1.000000000000000000, 0.000000000000000000 ) ) ;
#11076 = FACE_OUTER_BOUND ( 'NONE', #23500, .T. ) ;
#11077 = DIRECTION ( 'NONE',  ( -0.2756373558169897264, 0.9612616959383215587, 0.000000000000000000 ) ) ;
#11078 = VERTEX_POINT ( 'NONE', #16820 ) ;
#11079 = LINE ( 'NONE', #1369, #32494 ) ;
#11080 = DIRECTION ( 'NONE',  ( -1.000000000000000000, 0.000000000000000000, 0.000000000000000000 ) ) ;
#11081 = DIRECTION ( 'NONE',  ( -1.000000000000000000, 0.000000000000000000, 0.000000000000000000 ) ) ;
#11082 = CARTESIAN_POINT ( 'NONE',  ( 21.09785597605719332, 24.56454579224780232, 86.74871914086746472 ) ) ;
#11083 = ORIENTED_EDGE ( 'NONE', *, *, #8305, .F. ) ;
#11084 = CARTESIAN_POINT ( 'NONE',  ( 72.66245921547933051, 10.95084857405595535, 22.29041010318592697 ) ) ;
#11085 = AXIS2_PLACEMENT_3D ( 'NONE', #4893, #19980, #27865 ) ;
#11086 = ORIENTED_EDGE ( 'NONE', *, *, #4202, .T. ) ;
#11087 = ADVANCED_FACE ( 'NONE', ( #11905 ), #5808, .T. ) ;
#11088 = VECTOR ( 'NONE', #19438, 1000.000000000000000 ) ;
#11089 = CLOSED_SHELL ( 'NONE', ( #11976, #12196, #20562, #16220, #16828, #23744, #4619, #29072, #27954, #25969, #30219, #20760, #9417, #12506, #2522, #7989, #3403, #12783, #25681, #29200, #7535, #13720, #17709, #29097, #2992, #30244, #18553, #10537, #19562, #2345, #14462, #19590, #10462, #20997, #31901, #13045, #2071, #20605, #11927, #19089, #9297, #21742, #23190, #9827, #14686, #17203, #616, #25687, #29656, #30678, #17631, #4072, #6750, #7242, #19866, #7952, #2182, #8370, #22852, #13284, #2407, #9536, #3970, #6630, #27886, #6046, #28671, #15971, #7033, #1432, #18334, #31296, #23639, #8780, #24987, #16346, #22936, #27269, #2193, #20488, #4375, #17062, #8930, #10449, #29351, #17776, #7542, #6350, #28133, #21149, #14971, #21186, #12825, #13020, #26451, #31306, #3443, #14355, #12543, #13359, #19448, #5420, #23130, #21598, #31756, #24229, #20199, #19401, #22566, #16039, #14244, #28309, #16475, #8232, #28529, #14274, #25796, #416 ) ) ;
#11090 = VECTOR ( 'NONE', #564, 1000.000000000000000 ) ;
#11091 = EDGE_CURVE ( 'NONE', #20897, #22868, #25725, .T. ) ;
#11092 = ORIENTED_EDGE ( 'NONE', *, *, #16249, .F. ) ;
#11093 = AXIS2_PLACEMENT_3D ( 'NONE', #17425, #25309, #27446 ) ;
#11094 = EDGE_CURVE ( 'NONE', #15585, #11769, #20469, .T. ) ;
#11095 = EDGE_CURVE ( 'NONE', #22848, #16786, #651, .T. ) ;
#11096 = CARTESIAN_POINT ( 'NONE',  ( 21.09992658989239089, 27.84164230456639544, 47.04930799450051637 ) ) ;
#11097 = DIRECTION ( 'NONE',  ( -1.000000000000000000, -1.101824276508909887E-16, 0.000000000000000000 ) ) ;
#11098 = CARTESIAN_POINT ( 'NONE',  ( 21.09785597605720753, -5.098646251524523443, 47.04930799450052348 ) ) ;
#11099 = VERTEX_POINT ( 'NONE', #31386 ) ;
#11100 = CARTESIAN_POINT ( 'NONE',  ( 21.09785597605720042, 12.78350261226561280, 102.7736706386835408 ) ) ;
#11101 = ORIENTED_EDGE ( 'NONE', *, *, #24199, .T. ) ;
#11102 = CARTESIAN_POINT ( 'NONE',  ( -43.38408989745150990, 1.111547985471239341, 60.54930799450051637 ) ) ;
#11103 = AXIS2_PLACEMENT_3D ( 'NONE', #28662, #926, #3059 ) ;
#11104 = DIRECTION ( 'NONE',  ( -0.000000000000000000, -1.000000000000000000, -0.000000000000000000 ) ) ;
#11105 = SPHERICAL_SURFACE ( 'NONE', #41, 0.1000000000000000056 ) ;
#11106 = EDGE_LOOP ( 'NONE', ( #25024, #16389, #13967, #14685 ) ) ;
#11107 = DIRECTION ( 'NONE',  ( -1.101824276508909887E-16, 1.000000000000000000, -0.000000000000000000 ) ) ;
#11108 = ORIENTED_EDGE ( 'NONE', *, *, #21432, .F. ) ;
#11109 = CARTESIAN_POINT ( 'NONE',  ( -40.46271621608484281, 3.081581074246050544, 61.94930799450052206 ) ) ;
#11110 = FACE_OUTER_BOUND ( 'NONE', #25376, .T. ) ;
#11111 = ORIENTED_EDGE ( 'NONE', *, *, #31947, .F. ) ;
#11112 = CARTESIAN_POINT ( 'NONE',  ( 46.71980555233013632, 23.04411657098542676, 45.97857331549464277 ) ) ;
#11113 = CARTESIAN_POINT ( 'NONE',  ( -40.60722745863126448, 9.415333058485023443, 35.49072935073782986 ) ) ;
#11114 = DIRECTION ( 'NONE',  ( 0.000000000000000000, 0.000000000000000000, -1.000000000000000000 ) ) ;
#11115 = CARTESIAN_POINT ( 'NONE',  ( 46.59785597605721108, 13.86454579224779948, 47.04930799450052348 ) ) ;
#11116 = DIRECTION ( 'NONE',  ( -0.000000000000000000, -1.000000000000000000, -0.000000000000000000 ) ) ;
#11117 = ORIENTED_EDGE ( 'NONE', *, *, #25020, .T. ) ;
#11118 = CARTESIAN_POINT ( 'NONE',  ( 33.46699938050303302, 38.56284415653841791, 47.04930799450051637 ) ) ;
#11119 = CARTESIAN_POINT ( 'NONE',  ( -40.57420052961218460, 7.102220148651144704, 35.23168232079561335 ) ) ;
#11120 = ORIENTED_EDGE ( 'NONE', *, *, #12358, .F. ) ;
#11121 = CARTESIAN_POINT ( 'NONE',  ( -41.61831254958298132, 11.12742816935064916, 35.90717268343339441 ) ) ;
#11122 = AXIS2_PLACEMENT_3D ( 'NONE', #31450, #16333, #6656 ) ;
#11123 = DIRECTION ( 'NONE',  ( -1.101824276508909887E-16, 1.000000000000000000, -0.000000000000000000 ) ) ;
#11124 = ORIENTED_EDGE ( 'NONE', *, *, #4575, .F. ) ;
#11125 = ORIENTED_EDGE ( 'NONE', *, *, #3172, .F. ) ;
#11126 = PRODUCT_DEFINITION_CONTEXT ( 'detailed design', #3625, 'design' ) ;
#11127 = CIRCLE ( 'NONE', #6916, 0.1249999999999983763 ) ;
#11128 = ORIENTED_EDGE ( 'NONE', *, *, #2631, .F. ) ;
#11129 = CIRCLE ( 'NONE', #23696, 1.700000000000007061 ) ;
#11130 = EDGE_CURVE ( 'NONE', #8185, #11449, #27281, .T. ) ;
#11131 = PRODUCT_DEFINITION_SHAPE ( 'NONE', 'NONE',  #32504 ) ;
#11132 = EDGE_CURVE ( 'NONE', #8819, #30210, #6835, .T. ) ;
#11133 = EDGE_LOOP ( 'NONE', ( #25821, #18214, #26039, #17630 ) ) ;
#11134 = CARTESIAN_POINT ( 'NONE',  ( 80.77181806311268986, -3.295808585244882849, 11.79002343214943238 ) ) ;
#11135 = AXIS2_PLACEMENT_3D ( 'NONE', #17476, #2388, #27496 ) ;
#11136 = ORIENTED_EDGE ( 'NONE', *, *, #11565, .T. ) ;
#11137 = TOROIDAL_SURFACE ( 'NONE', #20566, 12.61792373059895667, 0.1249999999999982098 ) ;
#11138 = CARTESIAN_POINT ( 'NONE',  ( 47.92168837363949052, 23.03451764446790051, 47.93439649084938736 ) ) ;
#11139 = DIRECTION ( 'NONE',  ( -1.000000000000000000, -1.101824276508909764E-16, 0.000000000000000000 ) ) ;
#11140 = DIRECTION ( 'NONE',  ( -0.000000000000000000, 1.000000000000000000, -0.000000000000000000 ) ) ;
#11141 = CARTESIAN_POINT ( 'NONE',  ( 47.20353132263855400, 28.20956182964376069, 45.01455027646040463 ) ) ;
#11142 = ORIENTED_EDGE ( 'NONE', *, *, #4254, .T. ) ;
#11143 = VERTEX_POINT ( 'NONE', #11850 ) ;
#11144 = DIRECTION ( 'NONE',  ( -0.000000000000000000, -1.000000000000000000, -0.000000000000000000 ) ) ;
#11145 = VERTEX_POINT ( 'NONE', #21845 ) ;
#11146 = AXIS2_PLACEMENT_3D ( 'NONE', #13765, #11144, #16053 ) ;
#11147 = CARTESIAN_POINT ( 'NONE',  ( -40.66259927863510626, 6.843847033175615380, 39.31544081796293710 ) ) ;
#11148 = DIRECTION ( 'NONE',  ( 0.000000000000000000, 0.000000000000000000, -1.000000000000000000 ) ) ;
#11149 = DIRECTION ( 'NONE',  ( 0.000000000000000000, -1.000000000000000000, 0.000000000000000000 ) ) ;
#11150 = CARTESIAN_POINT ( 'NONE',  ( -5.602943079677954685, 9.702389020015065313, -4.315940132965163656 ) ) ;
#11151 = DIRECTION ( 'NONE',  ( -7.588956326749211550E-18, 4.206627182996911684E-18, -1.000000000000000000 ) ) ;
#11152 = ORIENTED_EDGE ( 'NONE', *, *, #3337, .T. ) ;
#11153 = PLANE ( 'NONE',  #14587 ) ;
#11154 = CYLINDRICAL_SURFACE ( 'NONE', #10443, 0.1000000000000018235 ) ;
#11155 = DIRECTION ( 'NONE',  ( -1.101824276508909887E-16, 1.000000000000000000, -0.000000000000000000 ) ) ;
#11156 = FACE_OUTER_BOUND ( 'NONE', #24348, .T. ) ;
#11157 = EDGE_LOOP ( 'NONE', ( #12436, #18311 ) ) ;
#11158 = CARTESIAN_POINT ( 'NONE',  ( 48.94625023931840246, 25.35784706826093426, 46.10640627770148825 ) ) ;
#11159 = ORIENTED_EDGE ( 'NONE', *, *, #1245, .T. ) ;
#11160 = CARTESIAN_POINT ( 'NONE',  ( -40.71976880025163581, 7.963440923891331735, 57.04930799450051637 ) ) ;
#11161 = DIRECTION ( 'NONE',  ( -1.101824276508909887E-16, 1.000000000000000000, -0.000000000000000000 ) ) ;
#11162 = ORIENTED_EDGE ( 'NONE', *, *, #21700, .F. ) ;
#11163 = AXIS2_PLACEMENT_3D ( 'NONE', #2938, #12968, #10983 ) ;
#11164 = CIRCLE ( 'NONE', #29505, 12.62506659569710266 ) ;
#11165 = EDGE_CURVE ( 'NONE', #20447, #24091, #18263, .T. ) ;
#11166 = EDGE_CURVE ( 'NONE', #19917, #3984, #6272, .T. ) ;
#11167 = EDGE_CURVE ( 'NONE', #11099, #26330, #27808, .T. ) ;
#11168 = AXIS2_PLACEMENT_3D ( 'NONE', #27991, #22564, #22736 ) ;
#11169 = ORIENTED_EDGE ( 'NONE', *, *, #519, .T. ) ;
#11170 = ADVANCED_FACE ( 'NONE', ( #26457 ), #3644, .T. ) ;
#11171 = DIRECTION ( 'NONE',  ( -0.000000000000000000, -1.000000000000000000, -0.000000000000000000 ) ) ;
#11172 = CARTESIAN_POINT ( 'NONE',  ( -40.06561427811386267, 7.496110634155836117, 60.54930799450051637 ) ) ;
#11173 = FACE_OUTER_BOUND ( 'NONE', #6082, .T. ) ;
#11174 = EDGE_LOOP ( 'NONE', ( #15901, #15690, #15323, #16225 ) ) ;
#11175 = DIRECTION ( 'NONE',  ( 1.000000000000000000, 0.000000000000000000, 0.000000000000000000 ) ) ;
#11176 = LINE ( 'NONE', #23642, #28561 ) ;
#11177 = ORIENTED_EDGE ( 'NONE', *, *, #8746, .T. ) ;
#11178 = LINE ( 'NONE', #16408, #3521 ) ;
#11179 = ORIENTED_EDGE ( 'NONE', *, *, #30945, .T. ) ;
#11180 = DIRECTION ( 'NONE',  ( 0.000000000000000000, 0.000000000000000000, 1.000000000000000000 ) ) ;
#11181 = CARTESIAN_POINT ( 'NONE',  ( 47.62434977220233634, 29.18891845522693274, 44.62129988634950450 ) ) ;
#11182 = AXIS2_PLACEMENT_3D ( 'NONE', #25070, #10142, #25238 ) ;
#11183 = CARTESIAN_POINT ( 'NONE',  ( -40.68127404237834099, 6.801539337588502931, 34.61638395550082237 ) ) ;
#11184 = CIRCLE ( 'NONE', #15373, 0.1249999999999966416 ) ;
#11185 = ORIENTED_EDGE ( 'NONE', *, *, #15240, .F. ) ;
#11186 = EDGE_LOOP ( 'NONE', ( #24099, #12792, #20130, #24245 ) ) ;
#11187 = CARTESIAN_POINT ( 'NONE',  ( -40.02540636251513462, 2.839176264122873050, 35.04930799450051637 ) ) ;
#11188 = FACE_OUTER_BOUND ( 'NONE', #11726, .T. ) ;
#11189 = CARTESIAN_POINT ( 'NONE',  ( 21.09785597605719332, 25.56454579224779877, 47.04930799450051637 ) ) ;
#11190 = ORIENTED_EDGE ( 'NONE', *, *, #17068, .F. ) ;
#11191 =( BOUNDED_CURVE ( )  B_SPLINE_CURVE ( 3, ( #37, #350, #7917, #10373 ),
 .UNSPECIFIED., .F., .F. ) 
 B_SPLINE_CURVE_WITH_KNOTS ( ( 4, 4 ),
 ( 5.062864179022702693, 5.184122060454624759 ),
 .UNSPECIFIED. ) 
 CURVE ( )  GEOMETRIC_REPRESENTATION_ITEM ( )  RATIONAL_B_SPLINE_CURVE ( ( 1.000000000000000000, 0.9987750858034806223, 0.9987750858034806223, 1.000000000000000000 ) ) 
 REPRESENTATION_ITEM ( '' )  );
#11192 = FACE_OUTER_BOUND ( 'NONE', #27957, .T. ) ;
#11193 = CYLINDRICAL_SURFACE ( 'NONE', #18323, 12.27848799348799069 ) ;
#11194 = ORIENTED_EDGE ( 'NONE', *, *, #15234, .F. ) ;
#11195 = CARTESIAN_POINT ( 'NONE',  ( -40.63136629056263160, 9.462201496834364178, 34.66931185928405057 ) ) ;
#11196 = CARTESIAN_POINT ( 'NONE',  ( 49.41945501136223839, 29.86454579807170262, 45.86501535757901848 ) ) ;
#11197 = EDGE_CURVE ( 'NONE', #9081, #10697, #26740, .T. ) ;
#11198 = EDGE_CURVE ( 'NONE', #19299, #9250, #13662, .T. ) ;
#11199 = CARTESIAN_POINT ( 'NONE',  ( -40.75848109938849717, 9.580021662090986823, 38.54930799450052348 ) ) ;
#11200 = VERTEX_POINT ( 'NONE', #13671 ) ;
#11201 = CIRCLE ( 'NONE', #5425, 0.1250000000000001110 ) ;
#11202 = EDGE_CURVE ( 'NONE', #30206, #5667, #26514, .T. ) ;
#11203 = FACE_OUTER_BOUND ( 'NONE', #4219, .T. ) ;
#11204 = CARTESIAN_POINT ( 'NONE',  ( 48.66895200406656130, 28.58420399681022062, 44.62753372671561181 ) ) ;
#11205 = DIRECTION ( 'NONE',  ( 0.8746197071393858602, -0.4848096202463547666, 0.000000000000000000 ) ) ;
#11206 = EDGE_LOOP ( 'NONE', ( #7983, #18087, #1212, #20499 ) ) ;
#11207 = AXIS2_PLACEMENT_3D ( 'NONE', #22889, #27502, #25362 ) ;
#11208 = VECTOR ( 'NONE', #1824, 1000.000000000000000 ) ;
#11209 = CARTESIAN_POINT ( 'NONE',  ( -40.61178118339597631, 9.038025460530262123, 57.95249952744806166 ) ) ;
#11210 = FACE_OUTER_BOUND ( 'NONE', #17218, .T. ) ;
#11211 = CARTESIAN_POINT ( 'NONE',  ( 71.63986567979446818, 8.190330151142699577, 18.74290927009450058 ) ) ;
#11212 = ORIENTED_EDGE ( 'NONE', *, *, #27096, .F. ) ;
#11213 = CARTESIAN_POINT ( 'NONE',  ( 7.282982007932096380, 15.57592086119046826, 47.04930799450052348 ) ) ;
#11214 = DIRECTION ( 'NONE',  ( -1.000000000000000000, 0.000000000000000000, 0.000000000000000000 ) ) ;
#11215 = CARTESIAN_POINT ( 'NONE',  ( 21.09785597605720753, 14.86454579224779948, 47.04930799450052348 ) ) ;
#11216 = EDGE_CURVE ( 'NONE', #5139, #7595, #2643, .T. ) ;
#11217 = DIRECTION ( 'NONE',  ( -1.000000000000000000, 0.000000000000000000, 0.000000000000000000 ) ) ;
#11218 = ORIENTED_EDGE ( 'NONE', *, *, #1174, .F. ) ;
#11219 = FACE_OUTER_BOUND ( 'NONE', #13766, .T. ) ;
#11220 = CARTESIAN_POINT ( 'NONE',  ( 45.35708200440645044, 29.00457786121581805, 45.92000246470680480 ) ) ;
#11221 = DIRECTION ( 'NONE',  ( 0.2250569586005335410, -0.7848668881104262640, -0.5773502691896259531 ) ) ;
#11222 = EDGE_CURVE ( 'NONE', #9700, #13764, #29922, .T. ) ;
#11223 = CARTESIAN_POINT ( 'NONE',  ( -40.11688989807090167, 6.803825020423235337, 34.64825762772819218 ) ) ;
#11224 = DIRECTION ( 'NONE',  ( -0.000000000000000000, -1.000000000000000000, 0.000000000000000000 ) ) ;
#11225 = CIRCLE ( 'NONE', #26939, 12.62506659569710443 ) ;
#11226 = VERTEX_POINT ( 'NONE', #13831 ) ;
#11227 = DIRECTION ( 'NONE',  ( -1.101824276508909887E-16, 1.000000000000000000, -0.000000000000000000 ) ) ;
#11228 = DIRECTION ( 'NONE',  ( -1.000000000000000000, 0.000000000000000000, 0.000000000000000000 ) ) ;
#11229 = CARTESIAN_POINT ( 'NONE',  ( -40.11729073372970333, 6.802967823440400075, 34.64930799450051779 ) ) ;
#11230 = ORIENTED_EDGE ( 'NONE', *, *, #28933, .T. ) ;
#11231 = B_SPLINE_CURVE_WITH_KNOTS ( 'NONE', 3,
 ( #25433, #22804, #10507, #5575, #2939, #5415 ),
 .UNSPECIFIED., .F., .F.,
 ( 4, 2, 4 ),
 ( 0.000000000000000000, 0.5000000000000000000, 1.000000000000000000 ),
 .UNSPECIFIED. ) ;
#11232 = DIRECTION ( 'NONE',  ( -1.000000000000000000, 0.000000000000000000, 0.000000000000000000 ) ) ;
#11233 = SPHERICAL_SURFACE ( 'NONE', #6256, 0.1000000000000000056 ) ;
#11234 = ADVANCED_FACE ( 'NONE', ( #23676 ), #24149, .F. ) ;
#11235 = ADVANCED_FACE ( 'NONE', ( #21346 ), #19051, .T. ) ;
#11236 = CARTESIAN_POINT ( 'NONE',  ( -42.37913764077812573, 15.23192269303852697, 38.44930799450052916 ) ) ;
#11237 = CARTESIAN_POINT ( 'NONE',  ( 21.09785597605719332, -15.93545420775219945, 47.04930799450051637 ) ) ;
#11238 = EDGE_CURVE ( 'NONE', #14754, #7305, #26221, .T. ) ;
#11239 = ORIENTED_EDGE ( 'NONE', *, *, #14763, .F. ) ;
#11240 = CYLINDRICAL_SURFACE ( 'NONE', #31398, 37.50000000000000711 ) ;
#11241 = EDGE_LOOP ( 'NONE', ( #732, #6440, #13404, #8436 ) ) ;
#11242 = EDGE_LOOP ( 'NONE', ( #4946, #5025, #5079 ) ) ;
#11243 = EDGE_CURVE ( 'NONE', #2021, #22668, #6312, .T. ) ;
#11244 = CIRCLE ( 'NONE', #4422, 85.00000000000001421 ) ;
#11245 = CYLINDRICAL_SURFACE ( 'NONE', #2405, 0.1000000000000007272 ) ;
#11246 = DIRECTION ( 'NONE',  ( -0.000000000000000000, -1.000000000000000000, -0.000000000000000000 ) ) ;
#11247 = AXIS2_PLACEMENT_3D ( 'NONE', #3045, #20615, #12762 ) ;
#11248 = DIRECTION ( 'NONE',  ( -1.000000000000000000, 0.000000000000000000, 0.000000000000000000 ) ) ;
#11249 = AXIS2_PLACEMENT_3D ( 'NONE', #602, #24902, #18944 ) ;
#11250 = AXIS2_PLACEMENT_3D ( 'NONE', #25127, #1981, #4941 ) ;
#11251 = ORIENTED_EDGE ( 'NONE', *, *, #6520, .F. ) ;
#11252 = DIRECTION ( 'NONE',  ( 0.7141240004913198547, -0.3958453973320100738, 0.5773502691896283956 ) ) ;
#11253 = ORIENTED_EDGE ( 'NONE', *, *, #31267, .T. ) ;
#11254 = AXIS2_PLACEMENT_3D ( 'NONE', #20522, #338, #20353 ) ;
#11255 = DIRECTION ( 'NONE',  ( -1.000000000000000000, -1.101824276508909887E-16, 0.000000000000000000 ) ) ;
#11256 = DIRECTION ( 'NONE',  ( 0.000000000000000000, -0.000000000000000000, -1.000000000000000000 ) ) ;
#11257 = EDGE_CURVE ( 'NONE', #3723, #3559, #11040, .T. ) ;
#11258 = CARTESIAN_POINT ( 'NONE',  ( -5.144846497709795408, 10.07270486929682107, 97.52097793833394235 ) ) ;
#11259 = ORIENTED_EDGE ( 'NONE', *, *, #13950, .F. ) ;
#11260 = DIRECTION ( 'NONE',  ( 0.000000000000000000, 0.000000000000000000, -1.000000000000000000 ) ) ;
#11261 = DIRECTION ( 'NONE',  ( -0.000000000000000000, -1.000000000000000000, 0.000000000000000000 ) ) ;
#11262 = PLANE ( 'NONE',  #1305 ) ;
#11263 = DIRECTION ( 'NONE',  ( 2.779292025043186357E-18, -1.288349127009862211E-17, 1.000000000000000000 ) ) ;
#11264 = ORIENTED_EDGE ( 'NONE', *, *, #21249, .F. ) ;
#11265 = FACE_OUTER_BOUND ( 'NONE', #17695, .T. ) ;
#11266 = EDGE_CURVE ( 'NONE', #30099, #16025, #4210, .T. ) ;
#11267 = CARTESIAN_POINT ( 'NONE',  ( 33.50134396954521065, 29.84164230456639899, 47.04930799450051637 ) ) ;
#11268 = LINE ( 'NONE', #28658, #18929 ) ;
#11269 = FACE_OUTER_BOUND ( 'NONE', #12536, .T. ) ;
#11270 = ORIENTED_EDGE ( 'NONE', *, *, #3965, .F. ) ;
#11271 = CARTESIAN_POINT ( 'NONE',  ( 71.55936645880203173, 9.702389020015065313, 20.34850893876554423 ) ) ;
#11272 = CARTESIAN_POINT ( 'NONE',  ( -40.56500720768330837, 7.149487417330789185, 35.17537323039149300 ) ) ;
#11273 = EDGE_LOOP ( 'NONE', ( #17530, #29469, #23046, #19047 ) ) ;
#11274 = CARTESIAN_POINT ( 'NONE',  ( 8.732853799281738105, 25.46183152705960140, 47.04930799450051637 ) ) ;
#11275 = EDGE_CURVE ( 'NONE', #13490, #11782, #30951, .T. ) ;
#11276 = FACE_OUTER_BOUND ( 'NONE', #5282, .T. ) ;
#11277 = EDGE_LOOP ( 'NONE', ( #1903, #21909 ) ) ;
#11278 = CONICAL_SURFACE ( 'NONE', #29616, 72.49999999999997158, 0.7853981633974482790 ) ;
#11279 = VERTEX_POINT ( 'NONE', #17508 ) ;
#11280 = CIRCLE ( 'NONE', #15472, 12.73401709983438401 ) ;
#11281 = AXIS2_PLACEMENT_3D ( 'NONE', #22064, #19106, #24702 ) ;
#11282 = AXIS2_PLACEMENT_3D ( 'NONE', #765, #18473, #17995 ) ;
#11283 = AXIS2_PLACEMENT_3D ( 'NONE', #25414, #24933, #25094 ) ;
#11284 = ORIENTED_EDGE ( 'NONE', *, *, #22238, .T. ) ;
#11285 = ORIENTED_EDGE ( 'NONE', *, *, #26756, .T. ) ;
#11286 = DIRECTION ( 'NONE',  ( 0.000000000000000000, 0.000000000000000000, -1.000000000000000000 ) ) ;
#11287 = ORIENTED_EDGE ( 'NONE', *, *, #29250, .F. ) ;
#11288 = CARTESIAN_POINT ( 'NONE',  ( -42.34864001897649644, 13.69590355195401621, 59.50603524064797512 ) ) ;
#11289 = AXIS2_PLACEMENT_3D ( 'NONE', #15087, #25099, #4578 ) ;
#11290 = CARTESIAN_POINT ( 'NONE',  ( 47.41589883262609817, 23.11533908250407165, 47.25563437782572151 ) ) ;
#11291 = CARTESIAN_POINT ( 'NONE',  ( 21.09992658989239089, 24.34164230456639544, 47.04930799450051637 ) ) ;
#11292 = CARTESIAN_POINT ( 'NONE',  ( 21.09785597605719332, 15.24673779880127178, 47.04930799450051637 ) ) ;
#11293 = CIRCLE ( 'NONE', #29647, 1.899999999999999023 ) ;
#11294 = CARTESIAN_POINT ( 'NONE',  ( 45.28286642839709231, 27.78619643316631738, 47.97516931882780966 ) ) ;
#11295 = ORIENTED_EDGE ( 'NONE', *, *, #15240, .T. ) ;
#11296 = EDGE_LOOP ( 'NONE', ( #14898, #7884, #7875, #15270 ) ) ;
#11298 = CARTESIAN_POINT ( 'NONE',  ( 8.474859994195286461, 26.84143805560860940, 47.04930799450051637 ) ) ;
#11297 = CIRCLE ( 'NONE', #6074, 58.67217910650386870 ) ;
#11299 = VERTEX_POINT ( 'NONE', #24564 ) ;
#11300 = CARTESIAN_POINT ( 'NONE',  ( 49.01277441251810529, 29.50101108909405667, 48.06976730914941243 ) ) ;
#11301 = CARTESIAN_POINT ( 'NONE',  ( 21.09785597605720753, 14.86454579224779948, 47.04930799450052348 ) ) ;
#11302 = AXIS2_PLACEMENT_3D ( 'NONE', #12887, #32253, #22545 ) ;
#11303 = CARTESIAN_POINT ( 'NONE',  ( 21.09785597605719332, 25.56454579224779167, 23.54930799450051282 ) ) ;
#11304 = CARTESIAN_POINT ( 'NONE',  ( 21.09785597605719332, 30.56554579224779644, 70.54930799450050927 ) ) ;
#11305 = CARTESIAN_POINT ( 'NONE',  ( -43.72819403793993587, 1.315833819094413659, 34.64930799450052490 ) ) ;
#11306 = CARTESIAN_POINT ( 'NONE',  ( -40.70484894842233103, 8.274204744976163539, 59.54930799450050927 ) ) ;
#11307 = ORIENTED_EDGE ( 'NONE', *, *, #7272, .T. ) ;
#11308 = DIRECTION ( 'NONE',  ( 0.000000000000000000, 1.000000000000000000, -0.000000000000000000 ) ) ;
#11309 = FACE_BOUND ( 'NONE', #12704, .T. ) ;
#11310 = CARTESIAN_POINT ( 'NONE',  ( 21.09785597605719332, 44.06454579224779877, 46.04930799450054479 ) ) ;
#11311 = ADVANCED_FACE ( 'NONE', ( #32452 ), #12107, .F. ) ;
#11312 = AXIS2_PLACEMENT_3D ( 'NONE', #11654, #31032, #21155 ) ;
#11313 = CARTESIAN_POINT ( 'NONE',  ( 21.09785597605719332, 24.56454579224780232, 86.74871914086746472 ) ) ;
#11314 = DIRECTION ( 'NONE',  ( -1.101824276508909887E-16, 1.000000000000000000, -0.000000000000000000 ) ) ;
#11315 = EDGE_CURVE ( 'NONE', #27701, #21385, #9463, .T. ) ;
#11316 = VERTEX_POINT ( 'NONE', #9802 ) ;
#11317 = DIRECTION ( 'NONE',  ( -0.000000000000000000, 1.000000000000000000, -0.000000000000000000 ) ) ;
#11318 = EDGE_LOOP ( 'NONE', ( #14954, #5911, #22965, #9369 ) ) ;
#11319 = FACE_OUTER_BOUND ( 'NONE', #13195, .T. ) ;
#11320 = DIRECTION ( 'NONE',  ( -1.101824276508909887E-16, 1.000000000000000000, -0.000000000000000000 ) ) ;
#11321 = ORIENTED_EDGE ( 'NONE', *, *, #7381, .F. ) ;
#11322 = CIRCLE ( 'NONE', #20241, 12.27641737965283930 ) ;
#11323 = AXIS2_PLACEMENT_3D ( 'NONE', #22148, #32181, #9693 ) ;
#11324 = VERTEX_POINT ( 'NONE', #20284 ) ;
#11325 = CARTESIAN_POINT ( 'NONE',  ( 49.19517401419062708, 25.60920399681023341, 48.40991706654173754 ) ) ;
#11326 = LINE ( 'NONE', #13792, #2918 ) ;
#11327 = DIRECTION ( 'NONE',  ( -1.101824276508909887E-16, 1.000000000000000000, -0.000000000000000000 ) ) ;
#11328 = CIRCLE ( 'NONE', #29685, 12.36707279061065101 ) ;
#11329 = VERTEX_POINT ( 'NONE', #30314 ) ;
#11330 = CARTESIAN_POINT ( 'NONE',  ( 13.79206092585405230, -13.30632128221581212, 102.5023864623932894 ) ) ;
#11331 = DIRECTION ( 'NONE',  ( 0.000000000000000000, 0.000000000000000000, -1.000000000000000000 ) ) ;
#11332 = CARTESIAN_POINT ( 'NONE',  ( -40.04869510400517640, 6.988917179838707305, 39.04796398176969063 ) ) ;
#11333 = VERTEX_POINT ( 'NONE', #22097 ) ;
#11334 = DIRECTION ( 'NONE',  ( -0.8746197071393840838, 0.4848096202463581528, 0.000000000000000000 ) ) ;
#11335 = ORIENTED_EDGE ( 'NONE', *, *, #10545, .F. ) ;
#11336 = DIRECTION ( 'NONE',  ( -1.101824276508909887E-16, 1.000000000000000000, -0.000000000000000000 ) ) ;
#11337 = CARTESIAN_POINT ( 'NONE',  ( 47.09785597605719687, 15.77906836436399374, 47.04930799450078638 ) ) ;
#11338 = CARTESIAN_POINT ( 'NONE',  ( -39.58809650894544774, 2.596771453999702661, 47.04930799450051637 ) ) ;
#11339 = EDGE_LOOP ( 'NONE', ( #7214, #24769, #31421, #202 ) ) ;
#11340 = ORIENTED_EDGE ( 'NONE', *, *, #9459, .F. ) ;
#11341 = CARTESIAN_POINT ( 'NONE',  ( -38.21956372845817640, 5.305745712741808617, 52.04930799450051637 ) ) ;
#11342 = AXIS2_PLACEMENT_3D ( 'NONE', #3913, #31812, #1442 ) ;
#11343 = CARTESIAN_POINT ( 'NONE',  ( -40.02540636251514172, 2.839176264122877047, 57.04930799450051637 ) ) ;
#11344 = EDGE_CURVE ( 'NONE', #6305, #3624, #19962, .T. ) ;
#11345 = DIRECTION ( 'NONE',  ( -1.000000000000000000, -1.101824276508909887E-16, 0.000000000000000000 ) ) ;
#11346 = ADVANCED_FACE ( 'NONE', ( #32127 ), #19424, .T. ) ;
#11347 = ORIENTED_EDGE ( 'NONE', *, *, #25214, .F. ) ;
#11348 = CARTESIAN_POINT ( 'NONE',  ( 50.27680291267449775, -13.74047052604243468, -3.479232590077480758 ) ) ;
#11349 = ADVANCED_FACE ( 'NONE', ( #29663 ), #27184, .T. ) ;
#11350 = ORIENTED_EDGE ( 'NONE', *, *, #9121, .F. ) ;
#11351 = FACE_OUTER_BOUND ( 'NONE', #18688, .T. ) ;
#11352 = EDGE_CURVE ( 'NONE', #1319, #9226, #30981, .T. ) ;
#11353 = CARTESIAN_POINT ( 'NONE',  ( 50.10320668408830613, 27.70621246473837118, 47.20539118556276037 ) ) ;
#11354 = AXIS2_PLACEMENT_3D ( 'NONE', #30041, #27731, #11986 ) ;
#11355 = LINE ( 'NONE', #31380, #11208 ) ;
#11356 = EDGE_LOOP ( 'NONE', ( #30124, #21106, #27786, #20033, #29315, #5393 ) ) ;
#11357 = DIRECTION ( 'NONE',  ( 0.000000000000000000, 0.000000000000000000, 1.000000000000000000 ) ) ;
#11358 = FACE_OUTER_BOUND ( 'NONE', #18451, .T. ) ;
#11359 = CIRCLE ( 'NONE', #11342, 0.9999999999999731326 ) ;
#11360 = CARTESIAN_POINT ( 'NONE',  ( -63.90214402394282445, 9.925589859889734967, 54.04930799450052348 ) ) ;
#11361 = CARTESIAN_POINT ( 'NONE',  ( 46.00908685603034343, 29.03284706826092787, 44.91496614357595263 ) ) ;
#11362 = VERTEX_POINT ( 'NONE', #2415 ) ;
#11363 = FACE_OUTER_BOUND ( 'NONE', #29848, .T. ) ;
#11364 = CARTESIAN_POINT ( 'NONE',  ( 8.698509210239501854, 23.59164230456639544, 47.04930799450051637 ) ) ;
#11365 = EDGE_CURVE ( 'NONE', #63, #16672, #14195, .T. ) ;
#11366 = FACE_BOUND ( 'NONE', #9871, .T. ) ;
#11367 = AXIS2_PLACEMENT_3D ( 'NONE', #30226, #30383, #184 ) ;
#11368 = DIRECTION ( 'NONE',  ( -0.000000000000000000, 1.000000000000000000, -0.000000000000000000 ) ) ;
#11369 = CARTESIAN_POINT ( 'NONE',  ( -40.52064652407317169, 7.631814549704933448, 53.92245119299456491 ) ) ;
#11370 = DIRECTION ( 'NONE',  ( -1.000000000000000000, 0.000000000000000000, 0.000000000000000000 ) ) ;
#11371 = SHAPE_REPRESENTATION ( 'Lower Suspension', ( #8172 ), #27017 ) ;
#11372 = CARTESIAN_POINT ( 'NONE',  ( 48.23388202445966044, 28.22822092656774373, 49.27628909396054979 ) ) ;
#11373 = ORIENTED_EDGE ( 'NONE', *, *, #19838, .F. ) ;
#11374 = DIRECTION ( 'NONE',  ( 0.000000000000000000, -1.000000000000000000, 0.000000000000000000 ) ) ;
#11375 = CARTESIAN_POINT ( 'NONE',  ( 48.18662509608405031, 29.29624452788248234, 49.18364984542562013 ) ) ;
#11376 = CARTESIAN_POINT ( 'NONE',  ( -40.38150472626228549, 8.621068314769347651, 34.62702073480610210 ) ) ;
#11377 = CYLINDRICAL_SURFACE ( 'NONE', #9298, 12.36707279061065101 ) ;
#11378 = CYLINDRICAL_SURFACE ( 'NONE', #25232, 12.62506659569710266 ) ;
#11379 = EDGE_CURVE ( 'NONE', #14004, #30037, #1624, .T. ) ;
#11380 = ORIENTED_EDGE ( 'NONE', *, *, #15759, .F. ) ;
#11381 = DIRECTION ( 'NONE',  ( 0.4848096202463430537, 0.8746197071393926326, 9.920727850371700117E-18 ) ) ;
#11382 = CARTESIAN_POINT ( 'NONE',  ( -44.78514533282907450, -5.110533499441238803, 41.67803216526434795 ) ) ;
#11383 = DIRECTION ( 'NONE',  ( 0.000000000000000000, -1.000000000000000000, 0.000000000000000000 ) ) ;
#11384 = ORIENTED_EDGE ( 'NONE', *, *, #24383, .F. ) ;
#11385 = LINE ( 'NONE', #14183, #30926 ) ;
#11386 = EDGE_CURVE ( 'NONE', #23463, #2467, #12432, .T. ) ;
#11387 = CIRCLE ( 'NONE', #29736, 19.45967690998103805 ) ;
#11388 = FACE_OUTER_BOUND ( 'NONE', #14885, .T. ) ;
#11389 = CARTESIAN_POINT ( 'NONE',  ( 51.66808379569695830, 5.388785998227650254, 97.45038561958638468 ) ) ;
#11390 = ORIENTED_EDGE ( 'NONE', *, *, #22971, .F. ) ;
#11391 = FACE_OUTER_BOUND ( 'NONE', #6417, .T. ) ;
#11392 = EDGE_LOOP ( 'NONE', ( #403, #15879, #9787, #767 ) ) ;
#11393 = ORIENTED_EDGE ( 'NONE', *, *, #23233, .T. ) ;
#11394 = EDGE_CURVE ( 'NONE', #29823, #29193, #12632, .T. ) ;
#11395 = CARTESIAN_POINT ( 'NONE',  ( 21.09785597605719332, 30.36454579224779238, 47.04930799450051637 ) ) ;
#11396 = CARTESIAN_POINT ( 'NONE',  ( 21.09992658989238734, 31.47145308207317171, 47.04930799450051637 ) ) ;
#11397 = CARTESIAN_POINT ( 'NONE',  ( 9.016997203727585841, 15.24673779880127356, 46.73295957419995261 ) ) ;
#11398 = AXIS2_PLACEMENT_3D ( 'NONE', #13341, #13498, #3791 ) ;
#11399 = EDGE_CURVE ( 'NONE', #27481, #22149, #7410, .T. ) ;
#11400 = AXIS2_PLACEMENT_3D ( 'NONE', #20828, #3097, #18834 ) ;
#11401 = ORIENTED_EDGE ( 'NONE', *, *, #2599, .F. ) ;
#11402 = DIRECTION ( 'NONE',  ( -1.000000000000000000, 0.000000000000000000, 0.000000000000000000 ) ) ;
#11403 = ORIENTED_EDGE ( 'NONE', *, *, #13989, .F. ) ;
#11404 = DIRECTION ( 'NONE',  ( 0.000000000000000000, -1.000000000000000000, 0.000000000000000000 ) ) ;
#11405 = CARTESIAN_POINT ( 'NONE',  ( 21.09785597605719332, 13.74476430820393347, 102.0493079945005093 ) ) ;
#11406 = AXIS2_PLACEMENT_3D ( 'NONE', #968, #30408, #29929 ) ;
#11407 = FILL_AREA_STYLE ('',( #23882 ) ) ;
#11408 = VERTEX_POINT ( 'NONE', #12598 ) ;
#11409 = CARTESIAN_POINT ( 'NONE',  ( 47.09785597605719687, 25.56454579224779167, 47.04930799450078638 ) ) ;
#11410 = DIRECTION ( 'NONE',  ( -1.101824276508909887E-16, 1.000000000000000000, -0.000000000000000000 ) ) ;
#11411 = DIRECTION ( 'NONE',  ( 1.000000000000000000, 0.000000000000000000, 2.775557561562888984E-15 ) ) ;
#11412 = CARTESIAN_POINT ( 'NONE',  ( 45.47421713364555274, 22.88065857334294861, 45.99599230681428708 ) ) ;
#11413 = ORIENTED_EDGE ( 'NONE', *, *, #12398, .T. ) ;
#11414 = FACE_OUTER_BOUND ( 'NONE', #10766, .T. ) ;
#11415 = CARTESIAN_POINT ( 'NONE',  ( 21.09992658989238734, 31.97145308207317171, 47.04930799450051637 ) ) ;
#11416 = AXIS2_PLACEMENT_3D ( 'NONE', #21393, #3202, #1068 ) ;
#11417 = CARTESIAN_POINT ( 'NONE',  ( 21.09785597605719332, 12.74140866975414887, 47.04930799450051637 ) ) ;
#11418 = CARTESIAN_POINT ( 'NONE',  ( 21.09785597605719332, -6.659195188345857552, 47.04930799450051637 ) ) ;
#11419 = ORIENTED_EDGE ( 'NONE', *, *, #18724, .F. ) ;
#11420 = CARTESIAN_POINT ( 'NONE',  ( 21.09785597605719332, 45.06299627138002251, 47.04930799450051637 ) ) ;
#11421 = DIRECTION ( 'NONE',  ( 0.4848096202463506588, 0.8746197071393884137, 9.920727850371624621E-18 ) ) ;
#11422 = ORIENTED_EDGE ( 'NONE', *, *, #1149, .F. ) ;
#11423 = ADVANCED_FACE ( 'NONE', ( #109 ), #7669, .F. ) ;
#11424 = DIRECTION ( 'NONE',  ( -1.000000000000000000, 0.000000000000000000, 0.000000000000000000 ) ) ;
#11425 = DIRECTION ( 'NONE',  ( -1.000000000000000000, 0.000000000000000000, 0.000000000000000000 ) ) ;
#11426 = ORIENTED_EDGE ( 'NONE', *, *, #337, .T. ) ;
#11427 = ORIENTED_EDGE ( 'NONE', *, *, #12241, .F. ) ;
#11428 = AXIS2_PLACEMENT_3D ( 'NONE', #31337, #15855, #6158 ) ;
#11429 = VECTOR ( 'NONE', #32283, 1000.000000000000000 ) ;
#11430 = ORIENTED_EDGE ( 'NONE', *, *, #6115, .T. ) ;
#11431 = CIRCLE ( 'NONE', #29786, 0.5000000000000004441 ) ;
#11432 = AXIS2_PLACEMENT_3D ( 'NONE', #25319, #31330, #11462 ) ;
#11433 = EDGE_CURVE ( 'NONE', #28828, #23509, #23558, .T. ) ;
#11434 = EDGE_CURVE ( 'NONE', #19635, #19572, #30467, .T. ) ;
#11435 = AXIS2_PLACEMENT_3D ( 'NONE', #4623, #26461, #26619 ) ;
#11436 = DIRECTION ( 'NONE',  ( 0.000000000000000000, 0.000000000000000000, 1.000000000000000000 ) ) ;
#11437 = EDGE_CURVE ( 'NONE', #22710, #11279, #18145, .T. ) ;
#11438 = ORIENTED_EDGE ( 'NONE', *, *, #31546, .T. ) ;
#11439 = CARTESIAN_POINT ( 'NONE',  ( 8.732853799281734553, 38.56284415653841791, 47.04930799450051637 ) ) ;
#11440 = EDGE_CURVE ( 'NONE', #3369, #28743, #18304, .T. ) ;
#11441 = LINE ( 'NONE', #7006, #8850 ) ;
#11442 = CARTESIAN_POINT ( 'NONE',  ( 21.09785597605720753, -5.098646251524523443, 47.04930799450052348 ) ) ;
#11443 = DIRECTION ( 'NONE',  ( 0.2756373558169974980, -0.9612616959383193382, 9.694974607321218218E-33 ) ) ;
#11444 = CARTESIAN_POINT ( 'NONE',  ( 48.16694854572211426, 26.56119643316631951, 49.14507740233662503 ) ) ;
#11445 = ORIENTED_EDGE ( 'NONE', *, *, #1580, .F. ) ;
#11446 = ORIENTED_EDGE ( 'NONE', *, *, #19881, .T. ) ;
#11447 = CARTESIAN_POINT ( 'NONE',  ( -12.16553382968505481, -0.1676091211930501867, -5.936183209767050606 ) ) ;
#11448 = AXIS2_PLACEMENT_3D ( 'NONE', #29287, #1876, #16161 ) ;
#11449 = VERTEX_POINT ( 'NONE', #18470 ) ;
#11450 = CARTESIAN_POINT ( 'NONE',  ( 33.72499318558949710, 25.34184655352419213, 47.04930799450051637 ) ) ;
#11451 = AXIS2_PLACEMENT_3D ( 'NONE', #13311, #11320, #13947 ) ;
#11452 = CARTESIAN_POINT ( 'NONE',  ( -40.56083369918798098, 7.405617721157757849, 38.79123571389602887 ) ) ;
#11453 = CARTESIAN_POINT ( 'NONE',  ( -40.69114442294520728, 6.794816359673525596, 39.38644499583401881 ) ) ;
#11454 = DIRECTION ( 'NONE',  ( -1.000000000000000000, 0.000000000000000000, 0.000000000000000000 ) ) ;
#11455 = CIRCLE ( 'NONE', #1493, 1.300000000000002487 ) ;
#11456 = CARTESIAN_POINT ( 'NONE',  ( 48.46535932150934656, 25.48954579807171328, 49.73005965046827015 ) ) ;
#11457 = CIRCLE ( 'NONE', #29818, 12.27641737965287660 ) ;
#11458 = DIRECTION ( 'NONE',  ( 0.000000000000000000, 0.000000000000000000, -1.000000000000000000 ) ) ;
#11459 = LINE ( 'NONE', #28224, #3312 ) ;
#11460 = ORIENTED_EDGE ( 'NONE', *, *, #2072, .F. ) ;
#11461 = DIRECTION ( 'NONE',  ( -1.000000000000000000, 0.000000000000000000, 0.000000000000000000 ) ) ;
#11462 = DIRECTION ( 'NONE',  ( -1.000000000000000000, 0.000000000000000000, 0.000000000000000000 ) ) ;
#11463 = CARTESIAN_POINT ( 'NONE',  ( 47.09785597605719687, 29.16454579224780019, 47.04930799450078638 ) ) ;
#11464 = AXIS2_PLACEMENT_3D ( 'NONE', #14501, #32225, #19571 ) ;
#11465 = FACE_OUTER_BOUND ( 'NONE', #5480, .T. ) ;
#11466 = FACE_OUTER_BOUND ( 'NONE', #23941, .T. ) ;
#11467 = ORIENTED_EDGE ( 'NONE', *, *, #25356, .T. ) ;
#11468 = CARTESIAN_POINT ( 'NONE',  ( 21.09992658989239089, 26.09143805560860940, 47.04930799450051637 ) ) ;
#11469 = EDGE_LOOP ( 'NONE', ( #22524, #29133, #24942, #15017, #11422, #3381 ) ) ;
#11470 = CARTESIAN_POINT ( 'NONE',  ( 8.698509210239542710, 27.59164230456639544, 47.04930799450051637 ) ) ;
#11471 = DIRECTION ( 'NONE',  ( -1.000000000000000000, 0.000000000000000000, 0.000000000000000000 ) ) ;
#11472 = ORIENTED_EDGE ( 'NONE', *, *, #6435, .F. ) ;
#11473 = EDGE_CURVE ( 'NONE', #4508, #7574, #29788, .T. ) ;
#11474 = AXIS2_PLACEMENT_3D ( 'NONE', #30350, #5239, #25418 ) ;
#11475 = CIRCLE ( 'NONE', #20917, 0.1250000000000001110 ) ;
#11476 = ADVANCED_FACE ( 'NONE', ( #10937 ), #11105, .T. ) ;
#11477 = ORIENTED_EDGE ( 'NONE', *, *, #22194, .T. ) ;
#11478 = CARTESIAN_POINT ( 'NONE',  ( 65.59785597605720397, 13.86454579224779948, 47.04930799450051637 ) ) ;
#11479 = PLANE ( 'NONE',  #24421 ) ;
#11480 = DIRECTION ( 'NONE',  ( -1.224646799147353207E-16, -1.349345573449484691E-32, 1.000000000000000000 ) ) ;
#11481 = EDGE_CURVE ( 'NONE', #27575, #17665, #10000, .T. ) ;
#11482 = AXIS2_PLACEMENT_3D ( 'NONE', #5742, #25117, #12976 ) ;
#11483 = EDGE_LOOP ( 'NONE', ( #4523, #28764, #25892, #11124 ) ) ;
#11484 = DIRECTION ( 'NONE',  ( -1.101824276508909887E-16, 1.000000000000000000, -0.000000000000000000 ) ) ;
#11485 = AXIS2_PLACEMENT_3D ( 'NONE', #9373, #24795, #14141 ) ;
#11486 = DIRECTION ( 'NONE',  ( -1.000000000000000000, -1.101824276508909887E-16, 0.000000000000000000 ) ) ;
#11487 = CARTESIAN_POINT ( 'NONE',  ( 73.38268324366261197, 4.638969541771025717, 16.21882525954990228 ) ) ;
#11488 = ORIENTED_EDGE ( 'NONE', *, *, #5988, .T. ) ;
#11489 = DIRECTION ( 'NONE',  ( -1.101824276508909887E-16, 1.000000000000000000, -0.000000000000000000 ) ) ;
#11490 = VERTEX_POINT ( 'NONE', #761 ) ;
#11491 = FACE_BOUND ( 'NONE', #7155, .T. ) ;
#11492 = CARTESIAN_POINT ( 'NONE',  ( -41.23493495844309109, 10.15322714841875040, 37.04930799450052348 ) ) ;
#11493 = DIRECTION ( 'NONE',  ( -1.000000000000000000, 0.000000000000000000, 0.000000000000000000 ) ) ;
#11494 = DIRECTION ( 'NONE',  ( 0.000000000000000000, 0.000000000000000000, 1.000000000000000000 ) ) ;
#11495 = EDGE_LOOP ( 'NONE', ( #6735, #30385, #6253, #17592 ) ) ;
#11496 = ORIENTED_EDGE ( 'NONE', *, *, #31432, .F. ) ;
#11497 = CARTESIAN_POINT ( 'NONE',  ( 24.75079866426201392, -13.30632128221581034, -8.763545028782029789 ) ) ;
#11498 = VECTOR ( 'NONE', #30791, 1000.000000000000000 ) ;
#11499 = DIRECTION ( 'NONE',  ( -1.101824276508909887E-16, 1.000000000000000000, -0.000000000000000000 ) ) ;
#11500 = AXIS2_PLACEMENT_3D ( 'NONE', #10916, #10433, #25365 ) ;
#11501 = DIRECTION ( 'NONE',  ( 1.234978253042719660E-16, -1.000000000000000000, -1.170965406187439618E-31 ) ) ;
#11502 = ORIENTED_EDGE ( 'NONE', *, *, #19280, .T. ) ;
#11503 = CARTESIAN_POINT ( 'NONE',  ( -12.61173037625193061, -3.171899563477257100, -8.558298061174587801 ) ) ;
#11504 = DIRECTION ( 'NONE',  ( -0.8746197071393810862, 0.4848096202463637039, 8.676864087101942305E-18 ) ) ;
#11505 = VERTEX_POINT ( 'NONE', #30482 ) ;
#11506 = FACE_BOUND ( 'NONE', #18956, .T. ) ;
#11507 = CARTESIAN_POINT ( 'NONE',  ( 48.73570333863616355, 29.92287913140503619, 44.52463952959527660 ) ) ;
#11508 = CIRCLE ( 'NONE', #27222, 0.1250000000000001110 ) ;
#11509 = AXIS2_PLACEMENT_3D ( 'NONE', #10917, #7976, #3186 ) ;
#11510 = DIRECTION ( 'NONE',  ( -1.101824276508909887E-16, 1.000000000000000000, -0.000000000000000000 ) ) ;
#11511 = AXIS2_PLACEMENT_3D ( 'NONE', #25407, #295, #20477 ) ;
#11512 = CIRCLE ( 'NONE', #8378, 54.49999999999997868 ) ;
#11513 = ORIENTED_EDGE ( 'NONE', *, *, #31859, .T. ) ;
#11514 = CARTESIAN_POINT ( 'NONE',  ( 21.09992658989239089, 28.34164230456639544, 47.04930799450051637 ) ) ;
#11515 = FACE_OUTER_BOUND ( 'NONE', #30343, .T. ) ;
#11516 = CARTESIAN_POINT ( 'NONE',  ( -40.68422973805265030, 6.807290781432338456, 34.77612644482307758 ) ) ;
#11517 = CARTESIAN_POINT ( 'NONE',  ( 47.20547626766765603, 29.67451373492759004, 44.97710074790751378 ) ) ;
#11518 = AXIS2_PLACEMENT_3D ( 'NONE', #14855, #20092, #233 ) ;
#11519 = AXIS2_PLACEMENT_3D ( 'NONE', #23360, #23683, #5969 ) ;
#11520 = ADVANCED_FACE ( 'NONE', ( #17827 ), #25864, .F. ) ;
#11521 = ORIENTED_EDGE ( 'NONE', *, *, #23468, .T. ) ;
#11522 = EDGE_CURVE ( 'NONE', #10653, #11408, #28497, .T. ) ;
#11523 = EDGE_CURVE ( 'NONE', #14337, #8103, #22048, .T. ) ;
#11524 = EDGE_CURVE ( 'NONE', #22190, #3892, #26018, .T. ) ;
#11525 = CARTESIAN_POINT ( 'NONE',  ( -8.402144023942796025, 14.86454579224779948, 47.04930799450052348 ) ) ;
#11526 = CARTESIAN_POINT ( 'NONE',  ( 21.09992658989238734, 38.56284415653841791, 47.04930799450051637 ) ) ;
#11527 = EDGE_CURVE ( 'NONE', #14804, #8738, #5842, .T. ) ;
#11528 = CARTESIAN_POINT ( 'NONE',  ( 21.09992658989239089, 29.34143805560861296, 47.04930799450051637 ) ) ;
#11529 = VECTOR ( 'NONE', #24462, 1000.000000000000114 ) ;
#11530 = DIRECTION ( 'NONE',  ( 0.4848096202463424986, 0.8746197071393928546, -2.220446049250312834E-16 ) ) ;
#11531 = DIRECTION ( 'NONE',  ( -0.000000000000000000, -1.000000000000000000, 0.000000000000000000 ) ) ;
#11532 = DIRECTION ( 'NONE',  ( -0.000000000000000000, -1.000000000000000000, 0.000000000000000000 ) ) ;
#11533 = DIRECTION ( 'NONE',  ( -0.1949050434465282866, 0.6797146636928672603, -0.7071067811865470176 ) ) ;
#11534 = AXIS2_PLACEMENT_3D ( 'NONE', #28767, #30760, #18580 ) ;
#11535 = CARTESIAN_POINT ( 'NONE',  ( 21.09992658989238734, 31.21183152705961206, 47.04930799450051637 ) ) ;
#11536 = AXIS2_PLACEMENT_3D ( 'NONE', #19642, #17518, #27534 ) ;
#11537 = ORIENTED_EDGE ( 'NONE', *, *, #5669, .T. ) ;
#11538 = AXIS2_PLACEMENT_3D ( 'NONE', #1488, #13821, #16583 ) ;
#11539 = CARTESIAN_POINT ( 'NONE',  ( 45.41164638504195494, 22.93807716476589675, 46.96173444154113241 ) ) ;
#11540 = CARTESIAN_POINT ( 'NONE',  ( 45.24946171279598417, 26.32124452788248803, 47.99220971130008451 ) ) ;
#11541 = FACE_OUTER_BOUND ( 'NONE', #7031, .T. ) ;
#11542 = CARTESIAN_POINT ( 'NONE',  ( 8.732853799281729223, 30.72145308207317882, 47.04930799450051637 ) ) ;
#11543 = CARTESIAN_POINT ( 'NONE',  ( -6.402144023942790696, 14.86454579224779948, 47.04930799450052348 ) ) ;
#11544 = ORIENTED_EDGE ( 'NONE', *, *, #3963, .F. ) ;
#11545 = DIRECTION ( 'NONE',  ( 0.9612616959383221138, 0.2756373558169876170, 0.000000000000000000 ) ) ;
#11546 = CARTESIAN_POINT ( 'NONE',  ( -40.19913497620438392, 7.013551051776435230, 39.22537497467693157 ) ) ;
#11547 = CYLINDRICAL_SURFACE ( 'NONE', #25876, 12.36707279061065101 ) ;
#11548 = CIRCLE ( 'NONE', #27644, 36.51080762834750715 ) ;
#11549 = EDGE_LOOP ( 'NONE', ( #3417, #16301, #19567, #14155, #26636, #25473, #14173, #4535, #29485, #23469 ) ) ;
#11550 = DIRECTION ( 'NONE',  ( 0.1949050434465275650, -0.6797146636928697028, 0.7071067811865449082 ) ) ;
#11551 = CARTESIAN_POINT ( 'NONE',  ( 21.09785597605720042, -16.03545420775219910, -17.45069200549948718 ) ) ;
#11552 = AXIS2_PLACEMENT_3D ( 'NONE', #11864, #23687, #28608 ) ;
#11553 = DIRECTION ( 'NONE',  ( -4.252959262497663712E-16, 2.543118322573790544E-15, 1.000000000000000000 ) ) ;
#11554 = DIRECTION ( 'NONE',  ( -0.000000000000000000, -1.000000000000000000, 0.000000000000000000 ) ) ;
#11555 = ORIENTED_EDGE ( 'NONE', *, *, #30698, .T. ) ;
#11556 = DIRECTION ( 'NONE',  ( 5.368498217537939937E-17, 0.8987940462991685919, -0.4383711467890740732 ) ) ;
#11557 = ORIENTED_EDGE ( 'NONE', *, *, #2306, .F. ) ;
#11558 = CIRCLE ( 'NONE', #14192, 0.09999999999999753530 ) ;
#11559 = AXIS2_PLACEMENT_3D ( 'NONE', #12916, #17982, #18137 ) ;
#11560 = VERTEX_POINT ( 'NONE', #25381 ) ;
#11561 = TOROIDAL_SURFACE ( 'NONE', #15761, 1.142135311067127068, 0.1000000000000000056 ) ;
#11562 = AXIS2_PLACEMENT_3D ( 'NONE', #28708, #3597, #21306 ) ;
#11563 = MECHANICAL_DESIGN_GEOMETRIC_PRESENTATION_REPRESENTATION (  '', ( #13150 ), #6858 ) ;
#11564 = EDGE_CURVE ( 'NONE', #30197, #20645, #27311, .T. ) ;
#11565 = EDGE_CURVE ( 'NONE', #12497, #30197, #5296, .T. ) ;
#11566 = EDGE_CURVE ( 'NONE', #23085, #7282, #23630, .T. ) ;
#11567 =( BOUNDED_SURFACE ( )  B_SPLINE_SURFACE ( 3, 2, ( 
 ( #26359, #28827, #18484 ),
 ( #16343, #31140, #13739 ),
 ( #614, #3877, #26195 ),
 ( #23736, #23419, #20948 ),
 ( #30979, #11272, #11119 ),
 ( #6026, #20792, #16027 ),
 ( #1244, #21103, #21264 ),
 ( #18320, #23096, #8794 ),
 ( #18792, #8489, #31294 ),
 ( #10641, #20634, #30656 ) ),
 .UNSPECIFIED., .F., .F., .F. ) 
 B_SPLINE_SURFACE_WITH_KNOTS ( ( 4, 2, 2, 2, 4 ),
 ( 3, 3 ),
 ( -2.222614453595284090E-18, 0.0003347409949957051148, 0.0006694819899914123979, 0.001004222984987119573, 0.001338963979982826964 ),
 ( 0.000000000000000000, 1.000000000000000000 ),
 .UNSPECIFIED. ) 
 GEOMETRIC_REPRESENTATION_ITEM ( )  RATIONAL_B_SPLINE_SURFACE ( (
 ( 1.000000000000000000, 0.7071067811865465735, 1.000000000000000000),
 ( 1.000000000000000000, 0.7102524952755833176, 1.000000000000000000),
 ( 1.000000000000000000, 0.7282169120226342773, 1.000000000000000000),
 ( 1.000000000000000000, 0.7754022836010627806, 1.000000000000000000),
 ( 1.000000000000000000, 0.8043059223109642053, 1.000000000000000000),
 ( 1.000000000000000000, 0.8571167854607034675, 1.000000000000000000),
 ( 1.000000000000000000, 0.8816198077927471788, 1.000000000000000000),
 ( 1.000000000000000000, 0.9175117844836407910, 1.000000000000000000),
 ( 1.000000000000000000, 0.9295466150070802458, 1.000000000000000000),
 ( 1.000000000000000000, 0.9308844615756591834, 1.000000000000000000) ) ) 
 REPRESENTATION_ITEM ( '' )  SURFACE ( )  );
#11568 = DIRECTION ( 'NONE',  ( 0.000000000000000000, 0.000000000000000000, -1.000000000000000000 ) ) ;
#11569 = DIRECTION ( 'NONE',  ( -1.000000000000000000, 0.000000000000000000, 0.000000000000000000 ) ) ;
#11570 = CARTESIAN_POINT ( 'NONE',  ( 81.63175399755476747, -5.935454207809698346, 78.02743327247107175 ) ) ;
#11571 = EDGE_CURVE ( 'NONE', #12727, #5195, #4778, .T. ) ;
#11572 = EDGE_CURVE ( 'NONE', #28878, #19617, #22573, .T. ) ;
#11573 = AXIS2_PLACEMENT_3D ( 'NONE', #14900, #22425, #20135 ) ;
#11574 = EDGE_LOOP ( 'NONE', ( #21870, #31828, #30935, #9029 ) ) ;
#11575 = CARTESIAN_POINT ( 'NONE',  ( 21.09785597605720753, -5.098646251524523443, 47.04930799450052348 ) ) ;
#11576 = ORIENTED_EDGE ( 'NONE', *, *, #17408, .T. ) ;
#11577 = DIRECTION ( 'NONE',  ( -0.4848096202463430537, -0.8746197071393926326, -9.920727850371700117E-18 ) ) ;
#11578 = ORIENTED_EDGE ( 'NONE', *, *, #19556, .F. ) ;
#11579 = DIRECTION ( 'NONE',  ( 0.8746197071393926326, -0.4848096202463430537, -8.676864087101709653E-18 ) ) ;
#11580 = CARTESIAN_POINT ( 'NONE',  ( 21.09992658989239089, 25.84164230456639899, 47.04930799450051637 ) ) ;
#11581 = LINE ( 'NONE', #22348, #18611 ) ;
#11582 = FACE_OUTER_BOUND ( 'NONE', #32079, .T. ) ;
#11583 = ORIENTED_EDGE ( 'NONE', *, *, #9617, .T. ) ;
#11584 = DIRECTION ( 'NONE',  ( 0.000000000000000000, 1.000000000000000000, 0.000000000000000000 ) ) ;
#11585 = DIRECTION ( 'NONE',  ( -1.101824276508909887E-16, 1.000000000000000000, -0.000000000000000000 ) ) ;
#11586 = DIRECTION ( 'NONE',  ( -1.000000000000000000, 0.000000000000000000, 0.000000000000000000 ) ) ;
#11587 = DIRECTION ( 'NONE',  ( -0.000000000000000000, -1.000000000000000000, -0.000000000000000000 ) ) ;
#11588 = DIRECTION ( 'NONE',  ( -1.000000000000000000, -1.101824276508910010E-16, 0.000000000000000000 ) ) ;
#11589 = VERTEX_POINT ( 'NONE', #1882 ) ;
#11590 = TOROIDAL_SURFACE ( 'NONE', #3191, 56.00000000000000000, 1.700000000000000178 ) ;
#11591 = DIRECTION ( 'NONE',  ( 0.000000000000000000, 0.000000000000000000, -1.000000000000000000 ) ) ;
#11592 = LINE ( 'NONE', #31615, #32186 ) ;
#11593 = EDGE_LOOP ( 'NONE', ( #3869, #15169, #9580, #2677 ) ) ;
#11594 = AXIS2_PLACEMENT_3D ( 'NONE', #28813, #31762, #18625 ) ;
#11595 = CARTESIAN_POINT ( 'NONE',  ( -44.25477285282614304, -5.710200047292144809, 40.98160301053449928 ) ) ;
#11596 = AXIS2_PLACEMENT_3D ( 'NONE', #2543, #27162, #24874 ) ;
#11597 = CARTESIAN_POINT ( 'NONE',  ( 21.09992658989239089, 23.97145308207319658, 47.04930799450051637 ) ) ;
#11598 = ORIENTED_EDGE ( 'NONE', *, *, #13898, .F. ) ;
#11599 = ORIENTED_EDGE ( 'NONE', *, *, #20529, .F. ) ;
#11600 = EDGE_CURVE ( 'NONE', #13675, #3287, #7922, .T. ) ;
#11601 = VECTOR ( 'NONE', #2003, 1000.000000000000000 ) ;
#11602 = EDGE_CURVE ( 'NONE', #12393, #10938, #4183, .T. ) ;
#11603 = ORIENTED_EDGE ( 'NONE', *, *, #15890, .T. ) ;
#11604 = AXIS2_PLACEMENT_3D ( 'NONE', #14700, #7478, #17137 ) ;
#11605 = CIRCLE ( 'NONE', #26817, 12.36707279061065101 ) ;
#11606 = CARTESIAN_POINT ( 'NONE',  ( -42.73182147790732444, -0.8057266458565844891, 32.04930799450052348 ) ) ;
#11607 = EDGE_CURVE ( 'NONE', #27622, #607, #11058, .T. ) ;
#11608 = CLOSED_SHELL ( 'NONE', ( #22470, #24065, #25471, #14041, #25856, #25389, #10174, #20191, #23709, #29913, #21667, #4221, #11423, #21920, #819, #32093, #27636, #12047, #15801, #29617, #1185, #29807, #19238, #1839, #17742, #31830, #13753, #25415, #3200, #25609, #21354, #3400, #20803, #17693, #7720, #12239, #28984, #19892, #9557, #25458, #29649, #20970, #16610, #11757, #28206, #12640, #13401, #14351, #483, #15081, #24906, #3844, #24649, #20601, #9655, #16260, #16432, #16779, #18293 ) ) ;
#11609 = ORIENTED_EDGE ( 'NONE', *, *, #22476, .T. ) ;
#11610 = DIRECTION ( 'NONE',  ( -1.101824276508909887E-16, 1.000000000000000000, -0.000000000000000000 ) ) ;
#11611 = FACE_OUTER_BOUND ( 'NONE', #25190, .T. ) ;
#11612 = CARTESIAN_POINT ( 'NONE',  ( 47.09785597605719687, 25.56454579224779877, 47.04930799450042400 ) ) ;
#11613 = DIRECTION ( 'NONE',  ( 0.000000000000000000, 0.000000000000000000, -1.000000000000000000 ) ) ;
#11614 = CARTESIAN_POINT ( 'NONE',  ( 48.16694854572211426, 27.96119643316631453, 49.14507740233662503 ) ) ;
#11615 = ORIENTED_EDGE ( 'NONE', *, *, #24557, .F. ) ;
#11616 = CARTESIAN_POINT ( 'NONE',  ( 21.09785597605720753, 15.70210863493540288, 47.04930799450052348 ) ) ;
#11617 = ORIENTED_EDGE ( 'NONE', *, *, #32257, .T. ) ;
#11618 = CARTESIAN_POINT ( 'NONE',  ( 33.46699938050303302, 38.56284415653841791, 47.04930799450051637 ) ) ;
#11619 = CIRCLE ( 'NONE', #16316, 0.1249999999999983763 ) ;
#11620 = ORIENTED_EDGE ( 'NONE', *, *, #6304, .T. ) ;
#11621 = CARTESIAN_POINT ( 'NONE',  ( -36.45222641229887017, 9.925589859889722533, 42.04930799450051637 ) ) ;
#11622 = DIRECTION ( 'NONE',  ( -1.000000000000000000, 0.000000000000000000, 0.000000000000000000 ) ) ;
#11623 = CARTESIAN_POINT ( 'NONE',  ( -40.68293647075795860, 6.808040729367310639, 39.52524033956975558 ) ) ;
#11624 = CYLINDRICAL_SURFACE ( 'NONE', #1105, 10.00000000000000178 ) ;
#11625 = DIRECTION ( 'NONE',  ( -1.188208965918165239E-16, -1.880121038077813132E-16, -1.000000000000000000 ) ) ;
#11626 = CARTESIAN_POINT ( 'NONE',  ( 44.91142894931555674, 25.89787913140504472, 45.63089057098605394 ) ) ;
#11627 = DIRECTION ( 'NONE',  ( -1.188208965918165239E-16, -1.880121038077813132E-16, -1.000000000000000000 ) ) ;
#11628 = DIRECTION ( 'NONE',  ( 3.534951791954965799E-15, 3.759183808608825436E-15, -1.000000000000000000 ) ) ;
#11629 = EDGE_CURVE ( 'NONE', #16953, #27014, #1391, .T. ) ;
#11630 = ORIENTED_EDGE ( 'NONE', *, *, #32133, .T. ) ;
#11631 = DIRECTION ( 'NONE',  ( -0.3935310072385434510, 0.5000000000000004441, -0.7714488617801033010 ) ) ;
#11632 = DIRECTION ( 'NONE',  ( -0.8746197071393925215, 0.4848096202463429982, 1.121857559391816958E-19 ) ) ;
#11633 = DIRECTION ( 'NONE',  ( -0.000000000000000000, -1.000000000000000000, -0.000000000000000000 ) ) ;
#11634 = EDGE_CURVE ( 'NONE', #21015, #16985, #13172, .T. ) ;
#11635 = AXIS2_PLACEMENT_3D ( 'NONE', #30203, #14941, #17712 ) ;
#11636 = CARTESIAN_POINT ( 'NONE',  ( 48.48814272641119061, 22.95310733321322161, 46.17903408117996378 ) ) ;
#11637 = CARTESIAN_POINT ( 'NONE',  ( -43.86882709718853590, -0.1754741395363378920, 61.94930799450052206 ) ) ;
#11638 = AXIS2_PLACEMENT_3D ( 'NONE', #9303, #19300, #16846 ) ;
#11639 = ORIENTED_EDGE ( 'NONE', *, *, #14026, .F. ) ;
#11640 = CARTESIAN_POINT ( 'NONE',  ( -42.38687957179150345, 4.148162238788003719, 57.04930799450051637 ) ) ;
#11641 = ADVANCED_BREP_SHAPE_REPRESENTATION ( '', ( #1464, #8172 ), #19670 ) ;
#11642 = VECTOR ( 'NONE', #27620, 1000.000000000000000 ) ;
#11643 = ORIENTED_EDGE ( 'NONE', *, *, #28684, .T. ) ;
#11644 = DIRECTION ( 'NONE',  ( -1.224646799147353207E-16, 0.000000000000000000, -1.000000000000000000 ) ) ;
#11645 = FACE_OUTER_BOUND ( 'NONE', #22262, .T. ) ;
#11646 = EDGE_CURVE ( 'NONE', #21033, #31848, #26344, .T. ) ;
#11647 = EDGE_CURVE ( 'NONE', #2889, #6349, #15245, .T. ) ;
#11648 = EDGE_CURVE ( 'NONE', #21311, #24691, #21572, .T. ) ;
#11649 = ORIENTED_EDGE ( 'NONE', *, *, #21558, .F. ) ;
#11650 = CIRCLE ( 'NONE', #24740, 0.1000000000000014905 ) ;
#11651 = ORIENTED_EDGE ( 'NONE', *, *, #4813, .F. ) ;
#11652 = DIRECTION ( 'NONE',  ( -1.000000000000000000, 0.000000000000000000, 0.000000000000000000 ) ) ;
#11653 = EDGE_CURVE ( 'NONE', #16169, #13013, #3697, .T. ) ;
#11654 = CARTESIAN_POINT ( 'NONE',  ( 21.09785597605719332, 25.56454579224779877, 47.04930799450051637 ) ) ;
#11655 = CARTESIAN_POINT ( 'NONE',  ( 45.96182992765471909, 28.57822092656774160, 44.82232689504102296 ) ) ;
#11656 = VECTOR ( 'NONE', #22462, 1000.000000000000114 ) ;
#11657 = EDGE_LOOP ( 'NONE', ( #18645, #20261, #3171, #3305, #11101 ) ) ;
#11658 = TOROIDAL_SURFACE ( 'NONE', #2761, 12.61792373059897265, 0.1249999999999971551 ) ;
#11659 = DIRECTION ( 'NONE',  ( -0.6184495258776564475, 0.3428121700606708844, 0.7071067811865443531 ) ) ;
#11660 = CARTESIAN_POINT ( 'NONE',  ( 74.77803812839373165, 0.4256545730734913047, 14.01035497445585243 ) ) ;
#11661 = ORIENTED_EDGE ( 'NONE', *, *, #10010, .T. ) ;
#11662 = CARTESIAN_POINT ( 'NONE',  ( 47.07252097517607581, 23.24793988701932079, 48.01698397347956870 ) ) ;
#11663 = ORIENTED_EDGE ( 'NONE', *, *, #3614, .T. ) ;
#11664 = PLANE ( 'NONE',  #5515 ) ;
#11665 = DIRECTION ( 'NONE',  ( -1.000000000000000000, 0.000000000000000000, 0.000000000000000000 ) ) ;
#11666 = LINE ( 'NONE', #6732, #23094 ) ;
#11667 = ADVANCED_FACE ( 'NONE', ( #19266 ), #6342, .F. ) ;
#11668 = CARTESIAN_POINT ( 'NONE',  ( -44.81001360148904666, -3.469446951953614189E-15, 11.66857518453430842 ) ) ;
#11669 = VERTEX_POINT ( 'NONE', #31279 ) ;
#11670 = ORIENTED_EDGE ( 'NONE', *, *, #9907, .T. ) ;
#11671 = DIRECTION ( 'NONE',  ( -0.000000000000000000, -1.000000000000000000, 0.000000000000000000 ) ) ;
#11672 = DIRECTION ( 'NONE',  ( -0.000000000000000000, -1.000000000000000000, -0.000000000000000000 ) ) ;
#11673 = EDGE_CURVE ( 'NONE', #3218, #3824, #5312, .T. ) ;
#11674 = CARTESIAN_POINT ( 'NONE',  ( -39.85048242108726413, 2.742214340073605872, 47.04930799450051637 ) ) ;
#11675 = AXIS2_PLACEMENT_3D ( 'NONE', #25783, #679, #5933 ) ;
#11676 = VERTEX_POINT ( 'NONE', #23722 ) ;
#11677 = DIRECTION ( 'NONE',  ( 0.000000000000000000, -0.000000000000000000, 1.000000000000000000 ) ) ;
#11678 = LINE ( 'NONE', #16265, #24082 ) ;
#11679 = AXIS2_PLACEMENT_3D ( 'NONE', #17053, #2127, #27067 ) ;
#11680 = ORIENTED_EDGE ( 'NONE', *, *, #19172, .T. ) ;
#11681 = DIRECTION ( 'NONE',  ( -0.000000000000000000, -1.000000000000000000, -0.000000000000000000 ) ) ;
#11682 = CARTESIAN_POINT ( 'NONE',  ( 44.91142894931555674, 26.59787913140504401, 45.63089057098605394 ) ) ;
#11683 = ADVANCED_FACE ( 'NONE', ( #16643 ), #28887, .T. ) ;
#11684 = AXIS2_PLACEMENT_3D ( 'NONE', #32132, #19148, #29510 ) ;
#11685 = EDGE_CURVE ( 'NONE', #19299, #22139, #580, .T. ) ;
#11686 = CIRCLE ( 'NONE', #26365, 12.62506659569710266 ) ;
#11687 = ORIENTED_EDGE ( 'NONE', *, *, #2663, .F. ) ;
#11688 = MANIFOLD_SOLID_BREP ( 'Stock-MAT-060-1', #3216 ) ;
#11689 = CARTESIAN_POINT ( 'NONE',  ( 45.04270468994605636, 22.74928388133296764, 48.43919039919626357 ) ) ;
#11690 = DIRECTION ( 'NONE',  ( 0.000000000000000000, 0.000000000000000000, -1.000000000000000000 ) ) ;
#11691 = DIRECTION ( 'NONE',  ( 0.000000000000000000, 0.000000000000000000, -1.000000000000000000 ) ) ;
#11692 = CARTESIAN_POINT ( 'NONE',  ( 45.24946171279598417, 27.80784706826093000, 47.99220971130007030 ) ) ;
#11693 = ORIENTED_EDGE ( 'NONE', *, *, #26223, .F. ) ;
#11694 = AXIS2_PLACEMENT_3D ( 'NONE', #28220, #13453, #25587 ) ;
#11695 = CARTESIAN_POINT ( 'NONE',  ( -40.99628586177130529, 8.927770518203464789, 57.04930799450051637 ) ) ;
#11697 = DIRECTION ( 'NONE',  ( 0.9612616959383205595, 0.2756373558169931681, -1.660411357259282445E-16 ) ) ;
#11696 = AXIS2_PLACEMENT_3D ( 'NONE', #23916, #11774, #4382 ) ;
#11698 = CARTESIAN_POINT ( 'NONE',  ( 54.83501011029174066, -2.946992577399113244, -7.456648316814940003 ) ) ;
#11699 = DIRECTION ( 'NONE',  ( -1.224646799147353207E-16, -1.349345573449484691E-32, 1.000000000000000000 ) ) ;
#11700 = LINE ( 'NONE', #23557, #1680 ) ;
#11701 = DIRECTION ( 'NONE',  ( 0.000000000000000000, -0.000000000000000000, -1.000000000000000000 ) ) ;
#11702 = DIRECTION ( 'NONE',  ( -1.000000000000000000, 0.000000000000000000, 0.000000000000000000 ) ) ;
#11703 = TOROIDAL_SURFACE ( 'NONE', #16424, 12.40141737965279667, 0.1249999999999991951 ) ;
#11704 = CIRCLE ( 'NONE', #17462, 2.500000000000002220 ) ;
#11705 = CARTESIAN_POINT ( 'NONE',  ( 47.63716429968715715, 28.19696019071910342, 49.58068632438583734 ) ) ;
#11706 = ORIENTED_EDGE ( 'NONE', *, *, #19702, .T. ) ;
#11707 = DIRECTION ( 'NONE',  ( -1.000000000000000000, 0.000000000000000000, 0.000000000000000000 ) ) ;
#11708 = CARTESIAN_POINT ( 'NONE',  ( 48.34748475735720774, 25.40653309617948352, 49.49898713858203791 ) ) ;
#11709 = DIRECTION ( 'NONE',  ( -1.101824276508909887E-16, 1.000000000000000000, -0.000000000000000000 ) ) ;
#11710 = CARTESIAN_POINT ( 'NONE',  ( 21.09785597605720042, 11.78014697381582643, -8.546216316978195948 ) ) ;
#11711 = VERTEX_POINT ( 'NONE', #20093 ) ;
#11712 = DIRECTION ( 'NONE',  ( -1.000000000000000000, 0.000000000000000000, 0.000000000000000000 ) ) ;
#11713 = CARTESIAN_POINT ( 'NONE',  ( 52.07598125554711999, -5.935454207752202116, 106.6682925056943958 ) ) ;
#11714 = FACE_OUTER_BOUND ( 'NONE', #11882, .T. ) ;
#11715 = EDGE_LOOP ( 'NONE', ( #25334, #17328, #28575, #12056 ) ) ;
#11716 = DIRECTION ( 'NONE',  ( -1.000000000000000000, 0.000000000000000000, 0.000000000000000000 ) ) ;
#11717 = FACE_OUTER_BOUND ( 'NONE', #30779, .T. ) ;
#11718 = CARTESIAN_POINT ( 'NONE',  ( 33.71785032049097453, 31.46664230456641675, 47.04930799450051637 ) ) ;
#11719 = EDGE_CURVE ( 'NONE', #7469, #21385, #29973, .T. ) ;
#11720 = DIRECTION ( 'NONE',  ( -0.000000000000000000, -1.000000000000000000, 0.000000000000000000 ) ) ;
#11721 = VERTEX_POINT ( 'NONE', #7138 ) ;
#11722 = CARTESIAN_POINT ( 'NONE',  ( 73.84527214715876653, 11.92558985988973497, 26.36226255498455728 ) ) ;
#11723 = EDGE_LOOP ( 'NONE', ( #29078, #2600, #4870, #12100 ) ) ;
#11724 = CIRCLE ( 'NONE', #17483, 12.36707279061065101 ) ;
#11725 = B_SPLINE_CURVE_WITH_KNOTS ( 'NONE', 3,
 ( #6623, #13697, #31578, #14180, #16615, #1200 ),
 .UNSPECIFIED., .F., .F.,
 ( 4, 2, 4 ),
 ( 0.000000000000000000, 0.5000000000000000000, 1.000000000000000000 ),
 .UNSPECIFIED. ) ;
#11726 = EDGE_LOOP ( 'NONE', ( #11028, #9211, #6832, #16968 ) ) ;
#11727 = AXIS2_PLACEMENT_3D ( 'NONE', #2546, #10273, #7972 ) ;
#11728 = AXIS2_PLACEMENT_3D ( 'NONE', #6105, #16105, #30423 ) ;
#11729 = AXIS2_PLACEMENT_3D ( 'NONE', #15390, #285, #3060 ) ;
#11730 = CYLINDRICAL_SURFACE ( 'NONE', #5847, 0.1000000000000020595 ) ;
#11731 = LINE ( 'NONE', #19256, #1362 ) ;
#11732 = DIRECTION ( 'NONE',  ( -1.000000000000000000, 0.000000000000000000, 0.000000000000000000 ) ) ;
#11733 = CARTESIAN_POINT ( 'NONE',  ( 81.73634015752263338, -5.935454207752201228, 77.87546120947916961 ) ) ;
#11734 = ORIENTED_EDGE ( 'NONE', *, *, #20888, .F. ) ;
#11735 = DIRECTION ( 'NONE',  ( -0.000000000000000000, -1.000000000000000000, 0.000000000000000000 ) ) ;
#11736 = ORIENTED_EDGE ( 'NONE', *, *, #5837, .T. ) ;
#11737 = CARTESIAN_POINT ( 'NONE',  ( 21.09785597605720753, 13.86454579224779948, 47.04930799450052348 ) ) ;
#11738 =( LENGTH_UNIT ( ) NAMED_UNIT ( * ) SI_UNIT ( .MILLI., .METRE. ) );
#11739 = CARTESIAN_POINT ( 'NONE',  ( 73.09176707068564838, 11.92558985988973497, 67.46350265493038023 ) ) ;
#11740 = ORIENTED_EDGE ( 'NONE', *, *, #776, .T. ) ;
#11741 = CARTESIAN_POINT ( 'NONE',  ( -40.76967387488526384, 8.530668925462078889, 39.44930799450052206 ) ) ;
#11742 = DIRECTION ( 'NONE',  ( -1.000000000000000000, 0.000000000000000000, 0.000000000000000000 ) ) ;
#11743 = SURFACE_STYLE_USAGE ( .BOTH. , #31285 ) ;
#11744 = DIRECTION ( 'NONE',  ( -1.000000000000000000, 0.000000000000000000, 0.000000000000000000 ) ) ;
#11745 = DIRECTION ( 'NONE',  ( -0.9986540920324801229, -6.158269594508763597E-17, -0.05186525298099636111 ) ) ;
#11746 = CARTESIAN_POINT ( 'NONE',  ( 21.09992658989239089, 23.84164230456639544, 47.04930799450051637 ) ) ;
#11747 = DIRECTION ( 'NONE',  ( -1.000000000000000000, 0.000000000000000000, 0.000000000000000000 ) ) ;
#11748 = AXIS2_PLACEMENT_3D ( 'NONE', #6987, #4362, #31457 ) ;
#11749 = DIRECTION ( 'NONE',  ( -1.101824276508909887E-16, 1.000000000000000000, -0.000000000000000000 ) ) ;
#11750 = EDGE_LOOP ( 'NONE', ( #21315, #27379, #30571, #13237 ) ) ;
#11751 = CARTESIAN_POINT ( 'NONE',  ( -40.22853490217747208, 6.951940700334876766, 34.71623747574528807 ) ) ;
#11752 = DIRECTION ( 'NONE',  ( 0.000000000000000000, -0.000000000000000000, -1.000000000000000000 ) ) ;
#11753 = VERTEX_POINT ( 'NONE', #17131 ) ;
#11754 = DIRECTION ( 'NONE',  ( -0.6797146636928672603, -0.1949050434465268711, 0.7071067811865474617 ) ) ;
#11755 = DIRECTION ( 'NONE',  ( -1.101824276508909887E-16, 1.000000000000000000, -0.000000000000000000 ) ) ;
#11756 = EDGE_CURVE ( 'NONE', #12114, #23633, #31532, .T. ) ;
#11757 = ADVANCED_FACE ( 'NONE', ( #16971 ), #15806, .F. ) ;
#11758 = ORIENTED_EDGE ( 'NONE', *, *, #20966, .T. ) ;
#11759 = ADVANCED_FACE ( 'NONE', ( #22224 ), #17366, .F. ) ;
#11760 = ORIENTED_EDGE ( 'NONE', *, *, #21210, .T. ) ;
#11761 = EDGE_CURVE ( 'NONE', #9365, #5667, #15176, .T. ) ;
#11762 = ORIENTED_EDGE ( 'NONE', *, *, #13503, .T. ) ;
#11763 = CIRCLE ( 'NONE', #12292, 0.1999999999999987899 ) ;
#11764 = AXIS2_PLACEMENT_3D ( 'NONE', #1757, #29503, #14401 ) ;
#11765 = VECTOR ( 'NONE', #25465, 1000.000000000000000 ) ;
#11766 = VECTOR ( 'NONE', #19709, 999.9999999999998863 ) ;
#11767 = EDGE_CURVE ( 'NONE', #13582, #17141, #4255, .T. ) ;
#11768 = DIRECTION ( 'NONE',  ( 0.000000000000000000, 1.000000000000000000, 0.000000000000000000 ) ) ;
#11769 = VERTEX_POINT ( 'NONE', #9927 ) ;
#11770 = ORIENTED_EDGE ( 'NONE', *, *, #9200, .F. ) ;
#11771 = CARTESIAN_POINT ( 'NONE',  ( -42.36691375901575185, 13.72999064396537250, 59.48380644099231773 ) ) ;
#11772 = DIRECTION ( 'NONE',  ( -1.000000000000000000, 0.000000000000000000, 0.000000000000000000 ) ) ;
#11773 = LINE ( 'NONE', #7335, #21185 ) ;
#11774 = DIRECTION ( 'NONE',  ( 0.8746197071393926326, -0.4848096202463430537, -8.676864087101709653E-18 ) ) ;
#11775 = CARTESIAN_POINT ( 'NONE',  ( 48.37829923888483563, 28.19452976649965237, 45.07556196625585443 ) ) ;
#11776 = EDGE_CURVE ( 'NONE', #11676, #8185, #8977, .T. ) ;
#11777 = ORIENTED_EDGE ( 'NONE', *, *, #8178, .T. ) ;
#11778 = DIRECTION ( 'NONE',  ( -0.9612616959383205595, -0.2756373558169932236, 1.660411357259282445E-16 ) ) ;
#11779 = ORIENTED_EDGE ( 'NONE', *, *, #3551, .F. ) ;
#11780 = SPHERICAL_SURFACE ( 'NONE', #2236, 0.1000000000000000056 ) ;
#11781 = EDGE_CURVE ( 'NONE', #29845, #23862, #9441, .T. ) ;
#11782 = VERTEX_POINT ( 'NONE', #27152 ) ;
#11783 = CARTESIAN_POINT ( 'NONE',  ( 49.22880864277328072, 29.52863415674993064, 47.27039427357411938 ) ) ;
#11784 = DIRECTION ( 'NONE',  ( 1.188208965918165239E-16, 1.880121038077813132E-16, 1.000000000000000000 ) ) ;
#11785 = CARTESIAN_POINT ( 'NONE',  ( -40.47970302497625994, 7.463434137431150361, 60.54930799450051637 ) ) ;
#11786 = DIRECTION ( 'NONE',  ( -1.101824276508909887E-16, 1.000000000000000000, -0.000000000000000000 ) ) ;
#11787 = FACE_BOUND ( 'NONE', #30958, .T. ) ;
#11788 = CARTESIAN_POINT ( 'NONE',  ( 50.10320668408830613, 25.60621246473838042, 47.20539118556276037 ) ) ;
#11789 = TOROIDAL_SURFACE ( 'NONE', #14414, 12.61792373059896555, 0.1249999999999975853 ) ;
#11790 = DIRECTION ( 'NONE',  ( 0.000000000000000000, -1.000000000000000000, 0.000000000000000000 ) ) ;
#11791 = FACE_OUTER_BOUND ( 'NONE', #4399, .T. ) ;
#11792 = VECTOR ( 'NONE', #8077, 1000.000000000000114 ) ;
#11793 = VERTEX_POINT ( 'NONE', #25188 ) ;
#11794 = DIRECTION ( 'NONE',  ( -1.224646799147353207E-16, -1.349345573449484691E-32, 1.000000000000000000 ) ) ;
#11795 = DIRECTION ( 'NONE',  ( -1.224646799147353207E-16, -1.349345573449484691E-32, 1.000000000000000000 ) ) ;
#11796 = AXIS2_PLACEMENT_3D ( 'NONE', #16853, #7172, #19798 ) ;
#11797 = DIRECTION ( 'NONE',  ( 0.000000000000000000, -0.000000000000000000, -1.000000000000000000 ) ) ;
#11798 = AXIS2_PLACEMENT_3D ( 'NONE', #20131, #27188, #32456 ) ;
#11799 = CIRCLE ( 'NONE', #30149, 39.50000000000000000 ) ;
#11800 = LINE ( 'NONE', #21795, #1173 ) ;
#11801 = CARTESIAN_POINT ( 'NONE',  ( 45.84097905237065618, 22.86454579224779948, 48.98672734302541443 ) ) ;
#11802 = ORIENTED_EDGE ( 'NONE', *, *, #590, .T. ) ;
#11803 = CARTESIAN_POINT ( 'NONE',  ( 33.37634396954528171, 23.59164230456639544, 47.04930799450051637 ) ) ;
#11804 = ORIENTED_EDGE ( 'NONE', *, *, #25320, .F. ) ;
#11805 = DIRECTION ( 'NONE',  ( -0.000000000000000000, -1.000000000000000000, 0.000000000000000000 ) ) ;
#11806 = DIRECTION ( 'NONE',  ( -1.101824276508909887E-16, 1.000000000000000000, -0.000000000000000000 ) ) ;
#11807 = EDGE_CURVE ( 'NONE', #1546, #2479, #24699, .T. ) ;
#11808 = EDGE_LOOP ( 'NONE', ( #12340, #15765 ) ) ;
#11809 = TOROIDAL_SURFACE ( 'NONE', #31215, 12.40141737965286595, 0.1249999999999979183 ) ;
#11810 = VERTEX_POINT ( 'NONE', #32417 ) ;
#11811 = EDGE_CURVE ( 'NONE', #4643, #12963, #29467, .T. ) ;
#11812 = CIRCLE ( 'NONE', #14438, 12.62506659569710443 ) ;
#11813 = LINE ( 'NONE', #21646, #1306 ) ;
#11814 = CARTESIAN_POINT ( 'NONE',  ( 51.92400919103565116, -5.935454207752203004, -13.53511453669547215 ) ) ;
#11816 = FACE_OUTER_BOUND ( 'NONE', #1919, .T. ) ;
#11815 = AXIS2_PLACEMENT_3D ( 'NONE', #6326, #26668, #32262 ) ;
#11817 = AXIS2_PLACEMENT_3D ( 'NONE', #24700, #14858, #9928 ) ;
#11818 = ADVANCED_FACE ( 'NONE', ( #14527 ), #4673, .F. ) ;
#11819 = CIRCLE ( 'NONE', #23349, 0.1250000000000018319 ) ;
#11820 = ORIENTED_EDGE ( 'NONE', *, *, #13860, .F. ) ;
#11821 = CARTESIAN_POINT ( 'NONE',  ( 45.61530479625130852, 22.89977464660286444, 45.91938710987583505 ) ) ;
#11822 = CARTESIAN_POINT ( 'NONE',  ( 21.09785597605720753, 14.56454579224780232, 47.04930799450052348 ) ) ;
#11823 = CARTESIAN_POINT ( 'NONE',  ( 72.70365453605475636, 7.326690775934352473, 18.02522573148189977 ) ) ;
#11824 = EDGE_CURVE ( 'NONE', #16387, #17225, #13197, .T. ) ;
#11825 = ORIENTED_EDGE ( 'NONE', *, *, #20525, .T. ) ;
#11826 = EDGE_LOOP ( 'NONE', ( #8423, #7935, #22448, #31774 ) ) ;
#11827 = EDGE_CURVE ( 'NONE', #4768, #22442, #26785, .T. ) ;
#11828 = ORIENTED_EDGE ( 'NONE', *, *, #19045, .F. ) ;
#11829 = FACE_OUTER_BOUND ( 'NONE', #10977, .T. ) ;
#11830 = DIRECTION ( 'NONE',  ( 0.000000000000000000, 1.000000000000000000, -0.000000000000000000 ) ) ;
#11831 = CYLINDRICAL_SURFACE ( 'NONE', #18367, 31.50000000000000000 ) ;
#11832 = ORIENTED_EDGE ( 'NONE', *, *, #6446, .F. ) ;
#11833 = ORIENTED_EDGE ( 'NONE', *, *, #5537, .F. ) ;
#11834 = CARTESIAN_POINT ( 'NONE',  ( 65.47508102033168598, -13.30632128221580857, 13.00403739414153570 ) ) ;
#11835 = DIRECTION ( 'NONE',  ( 0.9612616959383206705, 0.2756373558169926130, 8.795445018804289444E-19 ) ) ;
#11836 = DIRECTION ( 'NONE',  ( -1.000000000000000000, 0.000000000000000000, 0.000000000000000000 ) ) ;
#11837 = VERTEX_POINT ( 'NONE', #14857 ) ;
#11838 = CARTESIAN_POINT ( 'NONE',  ( -12.08400064424376730, 0.05876815387848967343, -6.781675208179526848 ) ) ;
#11839 = FACE_OUTER_BOUND ( 'NONE', #5562, .T. ) ;
#11840 = ORIENTED_EDGE ( 'NONE', *, *, #10502, .T. ) ;
#11841 = DIRECTION ( 'NONE',  ( 1.000000000000000000, 0.000000000000000000, 0.000000000000000000 ) ) ;
#11842 = CARTESIAN_POINT ( 'NONE',  ( 48.73570333863616355, 26.42287913140504330, 44.52463952959527660 ) ) ;
#11843 = ADVANCED_FACE ( 'NONE', ( #29959 ), #2168, .T. ) ;
#11844 = VECTOR ( 'NONE', #28300, 1000.000000000000000 ) ;
#11845 = PRESENTATION_LAYER_ASSIGNMENT (  '', '', ( #12885 ) ) ;
#11846 = DIRECTION ( 'NONE',  ( 1.000000000000000000, -0.000000000000000000, -0.000000000000000000 ) ) ;
#11847 = EDGE_LOOP ( 'NONE', ( #2594, #16986, #22221, #11264 ) ) ;
#11848 = ADVANCED_FACE ( 'NONE', ( #24861 ), #14757, .T. ) ;
#11849 = DIRECTION ( 'NONE',  ( -1.000000000000000000, 0.000000000000000000, 0.000000000000000000 ) ) ;
#11850 = CARTESIAN_POINT ( 'NONE',  ( 21.09785597605719332, 17.36451738380053555, 34.26511779397349500 ) ) ;
#11851 = CARTESIAN_POINT ( 'NONE',  ( 45.38854177497844944, 26.26952976649965876, 45.94041160078741370 ) ) ;
#11852 = EDGE_CURVE ( 'NONE', #28587, #7860, #8273, .T. ) ;
#11853 = ORIENTED_EDGE ( 'NONE', *, *, #28914, .F. ) ;
#11854 = DIRECTION ( 'NONE',  ( 0.000000000000000000, 0.000000000000000000, 1.000000000000000000 ) ) ;
#11855 = DIRECTION ( 'NONE',  ( -0.000000000000000000, 1.000000000000000000, -0.000000000000000000 ) ) ;
#11856 = CIRCLE ( 'NONE', #10817, 12.62506659569710266 ) ;
#11857 = DIRECTION ( 'NONE',  ( -0.000000000000000000, 1.000000000000000000, -0.000000000000000000 ) ) ;
#11858 = STYLED_ITEM ( 'NONE', ( #13649 ), #12811 ) ;
#11859 = ADVANCED_FACE ( 'NONE', ( #5334, #13213 ), #25665, .T. ) ;
#11860 = CARTESIAN_POINT ( 'NONE',  ( 45.36511207810799107, 26.50948166895304325, 45.12672418911606087 ) ) ;
#11861 = EDGE_CURVE ( 'NONE', #1224, #9654, #17447, .T. ) ;
#11862 = DIRECTION ( 'NONE',  ( 0.1949050434465268156, -0.6797146636928675933, -0.7071067811865470176 ) ) ;
#11863 = PLANE ( 'NONE',  #3199 ) ;
#11864 = CARTESIAN_POINT ( 'NONE',  ( 21.09992658989238734, 38.56284415653841791, 47.04930799450051637 ) ) ;
#11865 = ORIENTED_EDGE ( 'NONE', *, *, #17828, .T. ) ;
#11866 = DIRECTION ( 'NONE',  ( -1.000000000000000000, -1.101824276508909887E-16, 0.000000000000000000 ) ) ;
#11867 = DIRECTION ( 'NONE',  ( -1.101824276508909887E-16, 1.000000000000000000, -0.000000000000000000 ) ) ;
#11868 = TOROIDAL_SURFACE ( 'NONE', #16055, 12.40141737965281976, 0.1249999999999999722 ) ;
#11869 = CARTESIAN_POINT ( 'NONE',  ( 21.09992658989239089, 29.59184655352418858, 47.04930799450051637 ) ) ;
#11870 = ORIENTED_EDGE ( 'NONE', *, *, #1359, .T. ) ;
#11871 = DIRECTION ( 'NONE',  ( -1.101824276508909887E-16, 1.000000000000000000, -0.000000000000000000 ) ) ;
#11872 = CARTESIAN_POINT ( 'NONE',  ( -40.18454328187963398, 7.548069831825863218, 60.44930799450051495 ) ) ;
#11873 = DIRECTION ( 'NONE',  ( -1.000000000000000000, -1.101824276508909887E-16, 0.000000000000000000 ) ) ;
#11874 = ORIENTED_EDGE ( 'NONE', *, *, #30428, .T. ) ;
#11875 = ORIENTED_EDGE ( 'NONE', *, *, #714, .T. ) ;
#11876 = CARTESIAN_POINT ( 'NONE',  ( 21.09992658989239089, 30.59164230456639544, 47.04930799450051637 ) ) ;
#11877 = DIRECTION ( 'NONE',  ( 1.000000000000000000, 0.000000000000000000, 0.000000000000000000 ) ) ;
#11878 = PLANE ( 'NONE',  #2606 ) ;
#11879 = DIRECTION ( 'NONE',  ( -1.101824276508909887E-16, 1.000000000000000000, -0.000000000000000000 ) ) ;
#11880 = EDGE_LOOP ( 'NONE', ( #27640, #4180, #20386, #19073 ) ) ;
#11881 = CARTESIAN_POINT ( 'NONE',  ( 45.11371142117359057, 29.27222086838446202, 45.70422120043853909 ) ) ;
#11882 = EDGE_LOOP ( 'NONE', ( #30505, #13915, #14275, #26679, #22550, #15492 ) ) ;
#11883 = CIRCLE ( 'NONE', #25522, 12.62506659569710443 ) ;
#11884 = PRODUCT_DEFINITION_FORMATION_WITH_SPECIFIED_SOURCE ( 'ANY', '', #7202, .NOT_KNOWN. ) ;
#11885 = VERTEX_POINT ( 'NONE', #8435 ) ;
#11886 = EDGE_CURVE ( 'NONE', #25156, #3119, #28140, .T. ) ;
#11887 = CIRCLE ( 'NONE', #8737, 0.1250000000000001110 ) ;
#11888 = ORIENTED_EDGE ( 'NONE', *, *, #28579, .T. ) ;
#11889 = CARTESIAN_POINT ( 'NONE',  ( 21.09992658989239089, 24.59184655352419213, 47.04930799450051637 ) ) ;
#11890 = DIRECTION ( 'NONE',  ( -1.000000000000000000, 0.000000000000000000, 0.000000000000000000 ) ) ;
#11891 = CARTESIAN_POINT ( 'NONE',  ( 21.09992658989238734, 32.59164230456639899, 47.04930799450051637 ) ) ;
#11892 = B_SPLINE_CURVE_WITH_KNOTS ( 'NONE', 3,
 ( #18299, #8467, #31276, #8627 ),
 .UNSPECIFIED., .F., .F.,
 ( 4, 4 ),
 ( 0.000000000000000000, 0.0001058398962549312607 ),
 .UNSPECIFIED. ) ;
#11893 = EDGE_CURVE ( 'NONE', #20681, #2165, #28774, .T. ) ;
#11894 = ORIENTED_EDGE ( 'NONE', *, *, #32219, .T. ) ;
#11895 = CARTESIAN_POINT ( 'NONE',  ( 21.09785597605720042, -16.03545420775220265, 47.04930799450051637 ) ) ;
#11896 = ORIENTED_EDGE ( 'NONE', *, *, #31220, .F. ) ;
#11897 = DIRECTION ( 'NONE',  ( -1.000000000000000000, 0.000000000000000000, 0.000000000000000000 ) ) ;
#11898 = CARTESIAN_POINT ( 'NONE',  ( -41.13768170161382898, 11.26524684725914227, 37.04930799450052348 ) ) ;
#11899 = CARTESIAN_POINT ( 'NONE',  ( 71.56952591989053758, 10.07270486929681930, 73.29201046826767652 ) ) ;
#11900 = EDGE_LOOP ( 'NONE', ( #26229, #25009, #11179, #16857 ) ) ;
#11901 = CARTESIAN_POINT ( 'NONE',  ( -17.40214402394279247, 13.86454579224779948, 47.04930799450052348 ) ) ;
#11902 = VECTOR ( 'NONE', #3349, 1000.000000000000000 ) ;
#11903 = DIRECTION ( 'NONE',  ( -0.000000000000000000, -1.000000000000000000, 0.000000000000000000 ) ) ;
#11904 = CARTESIAN_POINT ( 'NONE',  ( 21.09785597605721108, -16.93545420775220478, 125.4493079945005150 ) ) ;
#11905 = FACE_OUTER_BOUND ( 'NONE', #26225, .T. ) ;
#11906 = CARTESIAN_POINT ( 'NONE',  ( 21.09992658989238734, 32.09143805560860585, 47.04930799450051637 ) ) ;
#11907 = ORIENTED_EDGE ( 'NONE', *, *, #1662, .T. ) ;
#11908 = CARTESIAN_POINT ( 'NONE',  ( -38.41701585771487260, 6.978388747684010518, 32.04930799450052348 ) ) ;
#11909 = DIRECTION ( 'NONE',  ( -1.000000000000000000, 0.000000000000000000, 0.000000000000000000 ) ) ;
#11910 = VERTEX_POINT ( 'NONE', #25508 ) ;
#11911 = CARTESIAN_POINT ( 'NONE',  ( 21.09992658989239089, 25.34164230456639899, 47.04930799450051637 ) ) ;
#11912 = DIRECTION ( 'NONE',  ( -1.000000000000000000, -1.101824276508909764E-16, 0.000000000000000000 ) ) ;
#11913 = ORIENTED_EDGE ( 'NONE', *, *, #8451, .T. ) ;
#11914 = ORIENTED_EDGE ( 'NONE', *, *, #22197, .T. ) ;
#11915 = PRODUCT_RELATED_PRODUCT_CATEGORY ( 'part', '', ( #29749 ) ) ;
#11916 = AXIS2_PLACEMENT_3D ( 'NONE', #22500, #31, #17584 ) ;
#11917 = ORIENTED_EDGE ( 'NONE', *, *, #7950, .T. ) ;
#11918 = AXIS2_PLACEMENT_3D ( 'NONE', #19211, #6598, #29238 ) ;
#11919 = AXIS2_PLACEMENT_3D ( 'NONE', #17440, #27462, #4977 ) ;
#11920 = AXIS2_PLACEMENT_3D ( 'NONE', #7191, #26403, #9325 ) ;
#11921 = CONICAL_SURFACE ( 'NONE', #9832, 39.63553620740810857, 0.6632251157578421541 ) ;
#11922 = DIRECTION ( 'NONE',  ( -0.2756373558169926130, 0.9612616959383207815, -2.065119226596364453E-17 ) ) ;
#11923 = ADVANCED_FACE ( 'NONE', ( #10586 ), #25982, .F. ) ;
#11924 = ORIENTED_EDGE ( 'NONE', *, *, #29161, .F. ) ;
#11925 = ORIENTED_EDGE ( 'NONE', *, *, #5589, .F. ) ;
#11926 = LINE ( 'NONE', #18255, #4293 ) ;
#11927 = ADVANCED_FACE ( 'NONE', ( #30276 ), #25348, .F. ) ;
#11928 = EDGE_CURVE ( 'NONE', #25082, #16711, #15275, .T. ) ;
#11929 = CARTESIAN_POINT ( 'NONE',  ( -39.45773241730296377, -5.935454212835550969, 77.98461610899785512 ) ) ;
#11930 = EDGE_CURVE ( 'NONE', #6715, #23081, #1103, .T. ) ;
#11931 = FACE_BOUND ( 'NONE', #21143, .T. ) ;
#11932 = DIRECTION ( 'NONE',  ( 2.779292025043186357E-18, -1.288349127009862057E-17, 1.000000000000000000 ) ) ;
#11933 = EDGE_CURVE ( 'NONE', #17141, #4744, #600, .T. ) ;
#11934 = CARTESIAN_POINT ( 'NONE',  ( 46.02876340639226527, 26.91119643316632093, 44.95353858666495483 ) ) ;
#11935 = ORIENTED_EDGE ( 'NONE', *, *, #23234, .T. ) ;
#11937 = EDGE_CURVE ( 'NONE', #9226, #32103, #20579, .T. ) ;
#11936 = CARTESIAN_POINT ( 'NONE',  ( -5.950449876020693196, 9.421471677506305653, 97.50311162695551559 ) ) ;
#11938 = VERTEX_POINT ( 'NONE', #5816 ) ;
#11939 = CARTESIAN_POINT ( 'NONE',  ( -12.52393922272763227, -3.543532154952163893, -7.915647480175222128 ) ) ;
#11940 = ORIENTED_EDGE ( 'NONE', *, *, #31947, .T. ) ;
#11941 = DIRECTION ( 'NONE',  ( -1.000000000000000000, 0.000000000000000000, 0.000000000000000000 ) ) ;
#11942 = CARTESIAN_POINT ( 'NONE',  ( -41.07560527903737579, 9.385057823277964673, 35.44930799450052206 ) ) ;
#11943 = DIRECTION ( 'NONE',  ( 0.000000000000000000, 0.000000000000000000, -1.000000000000000000 ) ) ;
#11944 = CARTESIAN_POINT ( 'NONE',  ( 33.72499318558949710, 30.34143805560860585, 47.04930799450051637 ) ) ;
#11945 = FACE_OUTER_BOUND ( 'NONE', #17501, .T. ) ;
#11946 = CARTESIAN_POINT ( 'NONE',  ( 48.73570333863616355, 27.12287913140504259, 44.52463952959527660 ) ) ;
#11947 = CARTESIAN_POINT ( 'NONE',  ( 47.47590639978425031, 23.04411657098542321, 48.12004267350693709 ) ) ;
#11948 = FACE_OUTER_BOUND ( 'NONE', #17033, .T. ) ;
#11949 = ORIENTED_EDGE ( 'NONE', *, *, #28426, .F. ) ;
#11950 = FACE_OUTER_BOUND ( 'NONE', #1203, .T. ) ;
#11951 = FACE_OUTER_BOUND ( 'NONE', #28446, .T. ) ;
#11952 = AXIS2_PLACEMENT_3D ( 'NONE', #26892, #14104, #16388 ) ;
#11953 = DIRECTION ( 'NONE',  ( 0.000000000000000000, 0.000000000000000000, 1.000000000000000000 ) ) ;
#11954 = AXIS2_PLACEMENT_3D ( 'NONE', #10929, #20608, #30956 ) ;
#11955 = CARTESIAN_POINT ( 'NONE',  ( 48.55603101936429056, 22.91413368675619111, 45.98877541807350156 ) ) ;
#11956 = CARTESIAN_POINT ( 'NONE',  ( -38.57628410747783221, 11.92829594627139933, 24.97746215641624090 ) ) ;
#11957 = AXIS2_PLACEMENT_3D ( 'NONE', #23528, #25830, #13375 ) ;
#11958 = EDGE_LOOP ( 'NONE', ( #6159, #20352, #21270, #4788 ) ) ;
#11959 = AXIS2_PLACEMENT_3D ( 'NONE', #27047, #14910, #20143 ) ;
#11960 = ORIENTED_EDGE ( 'NONE', *, *, #17634, .T. ) ;
#11961 = CYLINDRICAL_SURFACE ( 'NONE', #23549, 12.36707279061065279 ) ;
#11962 = CARTESIAN_POINT ( 'NONE',  ( 21.09785597605719332, 11.78014697381582643, 47.04930799450051637 ) ) ;
#11963 = AXIS2_PLACEMENT_3D ( 'NONE', #3485, #1184, #23514 ) ;
#11964 = ORIENTED_EDGE ( 'NONE', *, *, #3227, .T. ) ;
#11965 = ADVANCED_FACE ( 'NONE', ( #15819 ), #28769, .T. ) ;
#11966 = ORIENTED_EDGE ( 'NONE', *, *, #4944, .F. ) ;
#11967 = CARTESIAN_POINT ( 'NONE',  ( 21.09785597605719332, 38.31023907818019580, 47.04930799450051637 ) ) ;
#11968 = DIRECTION ( 'NONE',  ( -1.000000000000000000, 0.000000000000000000, 0.000000000000000000 ) ) ;
#11969 = LINE ( 'NONE', #5193, #30430 ) ;
#11970 = AXIS2_PLACEMENT_3D ( 'NONE', #15129, #20530, #10047 ) ;
#11971 = AXIS2_PLACEMENT_3D ( 'NONE', #24631, #22166, #31701 ) ;
#11972 = ORIENTED_EDGE ( 'NONE', *, *, #4133, .T. ) ;
#11973 = AXIS2_PLACEMENT_3D ( 'NONE', #7965, #15342, #30766 ) ;
#11974 = ADVANCED_FACE ( 'NONE', ( #21359 ), #30995, .T. ) ;
#11975 = CARTESIAN_POINT ( 'NONE',  ( 21.09785597605720753, -5.098646251524523443, 47.04930799450052348 ) ) ;
#11976 = ADVANCED_FACE ( 'NONE', ( #26625 ), #1514, .T. ) ;
#11977 = CIRCLE ( 'NONE', #18769, 1.500000000000001332 ) ;
#11978 = CARTESIAN_POINT ( 'NONE',  ( 8.474859994195286461, 30.34143805560860585, 47.04930799450051637 ) ) ;
#11979 = CYLINDRICAL_SURFACE ( 'NONE', #28449, 12.62506659569710266 ) ;
#11980 = EDGE_CURVE ( 'NONE', #20581, #16953, #3214, .T. ) ;
#11981 = ORIENTED_EDGE ( 'NONE', *, *, #18374, .F. ) ;
#11982 = EDGE_LOOP ( 'NONE', ( #875, #29753, #25300, #18963 ) ) ;
#11983 = DIRECTION ( 'NONE',  ( 0.6184495258776571136, -0.3428121700606572286, -0.7071067811865505703 ) ) ;
#11984 = EDGE_LOOP ( 'NONE', ( #27240, #23490, #5993, #15946, #21376 ) ) ;
#11985 = TOROIDAL_SURFACE ( 'NONE', #26660, 17.50000000000000000, 1.999999999999998224 ) ;
#11986 = DIRECTION ( 'NONE',  ( -1.000000000000000000, 0.000000000000000000, 0.000000000000000000 ) ) ;
#11987 = CARTESIAN_POINT ( 'NONE',  ( 21.09992658989238734, 38.56284415653841791, 47.04930799450051637 ) ) ;
#11988 = DIRECTION ( 'NONE',  ( -1.000000000000000000, 0.000000000000000000, 0.000000000000000000 ) ) ;
#11989 = FACE_OUTER_BOUND ( 'NONE', #13294, .T. ) ;
#11990 = DIRECTION ( 'NONE',  ( 1.000000000000000000, 0.000000000000000000, 0.000000000000000000 ) ) ;
#11991 = VERTEX_POINT ( 'NONE', #28611 ) ;
#11992 = EDGE_LOOP ( 'NONE', ( #3784, #24790, #4331, #24293 ) ) ;
#11993 = DIRECTION ( 'NONE',  ( -0.000000000000000000, -1.000000000000000000, 0.000000000000000000 ) ) ;
#11994 = PLANE ( 'NONE',  #5189 ) ;
#11995 = CARTESIAN_POINT ( 'NONE',  ( 21.09785597605720753, 13.78276522714992147, 47.04930799450052348 ) ) ;
#11996 = ORIENTED_EDGE ( 'NONE', *, *, #26298, .T. ) ;
#11997 = FACE_OUTER_BOUND ( 'NONE', #1118, .T. ) ;
#11998 = CARTESIAN_POINT ( 'NONE',  ( 36.19429842010746512, -13.74047052604243646, 103.4110129320798563 ) ) ;
#11999 = ORIENTED_EDGE ( 'NONE', *, *, #1745, .T. ) ;
#12000 = PLANE ( 'NONE',  #19950 ) ;
#12001 = CARTESIAN_POINT ( 'NONE',  ( 21.09992658989238734, 38.56284415653841791, 47.04930799450051637 ) ) ;
#12002 = VECTOR ( 'NONE', #25575, 1000.000000000000000 ) ;
#12003 = AXIS2_PLACEMENT_3D ( 'NONE', #12214, #31905, #22368 ) ;
#12004 = FACE_OUTER_BOUND ( 'NONE', #12873, .T. ) ;
#12005 = VECTOR ( 'NONE', #18707, 1000.000000000000000 ) ;
#12006 = ADVANCED_FACE ( 'NONE', ( #31566 ), #5322, .T. ) ;
#12007 = AXIS2_PLACEMENT_3D ( 'NONE', #22287, #16871, #12907 ) ;
#12008 = ORIENTED_EDGE ( 'NONE', *, *, #28676, .T. ) ;
#12009 = DIRECTION ( 'NONE',  ( -0.2250569586005261857, 0.7848668881104258199, 0.5773502691896292838 ) ) ;
#12010 = CARTESIAN_POINT ( 'NONE',  ( -41.93344242462055149, 13.82826554927148166, 54.56265170360538264 ) ) ;
#12011 = CARTESIAN_POINT ( 'NONE',  ( 44.74832014356462651, 25.62786309983298949, 46.92728461490987257 ) ) ;
#12012 = VERTEX_POINT ( 'NONE', #9073 ) ;
#12013 = DIRECTION ( 'NONE',  ( 0.000000000000000000, 1.000000000000000000, -0.000000000000000000 ) ) ;
#12014 = DIRECTION ( 'NONE',  ( -0.000000000000000000, -1.000000000000000000, -0.000000000000000000 ) ) ;
#12015 = EDGE_CURVE ( 'NONE', #1960, #30715, #26422, .T. ) ;
#12016 = CARTESIAN_POINT ( 'NONE',  ( 53.16699371189685053, -5.614579432636292111, -10.15581503676737185 ) ) ;
#12017 = AXIS2_PLACEMENT_3D ( 'NONE', #28170, #5683, #25705 ) ;
#12018 = CIRCLE ( 'NONE', #30375, 0.9000000000000011324 ) ;
#12019 = CARTESIAN_POINT ( 'NONE',  ( -22.40214402394279247, -5.098646251524523443, 47.04930799450052348 ) ) ;
#12020 = DIRECTION ( 'NONE',  ( -1.000000000000000000, 0.000000000000000000, 0.000000000000000000 ) ) ;
#12021 = DIRECTION ( 'NONE',  ( -1.101824276508909887E-16, 1.000000000000000000, -0.000000000000000000 ) ) ;
#12022 = CARTESIAN_POINT ( 'NONE',  ( 47.09785597605719687, 25.56454579224779877, 49.54930799450042400 ) ) ;
#12023 = FACE_OUTER_BOUND ( 'NONE', #26750, .T. ) ;
#12024 = CARTESIAN_POINT ( 'NONE',  ( -42.68872152249107188, 16.18454730271123054, 55.97778115698459089 ) ) ;
#12025 = ORIENTED_EDGE ( 'NONE', *, *, #27201, .T. ) ;
#12026 = FACE_OUTER_BOUND ( 'NONE', #28847, .T. ) ;
#12027 = CARTESIAN_POINT ( 'NONE',  ( -40.43834990939047458, 8.528791397241549888, 34.55055826194722357 ) ) ;
#12028 = DIRECTION ( 'NONE',  ( -1.000000000000000000, 0.000000000000000000, 0.000000000000000000 ) ) ;
#12029 = VECTOR ( 'NONE', #9585, 1000.000000000000000 ) ;
#12030 = CARTESIAN_POINT ( 'NONE',  ( 54.14309329449467612, -4.768257113790710378, 103.1530495731739592 ) ) ;
#12031 = ORIENTED_EDGE ( 'NONE', *, *, #22578, .F. ) ;
#12032 = DIRECTION ( 'NONE',  ( 0.000000000000000000, -0.000000000000000000, -1.000000000000000000 ) ) ;
#12033 = CIRCLE ( 'NONE', #2609, 12.62506659569710266 ) ;
#12034 = CARTESIAN_POINT ( 'NONE',  ( -40.59758774925371938, 7.567737757495682338, 35.43807061034478778 ) ) ;
#12035 = CARTESIAN_POINT ( 'NONE',  ( 21.09992658989238734, 38.56284415653841791, 47.04930799450051637 ) ) ;
#12036 = EDGE_CURVE ( 'NONE', #19007, #24927, #14068, .T. ) ;
#12037 = ORIENTED_EDGE ( 'NONE', *, *, #20850, .F. ) ;
#12038 = ORIENTED_EDGE ( 'NONE', *, *, #5434, .T. ) ;
#12039 = CARTESIAN_POINT ( 'NONE',  ( -40.02540636251514172, 2.839176264122877047, 58.54930799450051637 ) ) ;
#12040 = CARTESIAN_POINT ( 'NONE',  ( 45.79384627280941089, 29.26618040159425860, 49.05938063676249072 ) ) ;
#12041 = FACE_OUTER_BOUND ( 'NONE', #9601, .T. ) ;
#12042 = EDGE_CURVE ( 'NONE', #24243, #29876, #19455, .T. ) ;
#12043 = CARTESIAN_POINT ( 'NONE',  ( -41.94956971822180947, 3.905757428664828890, 47.04930799450051637 ) ) ;
#12044 = ORIENTED_EDGE ( 'NONE', *, *, #5499, .F. ) ;
#12045 = CARTESIAN_POINT ( 'NONE',  ( 72.58709125692084285, 11.83483724345210142, 25.26238199259950079 ) ) ;
#12046 = EDGE_LOOP ( 'NONE', ( #24626, #17124, #26874, #15315, #29984 ) ) ;
#12047 = ADVANCED_FACE ( 'NONE', ( #23524 ), #4792, .F. ) ;
#12048 = AXIS2_PLACEMENT_3D ( 'NONE', #25186, #2212, #5008 ) ;
#12049 = ADVANCED_FACE ( 'NONE', ( #13843 ), #18927, .T. ) ;
#12050 = VECTOR ( 'NONE', #22328, 1000.000000000000000 ) ;
#12051 = EDGE_LOOP ( 'NONE', ( #13370, #8274, #32378, #8944 ) ) ;
#12052 = ADVANCED_FACE ( 'NONE', ( #21049 ), #3658, .F. ) ;
#12053 = FACE_OUTER_BOUND ( 'NONE', #28839, .T. ) ;
#12054 = VECTOR ( 'NONE', #7447, 1000.000000000000114 ) ;
#12055 = AXIS2_PLACEMENT_3D ( 'NONE', #24843, #17448, #22366 ) ;
#12056 = ORIENTED_EDGE ( 'NONE', *, *, #11564, .F. ) ;
#12057 = CARTESIAN_POINT ( 'NONE',  ( -30.88776582636845092, 11.92558985988972786, 67.48460561594581009 ) ) ;
#12058 = CARTESIAN_POINT ( 'NONE',  ( -29.85004370764308490, 6.158867040949189686, 76.91207085872912330 ) ) ;
#12059 = CARTESIAN_POINT ( 'NONE',  ( -29.27613032885505007, 11.92829597396328012, 69.12115383893792853 ) ) ;
#12060 = AXIS2_PLACEMENT_3D ( 'NONE', #32463, #22763, #25551 ) ;
#12061 = EDGE_CURVE ( 'NONE', #24037, #8764, #13687, .T. ) ;
#12062 = VECTOR ( 'NONE', #23380, 1000.000000000000000 ) ;
#12063 = VERTEX_POINT ( 'NONE', #26310 ) ;
#12064 = CARTESIAN_POINT ( 'NONE',  ( 51.97542764375435809, -5.937448199248382075, -13.65255231306078798 ) ) ;
#12065 = ORIENTED_EDGE ( 'NONE', *, *, #590, .F. ) ;
#12066 = DIRECTION ( 'NONE',  ( -1.101824276508909887E-16, 1.000000000000000000, -0.000000000000000000 ) ) ;
#12067 = DIRECTION ( 'NONE',  ( -1.101824276508909887E-16, 1.000000000000000000, -0.000000000000000000 ) ) ;
#12068 = CARTESIAN_POINT ( 'NONE',  ( 21.09992658989239089, 24.72145308207319303, 47.04930799450051637 ) ) ;
#12069 = ORIENTED_EDGE ( 'NONE', *, *, #8300, .F. ) ;
#12070 = CARTESIAN_POINT ( 'NONE',  ( 21.09992658989239089, 29.34164230456639899, 47.04930799450051637 ) ) ;
#12071 = DIRECTION ( 'NONE',  ( 0.000000000000000000, -0.000000000000000000, -1.000000000000000000 ) ) ;
#12072 = DIRECTION ( 'NONE',  ( 0.1949050434465251225, -0.6797146636928670382, 0.7071067811865481278 ) ) ;
#12073 = AXIS2_PLACEMENT_3D ( 'NONE', #17426, #22507, #9728 ) ;
#12074 = DIRECTION ( 'NONE',  ( 0.8746197071393926326, -0.4848096202463430537, -8.676864087101709653E-18 ) ) ;
#12075 = DIRECTION ( 'NONE',  ( -1.000000000000000000, 0.000000000000000000, 0.000000000000000000 ) ) ;
#12076 = CARTESIAN_POINT ( 'NONE',  ( -40.22836982583548604, 6.952244300597145710, 34.71735136656046450 ) ) ;
#12077 = DIRECTION ( 'NONE',  ( -1.000000000000000000, 0.000000000000000000, 0.000000000000000000 ) ) ;
#12078 = VERTEX_POINT ( 'NONE', #4800 ) ;
#12079 = CARTESIAN_POINT ( 'NONE',  ( -40.06891218940336330, 7.538004613239514207, 35.29832907986742185 ) ) ;
#12080 = DIRECTION ( 'NONE',  ( 0.000000000000000000, 0.000000000000000000, -1.000000000000000000 ) ) ;
#12081 = EDGE_CURVE ( 'NONE', #31932, #17073, #16935, .T. ) ;
#12082 = VERTEX_POINT ( 'NONE', #19564 ) ;
#12083 = LINE ( 'NONE', #7151, #2535 ) ;
#12084 = VECTOR ( 'NONE', #18510, 1000.000000000000114 ) ;
#12085 = CIRCLE ( 'NONE', #3157, 0.09999999999999795164 ) ;
#12086 = EDGE_CURVE ( 'NONE', #7375, #23526, #22188, .T. ) ;
#12087 = DIRECTION ( 'NONE',  ( -0.8746197071393858602, 0.4848096202463547666, 0.000000000000000000 ) ) ;
#12088 = ORIENTED_EDGE ( 'NONE', *, *, #4536, .T. ) ;
#12089 = AXIS2_PLACEMENT_3D ( 'NONE', #31167, #3266, #31009 ) ;
#12090 = ORIENTED_EDGE ( 'NONE', *, *, #18520, .T. ) ;
#12091 = AXIS2_PLACEMENT_3D ( 'NONE', #23892, #31452, #21581 ) ;
#12092 = AXIS2_PLACEMENT_3D ( 'NONE', #14343, #14671, #22034 ) ;
#12093 = CIRCLE ( 'NONE', #11043, 0.1000000000000016431 ) ;
#12094 = EDGE_CURVE ( 'NONE', #18864, #26491, #1135, .T. ) ;
#12095 = ORIENTED_EDGE ( 'NONE', *, *, #23018, .T. ) ;
#12096 = TOROIDAL_SURFACE ( 'NONE', #14203, 12.40141737965281621, 0.1249999999999985428 ) ;
#12097 = LINE ( 'NONE', #7819, #16666 ) ;
#12098 = VECTOR ( 'NONE', #12932, 1000.000000000000000 ) ;
#12099 = EDGE_LOOP ( 'NONE', ( #169, #11159, #21134, #2625 ) ) ;
#12100 = ORIENTED_EDGE ( 'NONE', *, *, #24470, .T. ) ;
#12101 = DIRECTION ( 'NONE',  ( -0.1949050434465267878, 0.6797146636928665941, -0.7071067811865480168 ) ) ;
#12102 = DIRECTION ( 'NONE',  ( -1.101824276508909887E-16, 1.000000000000000000, -0.000000000000000000 ) ) ;
#12103 = AXIS2_PLACEMENT_3D ( 'NONE', #31293, #8167, #28515 ) ;
#12104 = DIRECTION ( 'NONE',  ( -0.000000000000000000, -1.000000000000000000, 0.000000000000000000 ) ) ;
#12105 = DIRECTION ( 'NONE',  ( -1.101824276508909887E-16, 1.000000000000000000, -0.000000000000000000 ) ) ;
#12106 = CIRCLE ( 'NONE', #2150, 0.1250000000000001110 ) ;
#12107 = CYLINDRICAL_SURFACE ( 'NONE', #29366, 0.1000000000000006301 ) ;
#12108 = ORIENTED_EDGE ( 'NONE', *, *, #17453, .T. ) ;
#12109 = CARTESIAN_POINT ( 'NONE',  ( -39.58809650894544774, 2.596771453999702661, 48.54930799450051637 ) ) ;
#12110 = ORIENTED_EDGE ( 'NONE', *, *, #10040, .F. ) ;
#12111 = CARTESIAN_POINT ( 'NONE',  ( 33.46699938050304013, 28.97145308207318237, 47.04930799450050927 ) ) ;
#12112 = CARTESIAN_POINT ( 'NONE',  ( -11.17519415121370763, 2.112486173643649767, -5.064473702997324800 ) ) ;
#12113 = AXIS2_PLACEMENT_3D ( 'NONE', #18748, #3668, #21215 ) ;
#12114 = VERTEX_POINT ( 'NONE', #17262 ) ;
#12115 = DIRECTION ( 'NONE',  ( 0.000000000000000000, 1.000000000000000000, 0.000000000000000000 ) ) ;
#12116 = DIRECTION ( 'NONE',  ( -1.000000000000000000, 0.000000000000000000, 0.000000000000000000 ) ) ;
#12117 = CARTESIAN_POINT ( 'NONE',  ( 52.13943755312613604, -5.936969727347465309, 107.6745679524140229 ) ) ;
#12118 = CARTESIAN_POINT ( 'NONE',  ( 47.09785597605719687, 24.86454579224779948, 44.54930799450042400 ) ) ;
#12119 = DIRECTION ( 'NONE',  ( -1.101824276508909887E-16, 1.000000000000000000, -0.000000000000000000 ) ) ;
#12120 = CARTESIAN_POINT ( 'NONE',  ( 44.77625694075214824, 27.41454579807170688, 48.23360063142255427 ) ) ;
#12121 = CYLINDRICAL_SURFACE ( 'NONE', #24155, 0.1000000000000008243 ) ;
#12122 = DIRECTION ( 'NONE',  ( 0.1949050434465265935, -0.6797146636928685925, -0.7071067811865462405 ) ) ;
#12123 = EDGE_LOOP ( 'NONE', ( #21594, #2381 ) ) ;
#12124 = DIRECTION ( 'NONE',  ( 0.000000000000000000, -0.000000000000000000, -1.000000000000000000 ) ) ;
#12125 = DIRECTION ( 'NONE',  ( 0.9612616959383207815, 0.2756373558169926685, 8.795445018804289444E-19 ) ) ;
#12126 = AXIS2_PLACEMENT_3D ( 'NONE', #12220, #24513, #16632 ) ;
#12127 = CARTESIAN_POINT ( 'NONE',  ( 100.3079064823960493, -16.63545420775219696, 47.04930799450134771 ) ) ;
#12128 = CARTESIAN_POINT ( 'NONE',  ( -37.49824857498671093, 12.70128680827697387, 57.04930799450051637 ) ) ;
#12129 = DIRECTION ( 'NONE',  ( -1.000000000000000000, 0.000000000000000000, 0.000000000000000000 ) ) ;
#12130 = VERTEX_POINT ( 'NONE', #29425 ) ;
#12131 = ORIENTED_EDGE ( 'NONE', *, *, #21747, .T. ) ;
#12132 = CARTESIAN_POINT ( 'NONE',  ( -42.30123736278718383, 13.66041317296246937, 54.56265170360538264 ) ) ;
#12133 = EDGE_CURVE ( 'NONE', #21157, #9796, #14980, .T. ) ;
#12134 = ORIENTED_EDGE ( 'NONE', *, *, #11197, .T. ) ;
#12135 = AXIS2_PLACEMENT_3D ( 'NONE', #12742, #2868, #24876 ) ;
#12136 = AXIS2_PLACEMENT_3D ( 'NONE', #8906, #6453, #4141 ) ;
#12137 = AXIS2_PLACEMENT_3D ( 'NONE', #18990, #29018, #16535 ) ;
#12138 = AXIS2_PLACEMENT_3D ( 'NONE', #3699, #1553, #24041 ) ;
#12139 = ORIENTED_EDGE ( 'NONE', *, *, #7820, .T. ) ;
#12140 = DIRECTION ( 'NONE',  ( -0.9612616959383221138, -0.2756373558169876170, 0.000000000000000000 ) ) ;
#12141 = CARTESIAN_POINT ( 'NONE',  ( 51.94765923753424630, -5.936248947737084336, -13.45830144247714344 ) ) ;
#12142 = VECTOR ( 'NONE', #17670, 1000.000000000000000 ) ;
#12143 = ORIENTED_EDGE ( 'NONE', *, *, #4300, .F. ) ;
#12144 = DIRECTION ( 'NONE',  ( 0.4544104193609911913, 0.000000000000000000, 0.8907924397839085406 ) ) ;
#12145 = DIRECTION ( 'NONE',  ( 0.7549115352271290602, 0.6546536707079775308, 0.03920644602090527647 ) ) ;
#12146 = CARTESIAN_POINT ( 'NONE',  ( 21.09992658989238734, 32.55121380581068991, 47.04930799450051637 ) ) ;
#12147 = ORIENTED_EDGE ( 'NONE', *, *, #16340, .F. ) ;
#12148 = ORIENTED_EDGE ( 'NONE', *, *, #32211, .F. ) ;
#12149 = FACE_OUTER_BOUND ( 'NONE', #21859, .T. ) ;
#12150 = ORIENTED_EDGE ( 'NONE', *, *, #28461, .F. ) ;
#12151 = DIRECTION ( 'NONE',  ( -1.101824276508909887E-16, 1.000000000000000000, -0.000000000000000000 ) ) ;
#12152 = MECHANICAL_DESIGN_GEOMETRIC_PRESENTATION_REPRESENTATION (  '', ( #25252 ), #30508 ) ;
#12153 = DIRECTION ( 'NONE',  ( 0.6797146636928683705, 0.1949050434465285919, 0.7071067811865459074 ) ) ;
#12154 = CARTESIAN_POINT ( 'NONE',  ( -40.68422973805265030, 6.807290781432338456, 34.77612644482307758 ) ) ;
#12155 = TOROIDAL_SURFACE ( 'NONE', #18941, 48.97546517713167447, 2.000000000000000000 ) ;
#12156 = CARTESIAN_POINT ( 'NONE',  ( 48.18662509608405742, 27.19624452788248803, 49.18364984542562013 ) ) ;
#12157 = CARTESIAN_POINT ( 'NONE',  ( -52.00000000000000711, 6.938893903907228378E-15, -3.608224830031758756E-13 ) ) ;
#12158 = ORIENTED_EDGE ( 'NONE', *, *, #14005, .T. ) ;
#12159 = VERTEX_POINT ( 'NONE', #20056 ) ;
#12160 = CARTESIAN_POINT ( 'NONE',  ( 21.09992658989238734, 31.59164230456639544, 47.04930799450051637 ) ) ;
#12161 = DIRECTION ( 'NONE',  ( -0.9612616959383183390, -0.2756373558170014948, -8.795445018805493151E-19 ) ) ;
#12162 = LINE ( 'NONE', #22155, #18803 ) ;
#12163 = ORIENTED_EDGE ( 'NONE', *, *, #12814, .F. ) ;
#12164 = CARTESIAN_POINT ( 'NONE',  ( 45.79384627280941089, 27.16618040159427139, 49.05938063676250493 ) ) ;
#12165 = DIRECTION ( 'NONE',  ( -1.101824276508909887E-16, 1.000000000000000000, -0.000000000000000000 ) ) ;
#12166 = ORIENTED_EDGE ( 'NONE', *, *, #15718, .T. ) ;
#12167 = DIRECTION ( 'NONE',  ( 0.000000000000000000, 1.000000000000000000, 0.000000000000000000 ) ) ;
#12168 = CIRCLE ( 'NONE', #9017, 31.50000000000000711 ) ;
#12169 = FACE_OUTER_BOUND ( 'NONE', #26764, .T. ) ;
#12170 = EDGE_CURVE ( 'NONE', #27545, #12894, #24825, .T. ) ;
#12171 = EDGE_CURVE ( 'NONE', #2697, #2431, #4477, .T. ) ;
#12172 = EDGE_CURVE ( 'NONE', #26169, #26256, #32218, .T. ) ;
#12173 = ADVANCED_FACE ( 'NONE', ( #9887 ), #4633, .F. ) ;
#12174 = AXIS2_PLACEMENT_3D ( 'NONE', #10333, #4921, #17550 ) ;
#12175 = VERTEX_POINT ( 'NONE', #2498 ) ;
#12176 = MANIFOLD_SOLID_BREP ( 'Stock-MAT-060-1', #23142 ) ;
#12177 = AXIS2_PLACEMENT_3D ( 'NONE', #1447, #18836, #23621 ) ;
#12178 = ORIENTED_EDGE ( 'NONE', *, *, #3336, .T. ) ;
#12179 = DIRECTION ( 'NONE',  ( -1.000000000000000000, 0.000000000000000000, 0.000000000000000000 ) ) ;
#12180 = CARTESIAN_POINT ( 'NONE',  ( 48.83862994770794330, 25.24118040159426712, 48.17861352429476796 ) ) ;
#12181 = ORIENTED_EDGE ( 'NONE', *, *, #15677, .F. ) ;
#12182 = CARTESIAN_POINT ( 'NONE',  ( 2.097855976057206639, 13.86454579224779948, 47.04930799450052348 ) ) ;
#12183 = CARTESIAN_POINT ( 'NONE',  ( -40.02540636251514172, 2.839176264122877047, 57.04930799450051637 ) ) ;
#12184 = DIRECTION ( 'NONE',  ( 0.000000000000000000, 0.000000000000000000, -1.000000000000000000 ) ) ;
#12185 = DIRECTION ( 'NONE',  ( -0.03667427209081837447, 0.7071067811865474617, 0.7061550805358612903 ) ) ;
#12186 = CARTESIAN_POINT ( 'NONE',  ( -40.11286833322908052, 2.887657226147511302, 55.74930799450051211 ) ) ;
#12187 = DIRECTION ( 'NONE',  ( -1.101824276508909887E-16, 1.000000000000000000, -0.000000000000000000 ) ) ;
#12188 = DIRECTION ( 'NONE',  ( -1.000000000000000000, 0.000000000000000000, 0.000000000000000000 ) ) ;
#12189 = CARTESIAN_POINT ( 'NONE',  ( 0.6836613156275053171, 11.92558985988973497, -5.803495753465989893 ) ) ;
#12190 = AXIS2_PLACEMENT_3D ( 'NONE', #5772, #26273, #3621 ) ;
#12191 = B_SPLINE_SURFACE_WITH_KNOTS ( 'NONE', 3, 3, ( 
 ( #21138, #13941, #13015, #10386, #20384, #30415 ),
 ( #30579, #23010, #7932, #526, #8526, #10560 ),
 ( #3756, #3593, #18519, #28554, #16064, #26073 ),
 ( #13779, #31815, #24422, #19164, #2103, #26562 ),
 ( #4562, #9172, #4404, #11636, #29525, #14427 ),
 ( #29189, #26726, #1937, #11955, #31979, #6549 ) ),
 .UNSPECIFIED., .F., .F., .F.,
 ( 4, 2, 4 ),
 ( 4, 2, 4 ),
 ( 0.000000000000000000, 0.5000000000000000000, 1.000000000000000000 ),
 ( 0.000000000000000000, 0.5000000000000000000, 1.000000000000000000 ),
 .UNSPECIFIED. ) ;
#12192 = DIRECTION ( 'NONE',  ( 0.000000000000000000, 0.000000000000000000, -1.000000000000000000 ) ) ;
#12193 = AXIS2_PLACEMENT_3D ( 'NONE', #30559, #18538, #834 ) ;
#12194 = VERTEX_POINT ( 'NONE', #21857 ) ;
#12195 = ORIENTED_EDGE ( 'NONE', *, *, #12359, .F. ) ;
#12196 = ADVANCED_FACE ( 'NONE', ( #9399 ), #15292, .T. ) ;
#12197 = DIRECTION ( 'NONE',  ( -0.000000000000000000, -1.000000000000000000, 0.000000000000000000 ) ) ;
#12198 = EDGE_CURVE ( 'NONE', #25211, #21636, #20767, .T. ) ;
#12199 = CARTESIAN_POINT ( 'NONE',  ( 49.77860763202481564, 24.96454579807170404, 45.68180464904889959 ) ) ;
#12200 = TOROIDAL_SURFACE ( 'NONE', #15881, 12.40141737965281621, 0.1249999999999985428 ) ;
#12201 = CARTESIAN_POINT ( 'NONE',  ( 48.59785597605720397, -5.098646251524523443, 47.04930799450052348 ) ) ;
#12202 = CYLINDRICAL_SURFACE ( 'NONE', #27730, 12.36707279061065101 ) ;
#12203 = ORIENTED_EDGE ( 'NONE', *, *, #13246, .T. ) ;
#12204 = CIRCLE ( 'NONE', #9594, 0.1249999999999966416 ) ;
#12205 = CARTESIAN_POINT ( 'NONE',  ( -39.52299075669071016, -5.935454207752198563, 77.87546120947918382 ) ) ;
#12206 = DIRECTION ( 'NONE',  ( -0.9612616959383205595, -0.2756373558169931681, 1.660411357259282445E-16 ) ) ;
#12207 = ORIENTED_EDGE ( 'NONE', *, *, #3296, .F. ) ;
#12208 = VERTEX_POINT ( 'NONE', #19723 ) ;
#12209 = LINE ( 'NONE', #32233, #6313 ) ;
#12210 = CARTESIAN_POINT ( 'NONE',  ( -40.02540636251513462, 2.839176264122873050, 37.04930799450052348 ) ) ;
#12211 = CARTESIAN_POINT ( 'NONE',  ( 7.896202261960366009, 17.36467600858027183, 47.04930799450052348 ) ) ;
#12212 = DIRECTION ( 'NONE',  ( -0.000000000000000000, -1.000000000000000000, 0.000000000000000000 ) ) ;
#12213 = PRODUCT_DEFINITION_SHAPE ( 'NONE', 'NONE',  #32508 ) ;
#12214 = CARTESIAN_POINT ( 'NONE',  ( 21.09992658989238734, 31.09164230456639544, 47.04930799450051637 ) ) ;
#12215 = ORIENTED_EDGE ( 'NONE', *, *, #4903, .T. ) ;
#12216 = EDGE_CURVE ( 'NONE', #28526, #14460, #2669, .T. ) ;
#12217 = ORIENTED_EDGE ( 'NONE', *, *, #16733, .T. ) ;
#12218 = CIRCLE ( 'NONE', #19531, 12.36707279061065101 ) ;
#12219 = CIRCLE ( 'NONE', #17458, 55.87116166729571631 ) ;
#12220 = CARTESIAN_POINT ( 'NONE',  ( 21.09785597605720042, -14.03534765547855656, 47.04930799450051637 ) ) ;
#12221 = EDGE_LOOP ( 'NONE', ( #10317, #5682, #28362, #24549 ) ) ;
#12222 = CIRCLE ( 'NONE', #26882, 0.1249999999999983763 ) ;
#12223 = CIRCLE ( 'NONE', #22168, 12.98419020052702599 ) ;
#12224 = EDGE_CURVE ( 'NONE', #13560, #9356, #13007, .T. ) ;
#12225 = DIRECTION ( 'NONE',  ( -1.000000000000000000, 0.000000000000000000, 0.000000000000000000 ) ) ;
#12226 = CARTESIAN_POINT ( 'NONE',  ( 33.46699938050304013, 24.97145308207319303, 47.04930799450050927 ) ) ;
#12227 = ADVANCED_FACE ( 'NONE', ( #20861 ), #6838, .F. ) ;
#12228 = EDGE_LOOP ( 'NONE', ( #7559, #27407, #9036, #1470 ) ) ;
#12229 = DIRECTION ( 'NONE',  ( -1.000000000000000000, 0.000000000000000000, 0.000000000000000000 ) ) ;
#12230 = ORIENTED_EDGE ( 'NONE', *, *, #15620, .T. ) ;
#12231 = DIRECTION ( 'NONE',  ( -1.101824276508909887E-16, 1.000000000000000000, -0.000000000000000000 ) ) ;
#12232 = DIRECTION ( 'NONE',  ( 0.000000000000000000, 0.000000000000000000, 1.000000000000000000 ) ) ;
#12233 = DIRECTION ( 'NONE',  ( 0.000000000000000000, 1.000000000000000000, 0.000000000000000000 ) ) ;
#12234 = ORIENTED_EDGE ( 'NONE', *, *, #10244, .F. ) ;
#12235 = EDGE_CURVE ( 'NONE', #19419, #7551, #16801, .T. ) ;
#12236 = DIRECTION ( 'NONE',  ( 0.4848096202463673676, 0.8746197071393789768, 0.000000000000000000 ) ) ;
#12237 = DIRECTION ( 'NONE',  ( 0.000000000000000000, 0.000000000000000000, -1.000000000000000000 ) ) ;
#12238 = CARTESIAN_POINT ( 'NONE',  ( 8.698509210239539158, 27.34164230456639544, 47.04930799450051637 ) ) ;
#12239 = ADVANCED_FACE ( 'NONE', ( #10375 ), #5129, .F. ) ;
#12240 = DIRECTION ( 'NONE',  ( -1.101824276508909887E-16, 1.000000000000000000, -0.000000000000000000 ) ) ;
#12241 = EDGE_CURVE ( 'NONE', #29156, #5398, #25147, .T. ) ;
#12242 = CIRCLE ( 'NONE', #29001, 12.62506659569710266 ) ;
#12243 = DIRECTION ( 'NONE',  ( -2.946248497964555786E-19, -3.001156285468303092E-19, -1.000000000000000000 ) ) ;
#12244 = EDGE_LOOP ( 'NONE', ( #4364, #26318, #23262, #9938 ) ) ;
#12245 = DIRECTION ( 'NONE',  ( -1.000000000000000000, 0.000000000000000000, 0.000000000000000000 ) ) ;
#12246 = CARTESIAN_POINT ( 'NONE',  ( 21.09785597605719332, 24.86454579224780304, 47.04930799450051637 ) ) ;
#12247 = VECTOR ( 'NONE', #32451, 1000.000000000000000 ) ;
#12248 = ORIENTED_EDGE ( 'NONE', *, *, #26162, .T. ) ;
#12249 = DIRECTION ( 'NONE',  ( -1.101824276508909887E-16, 1.000000000000000000, -0.000000000000000000 ) ) ;
#12250 = LINE ( 'NONE', #12415, #176 ) ;
#12251 = AXIS2_PLACEMENT_3D ( 'NONE', #30455, #25199, #10110 ) ;
#12252 = ORIENTED_EDGE ( 'NONE', *, *, #31675, .T. ) ;
#12253 = CIRCLE ( 'NONE', #22711, 12.27641737965280555 ) ;
#12254 =( BOUNDED_CURVE ( )  B_SPLINE_CURVE ( 3, ( #29, #27441, #15131, #4957 ),
 .UNSPECIFIED., .F., .F. ) 
 B_SPLINE_CURVE_WITH_KNOTS ( ( 4, 4 ),
 ( 2.992702705980254230, 4.414609085165686508 ),
 .UNSPECIFIED. ) 
 CURVE ( )  GEOMETRIC_REPRESENTATION_ITEM ( )  RATIONAL_B_SPLINE_CURVE ( ( 1.000000000000000000, 0.8384934736035498659, 0.8384934736035498659, 1.000000000000000000 ) ) 
 REPRESENTATION_ITEM ( '' )  );
#12255 = CIRCLE ( 'NONE', #30597, 1.499999999999998668 ) ;
#12256 = ORIENTED_EDGE ( 'NONE', *, *, #24446, .F. ) ;
#12257 = EDGE_CURVE ( 'NONE', #30366, #23695, #25786, .T. ) ;
#12258 = ORIENTED_EDGE ( 'NONE', *, *, #3982, .T. ) ;
#12259 = CIRCLE ( 'NONE', #3860, 47.05803085792211249 ) ;
#12260 = EDGE_CURVE ( 'NONE', #26491, #18864, #15763, .T. ) ;
#12261 = DIRECTION ( 'NONE',  ( 0.000000000000000000, 0.000000000000000000, 1.000000000000000000 ) ) ;
#12262 = EDGE_CURVE ( 'NONE', #3764, #6409, #30983, .T. ) ;
#12263 = ORIENTED_EDGE ( 'NONE', *, *, #27843, .F. ) ;
#12264 = ORIENTED_EDGE ( 'NONE', *, *, #6999, .F. ) ;
#12265 = CARTESIAN_POINT ( 'NONE',  ( 78.48781352222600560, -5.738638231773887100, 15.17031821407819514 ) ) ;
#12266 = CIRCLE ( 'NONE', #8079, 1.500000000000001332 ) ;
#12267 = DIRECTION ( 'NONE',  ( -1.101824276508909887E-16, 1.000000000000000000, -0.000000000000000000 ) ) ;
#12268 = DIRECTION ( 'NONE',  ( 1.234978253042719660E-16, -1.000000000000000000, -1.109335647967047851E-31 ) ) ;
#12269 = CARTESIAN_POINT ( 'NONE',  ( 21.09992658989239089, 25.59184655352419213, 47.04930799450051637 ) ) ;
#12270 = EDGE_LOOP ( 'NONE', ( #23823, #1502, #14657, #8541 ) ) ;
#12271 = CARTESIAN_POINT ( 'NONE',  ( -8.808741845175550367, 6.094407115496628613, 98.01272063432647030 ) ) ;
#12272 = ORIENTED_EDGE ( 'NONE', *, *, #9759, .T. ) ;
#12273 = CARTESIAN_POINT ( 'NONE',  ( -30.40389907987879070, 7.914959306551518026, 18.50712902613415167 ) ) ;
#12274 = PLANE ( 'NONE',  #32114 ) ;
#12275 = EDGE_CURVE ( 'NONE', #27738, #22606, #26773, .T. ) ;
#12276 = VERTEX_POINT ( 'NONE', #28104 ) ;
#12277 = DIRECTION ( 'NONE',  ( -1.000000000000000000, 0.000000000000000000, 0.000000000000000000 ) ) ;
#12278 = CARTESIAN_POINT ( 'NONE',  ( -43.64647580959332629, 1.256990871545142774, 60.44930799450051495 ) ) ;
#12279 = CARTESIAN_POINT ( 'NONE',  ( 52.10136161249906195, -5.936382080411357620, 107.6680807723975164 ) ) ;
#12280 = DIRECTION ( 'NONE',  ( -0.000000000000000000, -0.000000000000000000, 1.000000000000000000 ) ) ;
#12281 = DIRECTION ( 'NONE',  ( -1.000000000000000000, 0.000000000000000000, 0.000000000000000000 ) ) ;
#12282 = CARTESIAN_POINT ( 'NONE',  ( 47.20547626766766314, 28.18791119454915162, 44.97710074790751378 ) ) ;
#12283 = CARTESIAN_POINT ( 'NONE',  ( -41.94956971822180947, 3.905757428664828890, 47.04930799450051637 ) ) ;
#12284 = CARTESIAN_POINT ( 'NONE',  ( -40.66586793973302605, 8.138261812237590931, 54.59072935073782418 ) ) ;
#12285 = ORIENTED_EDGE ( 'NONE', *, *, #16232, .F. ) ;
#12286 = CARTESIAN_POINT ( 'NONE',  ( 47.13718051761725292, 29.59454644216853936, 44.97967791668052229 ) ) ;
#12287 = CARTESIAN_POINT ( 'NONE',  ( 33.46699938050304013, 38.56284415653841791, 47.04930799450051637 ) ) ;
#12288 = ORIENTED_EDGE ( 'NONE', *, *, #19979, .T. ) ;
#12289 = CARTESIAN_POINT ( 'NONE',  ( 21.09992658989238734, 30.71664230456641675, 47.04930799450051637 ) ) ;
#12290 = CARTESIAN_POINT ( 'NONE',  ( -40.05987053574653345, 7.506472619680472746, 38.44930799450052916 ) ) ;
#12291 = VERTEX_POINT ( 'NONE', #20701 ) ;
#12292 = AXIS2_PLACEMENT_3D ( 'NONE', #380, #15639, #10576 ) ;
#12293 = EDGE_LOOP ( 'NONE', ( #12662, #29775 ) ) ;
#12294 = CIRCLE ( 'NONE', #30127, 12.36707279061065279 ) ;
#12295 = AXIS2_PLACEMENT_3D ( 'NONE', #17414, #2647, #22664 ) ;
#12296 = ORIENTED_EDGE ( 'NONE', *, *, #21810, .F. ) ;
#12297 = EDGE_LOOP ( 'NONE', ( #2065, #3610, #8650, #31467 ) ) ;
#12298 = DIRECTION ( 'NONE',  ( -1.044582700994767690E-16, 0.5219656503457801300, 0.8529665057076430967 ) ) ;
#12299 = DIRECTION ( 'NONE',  ( -1.101824276508909887E-16, 1.000000000000000000, -0.000000000000000000 ) ) ;
#12300 = VERTEX_POINT ( 'NONE', #10218 ) ;
#12301 = CIRCLE ( 'NONE', #12856, 0.1250000000000001110 ) ;
#12302 = FACE_OUTER_BOUND ( 'NONE', #31221, .T. ) ;
#12303 = CARTESIAN_POINT ( 'NONE',  ( 21.09992658989238734, 38.56284415653841791, 47.04930799450051637 ) ) ;
#12304 = DIRECTION ( 'NONE',  ( -1.101824276508909887E-16, 1.000000000000000000, -0.000000000000000000 ) ) ;
#12305 = CIRCLE ( 'NONE', #20666, 1.300000000000002487 ) ;
#12306 = CARTESIAN_POINT ( 'NONE',  ( 48.83862994770794330, 25.85457786121582302, 48.17861352429476796 ) ) ;
#12307 = VERTEX_POINT ( 'NONE', #30403 ) ;
#12308 = VERTEX_POINT ( 'NONE', #23169 ) ;
#12310 = CARTESIAN_POINT ( 'NONE',  ( 21.09785597605720042, -16.03545420775219910, 47.04930799450051637 ) ) ;
#12309 = AXIS2_PLACEMENT_3D ( 'NONE', #28176, #23080, #27684 ) ;
#12311 = CIRCLE ( 'NONE', #30148, 0.09999999999999714673 ) ;
#12312 = ADVANCED_FACE ( 'NONE', ( #25313 ), #24118, .T. ) ;
#12313 = VERTEX_POINT ( 'NONE', #8007 ) ;
#12314 = CARTESIAN_POINT ( 'NONE',  ( 67.09652168471781408, 13.80129159329807287, 47.04930799450051637 ) ) ;
#12315 = AXIS2_PLACEMENT_3D ( 'NONE', #21117, #25740, #944 ) ;
#12316 = CARTESIAN_POINT ( 'NONE',  ( -40.90015969217747482, 8.955334253785162346, 57.95249952744806166 ) ) ;
#12317 = FACE_OUTER_BOUND ( 'NONE', #24784, .T. ) ;
#12318 = EDGE_CURVE ( 'NONE', #29739, #15228, #7899, .T. ) ;
#12319 = DIRECTION ( 'NONE',  ( 0.000000000000000000, -1.000000000000000000, 0.000000000000000000 ) ) ;
#12320 = CARTESIAN_POINT ( 'NONE',  ( 46.99023568444673060, 29.23791119454914877, 49.12151524109405898 ) ) ;
#12321 = SHAPE_DEFINITION_REPRESENTATION ( #26588, #12446 ) ;
#12322 = ORIENTED_EDGE ( 'NONE', *, *, #14053, .F. ) ;
#12323 = EDGE_LOOP ( 'NONE', ( #19870, #26914, #8942, #24541 ) ) ;
#12324 = DIRECTION ( 'NONE',  ( -1.000000000000000000, 0.000000000000000000, 0.000000000000000000 ) ) ;
#12325 = DIRECTION ( 'NONE',  ( -1.000000000000000000, -1.101824276508909887E-16, 0.000000000000000000 ) ) ;
#12326 = B_SPLINE_CURVE_WITH_KNOTS ( 'NONE', 3,
 ( #19181, #11821, #29209, #6722, #1798, #20491 ),
 .UNSPECIFIED., .F., .F.,
 ( 4, 2, 4 ),
 ( 0.000000000000000000, 0.5000000000000000000, 1.000000000000000000 ),
 .UNSPECIFIED. ) ;
#12327 = CARTESIAN_POINT ( 'NONE',  ( -40.98031486389898248, 9.265261353013489298, 39.54930799450052348 ) ) ;
#12328 = EDGE_LOOP ( 'NONE', ( #26659, #16354, #19937, #23781 ) ) ;
#12329 = CARTESIAN_POINT ( 'NONE',  ( 48.18662509608405031, 29.38284706826092574, 49.18364984542562013 ) ) ;
#12330 = DIRECTION ( 'NONE',  ( -1.224646799147353207E-16, -1.349345573449484691E-32, 1.000000000000000000 ) ) ;
#12331 = EDGE_LOOP ( 'NONE', ( #13309, #23660, #7072, #9843 ) ) ;
#12332 = CYLINDRICAL_SURFACE ( 'NONE', #11485, 12.62506659569710266 ) ;
#12333 = CARTESIAN_POINT ( 'NONE',  ( 45.73035263060504718, 26.53954579807170688, 44.36855633853329550 ) ) ;
#12334 = DIRECTION ( 'NONE',  ( -0.1299938060159217812, 0.9915148059396262648, 1.313546309486176444E-17 ) ) ;
#12335 = AXIS2_PLACEMENT_3D ( 'NONE', #14927, #7385, #21969 ) ;
#12336 = CIRCLE ( 'NONE', #7077, 46.67448298906162307 ) ;
#12337 = AXIS2_PLACEMENT_3D ( 'NONE', #11901, #29632, #19269 ) ;
#12338 = AXIS2_PLACEMENT_3D ( 'NONE', #22385, #29295, #6812 ) ;
#12339 = CIRCLE ( 'NONE', #3423, 40.00000000000000711 ) ;
#12340 = ORIENTED_EDGE ( 'NONE', *, *, #1291, .T. ) ;
#12341 = VERTEX_POINT ( 'NONE', #13570 ) ;
#12342 = FACE_OUTER_BOUND ( 'NONE', #25053, .T. ) ;
#12343 = CARTESIAN_POINT ( 'NONE',  ( 72.77125109260951774, 11.18949478403749787, 71.27148623857269172 ) ) ;
#12344 = CARTESIAN_POINT ( 'NONE',  ( 21.09785597605719332, 25.76454579224779806, 34.04930799450050927 ) ) ;
#12345 = VERTEX_POINT ( 'NONE', #924 ) ;
#12346 = DIRECTION ( 'NONE',  ( 8.659560562354919300E-17, 0.7071067811865487940, -0.7071067811865463515 ) ) ;
#12347 = DIRECTION ( 'NONE',  ( -0.000000000000000000, -1.000000000000000000, -0.000000000000000000 ) ) ;
#12348 = CARTESIAN_POINT ( 'NONE',  ( 51.47386758732231016, 5.370505999354205251, -4.102960719301439241 ) ) ;
#12349 = EDGE_CURVE ( 'NONE', #21924, #30824, #18884, .T. ) ;
#12350 = CARTESIAN_POINT ( 'NONE',  ( 21.09992658989238734, 38.56284415653841791, 47.04930799450051637 ) ) ;
#12351 = DIRECTION ( 'NONE',  ( -1.224646799147353207E-16, -1.349345573449484691E-32, 1.000000000000000000 ) ) ;
#12352 = CARTESIAN_POINT ( 'NONE',  ( 33.37634396954523908, 27.59164230456639544, 47.04930799450051637 ) ) ;
#12353 = ADVANCED_FACE ( 'NONE', ( #3228 ), #28023, .T. ) ;
#12354 = DIRECTION ( 'NONE',  ( -0.000000000000000000, -1.000000000000000000, 0.000000000000000000 ) ) ;
#12356 = EDGE_CURVE ( 'NONE', #18631, #15214, #19951, .T. ) ;
#12355 = DIRECTION ( 'NONE',  ( 0.05186525298100497228, 2.168404344971009115E-16, -0.9986540920324796788 ) ) ;
#12357 = CIRCLE ( 'NONE', #28077, 94.94530576803560962 ) ;
#12358 = EDGE_CURVE ( 'NONE', #21770, #31503, #15542, .T. ) ;
#12359 = EDGE_CURVE ( 'NONE', #14096, #25267, #31996, .T. ) ;
#12360 = CARTESIAN_POINT ( 'NONE',  ( -40.50410981870283678, 7.604537000166496696, 35.33853321918559232 ) ) ;
#12361 = EDGE_CURVE ( 'NONE', #25372, #21089, #3058, .T. ) ;
#12362 = ORIENTED_EDGE ( 'NONE', *, *, #28119, .F. ) ;
#12363 = ORIENTED_EDGE ( 'NONE', *, *, #22531, .T. ) ;
#12364 = DIRECTION ( 'NONE',  ( 0.000000000000000000, 0.000000000000000000, -1.000000000000000000 ) ) ;
#12365 = VECTOR ( 'NONE', #18587, 1000.000000000000000 ) ;
#12366 = MECHANICAL_DESIGN_GEOMETRIC_PRESENTATION_REPRESENTATION (  '', ( #6075 ), #27557 ) ;
#12367 = DIRECTION ( 'NONE',  ( 0.2756373558169954441, -0.9612616959383198934, 1.479773560108263451E-16 ) ) ;
#12368 = CARTESIAN_POINT ( 'NONE',  ( -40.16409007829387434, 6.927803014773068035, 34.54930799450055190 ) ) ;
#12369 = VECTOR ( 'NONE', #28605, 1000.000000000000000 ) ;
#12370 = CARTESIAN_POINT ( 'NONE',  ( 52.27789684966019479, -5.944439029104267469, 104.9516812706435758 ) ) ;
#12371 = ORIENTED_EDGE ( 'NONE', *, *, #10469, .F. ) ;
#12372 = DIRECTION ( 'NONE',  ( -1.224646799147353207E-16, 0.000000000000000000, -1.000000000000000000 ) ) ;
#12373 = LINE ( 'NONE', #17765, #11642 ) ;
#12374 = DIRECTION ( 'NONE',  ( -0.2756373558169926130, 0.9612616959383206705, 3.682857393832930037E-14 ) ) ;
#12375 = ORIENTED_EDGE ( 'NONE', *, *, #24233, .F. ) ;
#12376 = ORIENTED_EDGE ( 'NONE', *, *, #14166, .T. ) ;
#12377 = CARTESIAN_POINT ( 'NONE',  ( -40.02540636251513462, 2.839176264122873050, 37.04930799450052348 ) ) ;
#12378 = CARTESIAN_POINT ( 'NONE',  ( 48.83862994770794330, 29.44118040159425931, 48.17861352429476796 ) ) ;
#12379 = DIRECTION ( 'NONE',  ( -1.000000000000000000, 0.000000000000000000, 0.000000000000000000 ) ) ;
#12380 = TOROIDAL_SURFACE ( 'NONE', #15001, 12.78419020052701960, 0.2000000000000000944 ) ;
#12381 = CARTESIAN_POINT ( 'NONE',  ( -40.71297758125562183, 7.970149924291493271, 39.96793714460204683 ) ) ;
#12382 = CARTESIAN_POINT ( 'NONE',  ( 45.73517587035135534, 29.24587785034128373, 45.04535568177062288 ) ) ;
#12383 = ORIENTED_EDGE ( 'NONE', *, *, #15247, .F. ) ;
#12384 = VERTEX_POINT ( 'NONE', #20945 ) ;
#12385 = DIRECTION ( 'NONE',  ( 0.000000000000000000, 3.756723415560144304E-15, -1.000000000000000000 ) ) ;
#12386 = EDGE_CURVE ( 'NONE', #21830, #1812, #10639, .T. ) ;
#12387 = AXIS2_PLACEMENT_3D ( 'NONE', #9855, #17716, #17227 ) ;
#12388 =( GEOMETRIC_REPRESENTATION_CONTEXT ( 3 ) GLOBAL_UNCERTAINTY_ASSIGNED_CONTEXT ( ( #21915 ) ) GLOBAL_UNIT_ASSIGNED_CONTEXT ( ( #18546, #23332, #15940 ) ) REPRESENTATION_CONTEXT ( 'NONE', 'WORKASPACE' ) );
#12389 = EDGE_LOOP ( 'NONE', ( #31634, #19657, #21639, #28280 ) ) ;
#12390 = FACE_OUTER_BOUND ( 'NONE', #5309, .T. ) ;
#12391 = DIRECTION ( 'NONE',  ( 0.000000000000000000, -1.000000000000000000, 0.000000000000000000 ) ) ;
#12392 = TOROIDAL_SURFACE ( 'NONE', #31251, 12.40141737965284463, 0.1250000000000005274 ) ;
#12393 = VERTEX_POINT ( 'NONE', #20630 ) ;
#12394 = CARTESIAN_POINT ( 'NONE',  ( 21.09992658989238734, 32.34164230456639899, 47.04930799450051637 ) ) ;
#12395 = ORIENTED_EDGE ( 'NONE', *, *, #8269, .T. ) ;
#12396 = MANIFOLD_SOLID_BREP ( 'Stock-MAT-060-1', #32042 ) ;
#12397 = DIRECTION ( 'NONE',  ( 1.000000000000000000, 0.000000000000000000, 1.224646799147353207E-16 ) ) ;
#12398 = EDGE_CURVE ( 'NONE', #9796, #1812, #5064, .T. ) ;
#12399 = CARTESIAN_POINT ( 'NONE',  ( 21.09992658989238734, 31.84164230456639544, 47.04930799450051637 ) ) ;
#12400 = EDGE_CURVE ( 'NONE', #26705, #26305, #12093, .T. ) ;
#12401 = DIRECTION ( 'NONE',  ( -1.000000000000000000, 0.000000000000000000, 0.000000000000000000 ) ) ;
#12402 = ORIENTED_EDGE ( 'NONE', *, *, #19585, .F. ) ;
#12403 = CARTESIAN_POINT ( 'NONE',  ( 74.89817579486182808, -1.820484904611762156, 80.73796779739511464 ) ) ;
#12404 = CARTESIAN_POINT ( 'NONE',  ( 33.72499318558949710, 24.84184655352419213, 47.04930799450051637 ) ) ;
#12405 = CARTESIAN_POINT ( 'NONE',  ( -31.75494777190936802, 11.92558985988973674, 26.63511333407100778 ) ) ;
#12406 = DIRECTION ( 'NONE',  ( 0.000000000000000000, 0.000000000000000000, 1.000000000000000000 ) ) ;
#12407 = CARTESIAN_POINT ( 'NONE',  ( 8.823509210239539158, 27.34164230456639544, 47.04930799450051637 ) ) ;
#12408 = ORIENTED_EDGE ( 'NONE', *, *, #4753, .F. ) ;
#12409 = CARTESIAN_POINT ( 'NONE',  ( -40.02540636251513462, 2.839176264122873050, 37.04930799450052348 ) ) ;
#12410 = CARTESIAN_POINT ( 'NONE',  ( 33.72499318558949710, 29.59184655352418858, 47.04930799450051637 ) ) ;
#12411 = ORIENTED_EDGE ( 'NONE', *, *, #7120, .F. ) ;
#12412 = CARTESIAN_POINT ( 'NONE',  ( -42.38687957179150345, 4.148162238788003719, 55.74930799450051211 ) ) ;
#12413 = AXIS2_PLACEMENT_3D ( 'NONE', #2468, #9696, #20022 ) ;
#12414 = DIRECTION ( 'NONE',  ( -1.000000000000000000, 0.000000000000000000, 0.000000000000000000 ) ) ;
#12415 = CARTESIAN_POINT ( 'NONE',  ( 46.27249149607015966, 23.24793988701932079, 46.54352925064344504 ) ) ;
#12416 = EDGE_LOOP ( 'NONE', ( #20682, #13411, #24851 ) ) ;
#12417 = VERTEX_POINT ( 'NONE', #1731 ) ;
#12418 = EDGE_CURVE ( 'NONE', #13126, #25102, #7382, .T. ) ;
#12419 = CIRCLE ( 'NONE', #29700, 12.27641737965286062 ) ;
#12420 = ORIENTED_EDGE ( 'NONE', *, *, #9116, .T. ) ;
#12421 = EDGE_CURVE ( 'NONE', #9009, #6807, #25210, .T. ) ;
#12422 = ADVANCED_FACE ( 'NONE', ( #1892 ), #3687, .T. ) ;
#12423 = DIRECTION ( 'NONE',  ( -1.224646799147353207E-16, -1.349345573449484691E-32, 1.000000000000000000 ) ) ;
#12424 = AXIS2_PLACEMENT_3D ( 'NONE', #16942, #19732, #14665 ) ;
#12425 = B_SPLINE_CURVE_WITH_KNOTS ( 'NONE', 3,
 ( #2426, #30804, #2903, #279, #8317, #17838, #3383, #18154, #13416, #18314, #3224, #5869 ),
 .UNSPECIFIED., .F., .F.,
 ( 4, 2, 2, 2, 2, 4 ),
 ( 0.0001999864807696098657, 0.001053893586900949038, 0.001480847139966614233, 0.001907800693032279428, 0.002761707799163610252, 0.003615614905294941075 ),
 .UNSPECIFIED. ) ;
#12426 = ORIENTED_EDGE ( 'NONE', *, *, #26795, .F. ) ;
#12427 = ORIENTED_EDGE ( 'NONE', *, *, #23159, .T. ) ;
#12428 = DIRECTION ( 'NONE',  ( -0.000000000000000000, -1.000000000000000000, 0.000000000000000000 ) ) ;
#12429 = CARTESIAN_POINT ( 'NONE',  ( -38.37328487235789964, 6.954148266671692724, 32.09930799450052064 ) ) ;
#12430 = DIRECTION ( 'NONE',  ( -0.4848096202463636484, -0.8746197071393810862, 0.000000000000000000 ) ) ;
#12431 = CARTESIAN_POINT ( 'NONE',  ( 44.79156314060809763, 22.86454579224779948, 46.92953032342012420 ) ) ;
#12432 = LINE ( 'NONE', #2569, #28357 ) ;
#12433 = EDGE_CURVE ( 'NONE', #15228, #29739, #29371, .T. ) ;
#12434 = ORIENTED_EDGE ( 'NONE', *, *, #26982, .F. ) ;
#12435 = CARTESIAN_POINT ( 'NONE',  ( -10.97128175978245324, -5.614579432636300993, 104.2544310257684117 ) ) ;
#12436 = ORIENTED_EDGE ( 'NONE', *, *, #24115, .F. ) ;
#12437 = CARTESIAN_POINT ( 'NONE',  ( -37.21204910874187988, -5.721341737285086992, 15.20211895544695757 ) ) ;
#12438 = DIRECTION ( 'NONE',  ( 0.4848096202463673121, 0.8746197071393789768, 0.000000000000000000 ) ) ;
#12439 = ORIENTED_EDGE ( 'NONE', *, *, #10733, .T. ) ;
#12440 = CARTESIAN_POINT ( 'NONE',  ( 8.698509210239574685, 30.59164230456639544, 47.04930799450051637 ) ) ;
#12441 = DIRECTION ( 'NONE',  ( 0.7141240004913198547, -0.3958453973320100738, -0.5773502691896283956 ) ) ;
#12442 = FACE_OUTER_BOUND ( 'NONE', #1861, .T. ) ;
#12443 = DIRECTION ( 'NONE',  ( -1.101824276508909887E-16, 1.000000000000000000, -0.000000000000000000 ) ) ;
#12444 = DIRECTION ( 'NONE',  ( -0.000000000000000000, -0.000000000000000000, 1.000000000000000000 ) ) ;
#12445 = CARTESIAN_POINT ( 'NONE',  ( 44.70507715278255745, 26.96291119454915730, 46.92503878583765697 ) ) ;
#12446 = SHAPE_REPRESENTATION ( 'Magnet', ( #8172 ), #9736 ) ;
#12447 = DIRECTION ( 'NONE',  ( 1.431146867680865853E-17, 2.558717127065790464E-17, 1.000000000000000000 ) ) ;
#12448 = DIRECTION ( 'NONE',  ( -0.000000000000000000, 1.000000000000000000, -0.000000000000000000 ) ) ;
#12449 = ORIENTED_EDGE ( 'NONE', *, *, #4819, .F. ) ;
#12450 = LINE ( 'NONE', #27206, #31305 ) ;
#12451 = DIRECTION ( 'NONE',  ( -1.000000000000000000, 0.000000000000000000, 0.000000000000000000 ) ) ;
#12452 = ORIENTED_EDGE ( 'NONE', *, *, #22709, .T. ) ;
#12453 = DIRECTION ( 'NONE',  ( -1.000000000000000000, 0.000000000000000000, 0.000000000000000000 ) ) ;
#12454 = MANIFOLD_SOLID_BREP ( 'Stock-MAT-060-1', #11608 ) ;
#12455 = ORIENTED_EDGE ( 'NONE', *, *, #5071, .F. ) ;
#12456 = EDGE_CURVE ( 'NONE', #21280, #2467, #10003, .T. ) ;
#12457 = ORIENTED_EDGE ( 'NONE', *, *, #27637, .T. ) ;
#12458 = LINE ( 'NONE', #27709, #4697 ) ;
#12459 = AXIS2_PLACEMENT_3D ( 'NONE', #9899, #32384, #53 ) ;
#12460 = EDGE_CURVE ( 'NONE', #20710, #19617, #8958, .T. ) ;
#12461 = B_SPLINE_CURVE_WITH_KNOTS ( 'NONE', 3,
 ( #4035, #22074, #19117, #21586 ),
 .UNSPECIFIED., .F., .F.,
 ( 4, 4 ),
 ( 0.000000000000000000, 1.000000000000000000 ),
 .UNSPECIFIED. ) ;
#12462 = ORIENTED_EDGE ( 'NONE', *, *, #18153, .F. ) ;
#12463 = VECTOR ( 'NONE', #20585, 1000.000000000000000 ) ;
#12464 = ADVANCED_FACE ( 'NONE', ( #28987 ), #26520, .F. ) ;
#12465 = EDGE_CURVE ( 'NONE', #1073, #29330, #24143, .T. ) ;
#12466 = ORIENTED_EDGE ( 'NONE', *, *, #29988, .F. ) ;
#12467 = CARTESIAN_POINT ( 'NONE',  ( 46.81682104422132085, 23.12036939723557083, 47.03471240234085116 ) ) ;
#12468 = CARTESIAN_POINT ( 'NONE',  ( 79.40776106085759523, -5.721341737285999152, 78.89649703355206611 ) ) ;
#12469 = ORIENTED_EDGE ( 'NONE', *, *, #10988, .T. ) ;
#12470 = DIRECTION ( 'NONE',  ( 0.000000000000000000, 0.000000000000000000, -1.000000000000000000 ) ) ;
#12471 = DIRECTION ( 'NONE',  ( -0.4848096202463430537, -0.8746197071393926326, -9.920727850371701658E-18 ) ) ;
#12472 = DIRECTION ( 'NONE',  ( -1.224646799147353207E-16, -1.349345573449484691E-32, 1.000000000000000000 ) ) ;
#12473 = CARTESIAN_POINT ( 'NONE',  ( 45.24946171279598417, 24.92124452788249300, 47.99220971130007030 ) ) ;
#12474 = ORIENTED_EDGE ( 'NONE', *, *, #6526, .F. ) ;
#12475 = AXIS2_PLACEMENT_3D ( 'NONE', #3759, #13944, #1450 ) ;
#12476 = VERTEX_POINT ( 'NONE', #9451 ) ;
#12477 = DIRECTION ( 'NONE',  ( -1.000000000000000000, 0.000000000000000000, 0.000000000000000000 ) ) ;
#12478 = AXIS2_PLACEMENT_3D ( 'NONE', #5741, #13304, #5907 ) ;
#12479 = ORIENTED_EDGE ( 'NONE', *, *, #20835, .T. ) ;
#12480 = DIRECTION ( 'NONE',  ( 0.000000000000000000, 0.000000000000000000, 1.000000000000000000 ) ) ;
#12481 = CARTESIAN_POINT ( 'NONE',  ( 21.09992658989239089, 30.59164230456639544, 47.04930799450051637 ) ) ;
#12482 = LINE ( 'NONE', #29712, #23711 ) ;
#12483 = AXIS2_PLACEMENT_3D ( 'NONE', #15071, #19986, #4560 ) ;
#12484 = CARTESIAN_POINT ( 'NONE',  ( 52.06562842487888787, -5.940946157296536967, -12.59682317512997685 ) ) ;
#12485 = DIRECTION ( 'NONE',  ( 0.000000000000000000, 0.000000000000000000, 1.000000000000000000 ) ) ;
#12486 = PRODUCT_CONTEXT ( 'NONE', #30906, 'mechanical' ) ;
#12487 = VERTEX_POINT ( 'NONE', #1563 ) ;
#12488 = ORIENTED_EDGE ( 'NONE', *, *, #32399, .T. ) ;
#12489 = DIRECTION ( 'NONE',  ( -0.3428121700606640565, -0.6184495258776567805, 0.7071067811865474617 ) ) ;
#12490 = B_SPLINE_CURVE_WITH_KNOTS ( 'NONE', 3,
 ( #10381, #205, #12528, #25477, #4972, #7927, #17758, #17599, #5615, #27611, #15144, #10223, #20546, #3136, #24992, #20221 ),
 .UNSPECIFIED., .F., .F.,
 ( 4, 2, 2, 2, 2, 2, 2, 4 ),
 ( 0.000000000000000000, 0.0002419933622418494166, 0.0004839867244836988333, 0.0009679734489673894266, 0.001451960173451080074, 0.001935946897934770830, 0.002903920346902169689, 0.003871893795869568982 ),
 .UNSPECIFIED. ) ;
#12491 = CARTESIAN_POINT ( 'NONE',  ( 7.596071960694295910, 17.16474120167318063, 47.04930799450052348 ) ) ;
#12492 = CIRCLE ( 'NONE', #24510, 12.27641737965287305 ) ;
#12493 = DIRECTION ( 'NONE',  ( -1.101824276508909887E-16, 1.000000000000000000, -0.000000000000000000 ) ) ;
#12494 = ORIENTED_EDGE ( 'NONE', *, *, #25601, .F. ) ;
#12495 = CARTESIAN_POINT ( 'NONE',  ( 45.24946171279598417, 28.50784706826092929, 47.99220971130007030 ) ) ;
#12496 = ADVANCED_FACE ( 'NONE', ( #6660 ), #27499, .T. ) ;
#12497 = VERTEX_POINT ( 'NONE', #25196 ) ;
#12498 = CARTESIAN_POINT ( 'NONE',  ( 21.09785597605719332, 16.86454579224779948, 47.04930799450051637 ) ) ;
#12499 = CARTESIAN_POINT ( 'NONE',  ( 48.35473289974373756, 19.96454579224779380, 45.11188864597615833 ) ) ;
#12500 = EDGE_CURVE ( 'NONE', #4462, #180, #7644, .T. ) ;
#12501 = DIRECTION ( 'NONE',  ( 0.000000000000000000, 1.000000000000000000, -0.000000000000000000 ) ) ;
#12502 = AXIS2_PLACEMENT_3D ( 'NONE', #21037, #13510, #8894 ) ;
#12503 = TOROIDAL_SURFACE ( 'NONE', #13526, 12.40141737965288904, 0.1249999999999998612 ) ;
#12504 = ADVANCED_FACE ( 'NONE', ( #4850 ), #24160, .F. ) ;
#12505 = EDGE_LOOP ( 'NONE', ( #1933, #9989, #18682, #21118 ) ) ;
#12506 = ADVANCED_FACE ( 'NONE', ( #2390 ), #5844, .T. ) ;
#12507 = CIRCLE ( 'NONE', #1987, 12.00000000000000355 ) ;
#12508 = TOROIDAL_SURFACE ( 'NONE', #2019, 12.61792373059896200, 0.1249999999999979183 ) ;
#12509 = ORIENTED_EDGE ( 'NONE', *, *, #11167, .F. ) ;
#12510 = LINE ( 'NONE', #24808, #17534 ) ;
#12511 = CARTESIAN_POINT ( 'NONE',  ( 21.09785597605719332, 25.56454579224779877, 49.97284587932492883 ) ) ;
#12512 = CARTESIAN_POINT ( 'NONE',  ( 49.32483701613094240, 27.82587066347689486, 45.91328182968236860 ) ) ;
#12513 = VECTOR ( 'NONE', #29415, 1000.000000000000000 ) ;
#12514 = ORIENTED_EDGE ( 'NONE', *, *, #27507, .T. ) ;
#12515 = DIRECTION ( 'NONE',  ( 0.000000000000000000, 1.000000000000000000, 0.000000000000000000 ) ) ;
#12516 = CARTESIAN_POINT ( 'NONE',  ( 44.21498992391907024, 27.29488759933318676, 46.89958605635244027 ) ) ;
#12517 = DIRECTION ( 'NONE',  ( -1.000000000000000000, 0.000000000000000000, 0.000000000000000000 ) ) ;
#12518 = CARTESIAN_POINT ( 'NONE',  ( 47.63716429968715005, 27.61960992152947725, 49.58068632438585155 ) ) ;
#12519 = DIRECTION ( 'NONE',  ( -1.101824276508909887E-16, 1.000000000000000000, -0.000000000000000000 ) ) ;
#12520 = CARTESIAN_POINT ( 'NONE',  ( -40.59307405792756640, 7.534955460439816122, 60.29072935073783412 ) ) ;
#12521 = DIRECTION ( 'NONE',  ( -6.722685822323786766E-17, 1.000000000000000000, 0.000000000000000000 ) ) ;
#12522 = FACE_OUTER_BOUND ( 'NONE', #23286, .T. ) ;
#12523 = DIRECTION ( 'NONE',  ( -1.000000000000000000, 0.000000000000000000, 0.000000000000000000 ) ) ;
#12524 = CARTESIAN_POINT ( 'NONE',  ( -40.54828680531407770, 6.846271790121643441, 39.54930799450052348 ) ) ;
#12525 = EDGE_LOOP ( 'NONE', ( #32086, #6602, #23310 ) ) ;
#12526 = ORIENTED_EDGE ( 'NONE', *, *, #7668, .T. ) ;
#12527 = CARTESIAN_POINT ( 'NONE',  ( 21.09992658989238734, 38.56284415653841791, 47.04930799450051637 ) ) ;
#12528 = CARTESIAN_POINT ( 'NONE',  ( 49.59575279743435772, 24.95410501111153323, 46.37542181765395100 ) ) ;
#12529 = CARTESIAN_POINT ( 'NONE',  ( -31.47697969167641219, 0.8211122444364866713, 14.16255949990320318 ) ) ;
#12530 = VECTOR ( 'NONE', #22653, 1000.000000000000000 ) ;
#12531 = CIRCLE ( 'NONE', #22978, 31.50000000000000711 ) ;
#12532 = EDGE_LOOP ( 'NONE', ( #28377, #22189, #20689, #7851 ) ) ;
#12533 = DIRECTION ( 'NONE',  ( -1.000000000000000000, 0.000000000000000000, 0.000000000000000000 ) ) ;
#12534 = FACE_OUTER_BOUND ( 'NONE', #953, .T. ) ;
#12535 = DIRECTION ( 'NONE',  ( 0.000000000000000000, 0.000000000000000000, -1.000000000000000000 ) ) ;
#12536 = EDGE_LOOP ( 'NONE', ( #23432, #14190, #5050, #5640 ) ) ;
#12537 = ORIENTED_EDGE ( 'NONE', *, *, #19743, .F. ) ;
#12538 = DIRECTION ( 'NONE',  ( -0.2756373558169932236, 0.9612616959383205595, -2.271050992151962865E-31 ) ) ;
#12539 = CARTESIAN_POINT ( 'NONE',  ( 45.24946171279598417, 27.80784706826093000, 47.99220971130007030 ) ) ;
#12540 = CARTESIAN_POINT ( 'NONE',  ( 8.698509210239512512, 24.59164230456639544, 47.04930799450051637 ) ) ;
#12541 = CARTESIAN_POINT ( 'NONE',  ( -42.21195563036361875, 4.051200314738730768, 35.04930799450051637 ) ) ;
#12542 = FACE_OUTER_BOUND ( 'NONE', #7134, .T. ) ;
#12543 = ADVANCED_FACE ( 'NONE', ( #17637 ), #5018, .F. ) ;
#12544 = VERTEX_POINT ( 'NONE', #22070 ) ;
#12545 = EDGE_CURVE ( 'NONE', #21091, #28622, #22051, .T. ) ;
#12546 = EDGE_CURVE ( 'NONE', #30210, #9196, #13177, .T. ) ;
#12547 = CARTESIAN_POINT ( 'NONE',  ( 21.09992658989238734, 38.56284415653841791, 47.04930799450051637 ) ) ;
#12548 = AXIS2_PLACEMENT_3D ( 'NONE', #1634, #19019, #29048 ) ;
#12549 = VECTOR ( 'NONE', #13068, 1000.000000000000000 ) ;
#12550 = ORIENTED_EDGE ( 'NONE', *, *, #12042, .T. ) ;
#12551 = DIRECTION ( 'NONE',  ( -1.000000000000000000, 0.000000000000000000, 0.000000000000000000 ) ) ;
#12552 = CARTESIAN_POINT ( 'NONE',  ( 21.09785597605720753, -13.68834655544033652, 102.7436001025633772 ) ) ;
#12553 = VERTEX_POINT ( 'NONE', #12407 ) ;
#12554 = TOROIDAL_SURFACE ( 'NONE', #8859, 12.40141737965286772, 0.1250000000000003331 ) ;
#12555 = DIRECTION ( 'NONE',  ( -0.9612616959383205595, -0.2756373558169931681, 1.660411357259282445E-16 ) ) ;
#12556 = VERTEX_POINT ( 'NONE', #32425 ) ;
#12557 = CARTESIAN_POINT ( 'NONE',  ( 21.09992658989238734, 38.56284415653841791, 47.04930799450051637 ) ) ;
#12558 = DIRECTION ( 'NONE',  ( -1.000000000000000000, 0.000000000000000000, 0.000000000000000000 ) ) ;
#12559 = TOROIDAL_SURFACE ( 'NONE', #17321, 12.61792373059858541, 0.1250000000000004996 ) ;
#12560 = CARTESIAN_POINT ( 'NONE',  ( 21.09785597605719332, 25.56454579224780232, 123.7593585008393831 ) ) ;
#12561 = DIRECTION ( 'NONE',  ( -0.2756373558169952220, 0.9612616959383201154, 0.000000000000000000 ) ) ;
#12562 = ORIENTED_EDGE ( 'NONE', *, *, #17456, .T. ) ;
#12563 = FACE_OUTER_BOUND ( 'NONE', #9180, .T. ) ;
#12564 = CARTESIAN_POINT ( 'NONE',  ( -9.883496200693420164, -5.935668478901861000, -13.53764849166516271 ) ) ;
#12565 = DIRECTION ( 'NONE',  ( 0.000000000000000000, 0.000000000000000000, -1.000000000000000000 ) ) ;
#12566 = LINE ( 'NONE', #82, #25566 ) ;
#12567 = CARTESIAN_POINT ( 'NONE',  ( 72.46539012849335393, 9.161285963347369332, 74.39120288609333898 ) ) ;
#12568 = EDGE_LOOP ( 'NONE', ( #13737, #17039, #2678, #3890 ) ) ;
#12569 = DIRECTION ( 'NONE',  ( -1.101824276508909887E-16, 1.000000000000000000, -0.000000000000000000 ) ) ;
#12570 = CARTESIAN_POINT ( 'NONE',  ( 33.72499318558949710, 31.09143805560860585, 47.04930799450051637 ) ) ;
#12571 = ORIENTED_EDGE ( 'NONE', *, *, #12235, .F. ) ;
#12573 = EDGE_CURVE ( 'NONE', #28679, #14445, #26787, .T. ) ;
#12572 = DIRECTION ( 'NONE',  ( -1.000000000000000000, 0.000000000000000000, 0.000000000000000000 ) ) ;
#12574 = AXIS2_PLACEMENT_3D ( 'NONE', #31121, #9108, #31761 ) ;
#12575 = VECTOR ( 'NONE', #20263, 1000.000000000000000 ) ;
#12576 = CARTESIAN_POINT ( 'NONE',  ( 21.09992658989239089, 29.97145308207317527, 47.04930799450051637 ) ) ;
#12577 = VERTEX_POINT ( 'NONE', #14703 ) ;
#12578 = DIRECTION ( 'NONE',  ( 0.000000000000000000, 0.000000000000000000, 1.000000000000000000 ) ) ;
#12579 = ORIENTED_EDGE ( 'NONE', *, *, #19632, .F. ) ;
#12580 = TOROIDAL_SURFACE ( 'NONE', #4694, 12.40141737965281621, 0.1250000000000009159 ) ;
#12581 = CIRCLE ( 'NONE', #2066, 0.1249999999999931721 ) ;
#12582 = ORIENTED_EDGE ( 'NONE', *, *, #9627, .T. ) ;
#12583 = B_SPLINE_CURVE_WITH_KNOTS ( 'NONE', 3,
 ( #27108, #14487, #9389, #2169, #4305, #16929, #22179, #26947, #14322, #12348, #32206, #9723, #19716, #24159, #22342, #9879, #19878, #29418, #29912, #26620, #9231, #1675, #11698, #21690, #24479, #19220, #6926, #1999, #32043, #29245, #12016, #22009, #10706, #13161, #2812, #10051 ),
 .UNSPECIFIED., .F., .F.,
 ( 4, 2, 2, 2, 2, 2, 2, 2, 2, 2, 2, 2, 2, 2, 2, 2, 2, 4 ),
 ( 0.000000000000000000, 0.001327013081135470672, 0.002654026162270941343, 0.003981039243406411798, 0.005308052324541882687, 0.006635065405677354443, 0.007962078486812823597, 0.01061610464908375670, 0.01194311773021922325, 0.01327013081135468633, 0.01459714389249015289, 0.01592415697362561944, 0.01725117005476108772, 0.01857818313589655254, 0.01924168967646429015, 0.01990519621703202777, 0.02056870275759976538, 0.02123220929816750299 ),
 .UNSPECIFIED. ) ;
#12584 = ADVANCED_FACE ( 'NONE', ( #2708 ), #4256, .T. ) ;
#12585 = EDGE_CURVE ( 'NONE', #20587, #20020, #3196, .T. ) ;
#12586 = EDGE_CURVE ( 'NONE', #20229, #22591, #29799, .T. ) ;
#12587 = CIRCLE ( 'NONE', #31433, 12.27641737965284463 ) ;
#12588 = EDGE_CURVE ( 'NONE', #20217, #7822, #19754, .T. ) ;
#12589 = AXIS2_PLACEMENT_3D ( 'NONE', #5659, #25679, #30774 ) ;
#12590 = CARTESIAN_POINT ( 'NONE',  ( -9.880269301913145341, -5.935454207809699234, 107.5832060159989965 ) ) ;
#12591 = DIRECTION ( 'NONE',  ( 0.000000000000000000, 1.000000000000000000, 0.000000000000000000 ) ) ;
#12592 = AXIS2_PLACEMENT_3D ( 'NONE', #27815, #22548, #19926 ) ;
#12593 = EDGE_LOOP ( 'NONE', ( #22840, #26688, #22243, #18693, #26364 ) ) ;
#12594 = ORIENTED_EDGE ( 'NONE', *, *, #11091, .T. ) ;
#12595 = CARTESIAN_POINT ( 'NONE',  ( 73.21163767355515972, 2.112486173643641774, 14.77625786722979839 ) ) ;
#12596 = FACE_OUTER_BOUND ( 'NONE', #20624, .T. ) ;
#12597 = DIRECTION ( 'NONE',  ( 0.8746197071393925215, -0.4848096202463429982, -8.676864087101708112E-18 ) ) ;
#12598 = CARTESIAN_POINT ( 'NONE',  ( 21.09785597605719687, 25.76454579224776964, 78.54930799450052348 ) ) ;
#12599 = ORIENTED_EDGE ( 'NONE', *, *, #25793, .F. ) ;
#12600 = CARTESIAN_POINT ( 'NONE',  ( -11.74161162749063081, 0.8961463385898310596, 99.60459568951398523 ) ) ;
#12601 = EDGE_LOOP ( 'NONE', ( #22052, #17638, #30839, #4388, #754, #1653 ) ) ;
#12602 = CARTESIAN_POINT ( 'NONE',  ( -30.25345129064801242, 9.506884710854171416, 20.08466430870300101 ) ) ;
#12603 = DIRECTION ( 'NONE',  ( -1.000000000000000000, 0.000000000000000000, 0.000000000000000000 ) ) ;
#12604 = VERTEX_POINT ( 'NONE', #31092 ) ;
#12605 = DIRECTION ( 'NONE',  ( 1.000000000000000000, 0.000000000000000000, 0.000000000000000000 ) ) ;
#12606 = DIRECTION ( 'NONE',  ( 0.4848096202463645921, 0.8746197071393805311, 0.000000000000000000 ) ) ;
#12607 = AXIS2_PLACEMENT_3D ( 'NONE', #22800, #315, #30360 ) ;
#12608 = AXIS2_PLACEMENT_3D ( 'NONE', #3118, #10701, #26089 ) ;
#12609 = CARTESIAN_POINT ( 'NONE',  ( 48.79601671567883159, 22.86454579224779948, 48.10649398831456125 ) ) ;
#12610 = CARTESIAN_POINT ( 'NONE',  ( 47.73724253767792192, 22.99884124225578219, 48.30271392650413276 ) ) ;
#12611 = DIRECTION ( 'NONE',  ( -1.101824276508909887E-16, 1.000000000000000000, -0.000000000000000000 ) ) ;
#12612 = CARTESIAN_POINT ( 'NONE',  ( 48.94625023931840957, 27.37124452788248874, 46.10640627770150246 ) ) ;
#12613 = CIRCLE ( 'NONE', #30950, 58.70143199044622406 ) ;
#12614 = CARTESIAN_POINT ( 'NONE',  ( -40.11085926462317275, 6.816553873983406397, 34.73944010433842067 ) ) ;
#12615 = CARTESIAN_POINT ( 'NONE',  ( 47.09785597605719687, 25.56454579224779167, 47.04930799450078638 ) ) ;
#12616 = ORIENTED_EDGE ( 'NONE', *, *, #32291, .T. ) ;
#12617 = CARTESIAN_POINT ( 'NONE',  ( 47.17209261226641104, 29.58954579224849368, 44.97563639035409011 ) ) ;
#12619 = EDGE_CURVE ( 'NONE', #13764, #2697, #6457, .T. ) ;
#12618 = CARTESIAN_POINT ( 'NONE',  ( -41.59221410450253842, 0.6853199587562655015, 52.04930799450050927 ) ) ;
#12620 = EDGE_LOOP ( 'NONE', ( #5254, #31849, #3100, #25226, #24234, #2151 ) ) ;
#12621 = EDGE_CURVE ( 'NONE', #9462, #7489, #27839, .T. ) ;
#12622 = FACE_OUTER_BOUND ( 'NONE', #23338, .T. ) ;
#12623 = EDGE_LOOP ( 'NONE', ( #24069, #6878, #4717, #14691, #27054, #11894, #2240, #25693 ) ) ;
#12624 = ORIENTED_EDGE ( 'NONE', *, *, #7038, .F. ) ;
#12625 = FACE_OUTER_BOUND ( 'NONE', #25208, .T. ) ;
#12626 = AXIS2_PLACEMENT_3D ( 'NONE', #24981, #9884, #27278 ) ;
#12627 = EDGE_LOOP ( 'NONE', ( #24988, #8130, #20548, #16835 ) ) ;
#12628 = EDGE_CURVE ( 'NONE', #31146, #26439, #25673, .T. ) ;
#12629 = TOROIDAL_SURFACE ( 'NONE', #27273, 12.40141737965287660, 0.1250000000000007772 ) ;
#12630 = CIRCLE ( 'NONE', #4223, 0.1999999999999970690 ) ;
#12631 = ORIENTED_EDGE ( 'NONE', *, *, #20084, .F. ) ;
#12632 = CIRCLE ( 'NONE', #19963, 12.62506659569710266 ) ;
#12633 = DIRECTION ( 'NONE',  ( -1.000000000000000000, 0.000000000000000000, 0.000000000000000000 ) ) ;
#12634 = AXIS2_PLACEMENT_3D ( 'NONE', #10712, #8084, #200 ) ;
#12635 = EDGE_LOOP ( 'NONE', ( #21398, #786, #8970, #2160 ) ) ;
#12636 = DIRECTION ( 'NONE',  ( -1.000000000000000000, -1.101824276508909887E-16, 0.000000000000000000 ) ) ;
#12637 =( BOUNDED_CURVE ( )  B_SPLINE_CURVE ( 2, ( #4099, #3949, #23959, #1476, #14125 ),
 .UNSPECIFIED., .F., .F. ) 
 B_SPLINE_CURVE_WITH_KNOTS ( ( 3, 2, 3 ),
 ( 0.08390304798631194327, 0.09523809523809523281, 0.1071428583041297289 ),
 .UNSPECIFIED. ) 
 CURVE ( )  GEOMETRIC_REPRESENTATION_ITEM ( )  RATIONAL_B_SPLINE_CURVE ( ( 0.9331661161814950312, 0.9362184480970371370, 1.000000000000000000, 0.9330126953578162796, 0.9330127018922200755 ) ) 
 REPRESENTATION_ITEM ( '' )  );
#12638 = DIRECTION ( 'NONE',  ( 1.000000000000000000, 0.000000000000000000, 0.000000000000000000 ) ) ;
#12639 = DIRECTION ( 'NONE',  ( 0.4848096202463783588, 0.8746197071393729816, 0.000000000000000000 ) ) ;
#12640 = ADVANCED_FACE ( 'NONE', ( #8600 ), #3178, .F. ) ;
#12641 = CARTESIAN_POINT ( 'NONE',  ( 48.37829923888483563, 28.85122849631042286, 45.07556196625585443 ) ) ;
#12642 = ORIENTED_EDGE ( 'NONE', *, *, #27867, .F. ) ;
#12643 = EDGE_LOOP ( 'NONE', ( #21220, #17814, #25424, #15596 ) ) ;
#12644 = DIRECTION ( 'NONE',  ( -0.000000000000000000, -1.000000000000000000, 0.000000000000000000 ) ) ;
#12645 = CIRCLE ( 'NONE', #11070, 0.1000000000000018235 ) ;
#12646 = EDGE_LOOP ( 'NONE', ( #22121, #18106, #22544, #32477 ) ) ;
#12647 = EDGE_CURVE ( 'NONE', #24672, #23918, #15248, .T. ) ;
#12648 = CARTESIAN_POINT ( 'NONE',  ( 21.09785597605807439, -5.935454207752083988, 47.04930799450051637 ) ) ;
#12649 = FACE_OUTER_BOUND ( 'NONE', #18586, .T. ) ;
#12650 = CARTESIAN_POINT ( 'NONE',  ( 33.72499318558949710, 32.09184655352418503, 47.04930799450051637 ) ) ;
#12651 = DIRECTION ( 'NONE',  ( -1.000000000000000000, 0.000000000000000000, 0.000000000000000000 ) ) ;
#12652 = DIRECTION ( 'NONE',  ( 0.000000000000000000, 0.000000000000000000, -1.000000000000000000 ) ) ;
#12653 = CONTEXT_DEPENDENT_SHAPE_REPRESENTATION ( #24188, #6413 ) ;
#12654 = ORIENTED_EDGE ( 'NONE', *, *, #29732, .F. ) ;
#12655 = ORIENTED_EDGE ( 'NONE', *, *, #20082, .T. ) ;
#12656 = CARTESIAN_POINT ( 'NONE',  ( -4.902144023942810236, 25.56454579224779167, 44.54930799450042400 ) ) ;
#12657 = EDGE_CURVE ( 'NONE', #22918, #1340, #22596, .T. ) ;
#12658 = CYLINDRICAL_SURFACE ( 'NONE', #29817, 19.00000000000000000 ) ;
#12659 = ADVANCED_FACE ( 'NONE', ( #13220 ), #15984, .T. ) ;
#12660 = EDGE_CURVE ( 'NONE', #15228, #12910, #17868, .T. ) ;
#12661 = DIRECTION ( 'NONE',  ( 0.4848096202463429982, 0.8746197071393925215, 9.920727850371698576E-18 ) ) ;
#12662 = ORIENTED_EDGE ( 'NONE', *, *, #26797, .T. ) ;
#12663 = CARTESIAN_POINT ( 'NONE',  ( 46.99023568444673060, 29.32451373492759217, 49.12151524109405898 ) ) ;
#12664 = AXIS2_PLACEMENT_3D ( 'NONE', #15225, #2584, #12447 ) ;
#12665 = ORIENTED_EDGE ( 'NONE', *, *, #25569, .F. ) ;
#12666 = CARTESIAN_POINT ( 'NONE',  ( -42.36153388572594736, 13.68895619636815475, 59.46110983642625314 ) ) ;
#12667 = AXIS2_PLACEMENT_3D ( 'NONE', #17791, #723, #27816 ) ;
#12668 = CARTESIAN_POINT ( 'NONE',  ( 21.09785597605720042, -6.659195188345857552, 114.2205349567709476 ) ) ;
#12669 = DIRECTION ( 'NONE',  ( 0.000000000000000000, 0.000000000000000000, -1.000000000000000000 ) ) ;
#12670 = ADVANCED_FACE ( 'NONE', ( #18273 ), #20487, .T. ) ;
#12671 = CIRCLE ( 'NONE', #15282, 0.9999999999999986677 ) ;
#12672 = ORIENTED_EDGE ( 'NONE', *, *, #16517, .F. ) ;
#12673 = ORIENTED_EDGE ( 'NONE', *, *, #4753, .T. ) ;
#12674 = CARTESIAN_POINT ( 'NONE',  ( -37.69242682074983719, -5.812585053298397142, 15.41977583216693226 ) ) ;
#12675 = DIRECTION ( 'NONE',  ( -1.224646799147353207E-16, -1.349345573449484691E-32, 1.000000000000000000 ) ) ;
#12676 = CARTESIAN_POINT ( 'NONE',  ( 48.94625023931840957, 27.45784706826093213, 46.10640627770150246 ) ) ;
#12677 = ORIENTED_EDGE ( 'NONE', *, *, #19376, .F. ) ;
#12678 = AXIS2_PLACEMENT_3D ( 'NONE', #31928, #31606, #19108 ) ;
#12679 = CARTESIAN_POINT ( 'NONE',  ( -38.65545646816406133, 8.768497436727981764, 75.00977582921336762 ) ) ;
#12680 = AXIS2_PLACEMENT_3D ( 'NONE', #24539, #21907, #14378 ) ;
#12681 = CARTESIAN_POINT ( 'NONE',  ( 21.09992658989238734, 38.56284415653841791, 47.04930799450051637 ) ) ;
#12682 = DIRECTION ( 'NONE',  ( 0.000000000000000000, -1.000000000000000000, 0.000000000000000000 ) ) ;
#12683 = EDGE_CURVE ( 'NONE', #12114, #27545, #23531, .T. ) ;
#12684 = AXIS2_PLACEMENT_3D ( 'NONE', #19225, #6770, #31084 ) ;
#12685 = CARTESIAN_POINT ( 'NONE',  ( 8.474859994195286461, 28.09184655352419213, 47.04930799450051637 ) ) ;
#12686 = EDGE_CURVE ( 'NONE', #28026, #20793, #31891, .T. ) ;
#12687 = FACE_OUTER_BOUND ( 'NONE', #25968, .T. ) ;
#12688 = CARTESIAN_POINT ( 'NONE',  ( 8.823509210239533829, 26.84164230456639899, 47.04930799450051637 ) ) ;
#12689 = FACE_OUTER_BOUND ( 'NONE', #4506, .T. ) ;
#12690 = CARTESIAN_POINT ( 'NONE',  ( 45.37383841111020644, 22.88065857334295217, 47.92876263475718446 ) ) ;
#12691 = CARTESIAN_POINT ( 'NONE',  ( -40.90015969217747482, 8.955334253785164123, 57.04930799450051637 ) ) ;
#12692 = DIRECTION ( 'NONE',  ( 0.8746197071393926326, -0.4848096202463430537, -8.676864087101709653E-18 ) ) ;
#12693 = CARTESIAN_POINT ( 'NONE',  ( -42.38687957179149635, 4.148162238787999279, 35.14930799450051779 ) ) ;
#12694 =( NAMED_UNIT ( * ) SI_UNIT ( $, .STERADIAN. ) SOLID_ANGLE_UNIT ( ) );
#12695 = ORIENTED_EDGE ( 'NONE', *, *, #27867, .T. ) ;
#12696 = ORIENTED_EDGE ( 'NONE', *, *, #5406, .T. ) ;
#12697 = LINE ( 'NONE', #20218, #2420 ) ;
#12698 = CIRCLE ( 'NONE', #3235, 12.36707279061065101 ) ;
#12699 = DIRECTION ( 'NONE',  ( -1.101824276508909887E-16, 1.000000000000000000, -0.000000000000000000 ) ) ;
#12700 = EDGE_CURVE ( 'NONE', #27012, #8335, #28949, .T. ) ;
#12701 = DIRECTION ( 'NONE',  ( -1.101824276508909887E-16, 1.000000000000000000, -0.000000000000000000 ) ) ;
#12702 = ADVANCED_FACE ( 'NONE', ( #14011 ), #11378, .T. ) ;
#12703 = CARTESIAN_POINT ( 'NONE',  ( 71.48501281440437083, 5.388785998227653806, 77.62194537253989779 ) ) ;
#12704 = EDGE_LOOP ( 'NONE', ( #10011, #9567 ) ) ;
#12705 = FACE_OUTER_BOUND ( 'NONE', #7313, .T. ) ;
#12706 = CARTESIAN_POINT ( 'NONE',  ( -20.40214402394279603, 14.86454579224779948, 47.04930799450052348 ) ) ;
#12707 = CYLINDRICAL_SURFACE ( 'NONE', #26711, 12.36707279061065101 ) ;
#12708 = ORIENTED_EDGE ( 'NONE', *, *, #6183, .T. ) ;
#12709 = VERTEX_POINT ( 'NONE', #6293 ) ;
#12710 = DIRECTION ( 'NONE',  ( -0.000000000000000000, 1.000000000000000000, -0.000000000000000000 ) ) ;
#12711 = CARTESIAN_POINT ( 'NONE',  ( 46.00908685603034343, 27.63284706826092929, 44.91496614357595263 ) ) ;
#12712 = CARTESIAN_POINT ( 'NONE',  ( 21.09785597605720042, -16.93545420775220123, 47.04930799450051637 ) ) ;
#12713 = CARTESIAN_POINT ( 'NONE',  ( 33.50134396954526750, 24.59164230456639544, 47.04930799450051637 ) ) ;
#12714 = AXIS2_PLACEMENT_3D ( 'NONE', #5040, #32122, #24730 ) ;
#12715 = CARTESIAN_POINT ( 'NONE',  ( -40.64500813507293486, 6.819128862114091305, 34.57932936825760351 ) ) ;
#12716 = VECTOR ( 'NONE', #4153, 1000.000000000000000 ) ;
#12717 = EDGE_LOOP ( 'NONE', ( #7558, #9329, #22593, #17548 ) ) ;
#12718 = DIRECTION ( 'NONE',  ( 1.000000000000000000, 0.000000000000000000, 0.000000000000000000 ) ) ;
#12719 = AXIS2_PLACEMENT_3D ( 'NONE', #3541, #13732, #23566 ) ;
#12720 = ORIENTED_EDGE ( 'NONE', *, *, #6112, .F. ) ;
#12721 = CIRCLE ( 'NONE', #16882, 12.36707279061065101 ) ;
#12722 = LINE ( 'NONE', #17619, #26534 ) ;
#12723 = CARTESIAN_POINT ( 'NONE',  ( -40.38516919650994197, 8.640923867788874446, 39.44930799450052206 ) ) ;
#12724 = VECTOR ( 'NONE', #5081, 1000.000000000000000 ) ;
#12725 = ORIENTED_EDGE ( 'NONE', *, *, #4262, .T. ) ;
#12726 = CARTESIAN_POINT ( 'NONE',  ( 21.09785597605720042, 13.06454579224779877, -7.250692005499486115 ) ) ;
#12727 = VERTEX_POINT ( 'NONE', #21370 ) ;
#12728 = DIRECTION ( 'NONE',  ( -1.000000000000000000, 0.000000000000000000, 0.000000000000000000 ) ) ;
#12729 = DIRECTION ( 'NONE',  ( 0.000000000000000000, -0.7660444431189775694, -0.6427876096865398070 ) ) ;
#12730 = DIRECTION ( 'NONE',  ( 0.4848096202463430537, 0.8746197071393926326, -1.125439520643636483E-16 ) ) ;
#12731 = DIRECTION ( 'NONE',  ( -0.000000000000000000, -1.000000000000000000, 0.000000000000000000 ) ) ;
#12732 = ORIENTED_EDGE ( 'NONE', *, *, #9375, .F. ) ;
#12733 = CARTESIAN_POINT ( 'NONE',  ( 79.08111791895156273, -5.943281723642246384, 78.07730698287811322 ) ) ;
#12734 = LINE ( 'NONE', #240, #9525 ) ;
#12735 = CARTESIAN_POINT ( 'NONE',  ( 33.50134396954518223, 32.34164230456639899, 47.04930799450051637 ) ) ;
#12736 = EDGE_CURVE ( 'NONE', #3138, #19781, #19232, .T. ) ;
#12737 = DIRECTION ( 'NONE',  ( -0.4848096202463424431, -0.8746197071393927436, 2.220446049250312588E-16 ) ) ;
#12738 = EDGE_CURVE ( 'NONE', #14305, #490, #31410, .T. ) ;
#12739 = ADVANCED_FACE ( 'NONE', ( #29262 ), #8750, .T. ) ;
#12740 = CARTESIAN_POINT ( 'NONE',  ( 21.09785597605719332, 6.547041198165487685, 47.04930799450051637 ) ) ;
#12741 = EDGE_LOOP ( 'NONE', ( #19665, #25519, #29067, #17368, #11557, #30242, #16098, #20246, #21812, #15264, #28703, #25499, #6368, #17562, #10779, #4550 ) ) ;
#12742 = CARTESIAN_POINT ( 'NONE',  ( 34.59963999142011204, 15.70210863493540288, 47.04930799450052348 ) ) ;
#12743 = CARTESIAN_POINT ( 'NONE',  ( 0.6836613156275018754, 11.92558985988973497, 99.04321908912905315 ) ) ;
#12744 = ORIENTED_EDGE ( 'NONE', *, *, #19664, .F. ) ;
#12745 = CYLINDRICAL_SURFACE ( 'NONE', #28806, 2.500000000000002220 ) ;
#12746 = FACE_OUTER_BOUND ( 'NONE', #16742, .T. ) ;
#12747 = CYLINDRICAL_SURFACE ( 'NONE', #11168, 1.500000000000001332 ) ;
#12748 = VECTOR ( 'NONE', #317, 1000.000000000000000 ) ;
#12749 = VERTEX_POINT ( 'NONE', #6778 ) ;
#12750 = B_SPLINE_SURFACE_WITH_KNOTS ( 'NONE', 3, 1, ( 
 ( #14524, #2043 ),
 ( #12064, #29134 ),
 ( #9600, #28970 ),
 ( #26661, #16489 ) ),
 .UNSPECIFIED., .F., .F., .F.,
 ( 4, 4 ),
 ( 2, 2 ),
 ( 0.1800733115436725096, 0.1889470565094409915 ),
 ( 0.000000000000000000, 1.000000000000000000 ),
 .UNSPECIFIED. ) ;
#12751 = CARTESIAN_POINT ( 'NONE',  ( 21.09785597605719332, 17.16451738380053627, 47.04930799450051637 ) ) ;
#12752 = ORIENTED_EDGE ( 'NONE', *, *, #2663, .T. ) ;
#12753 = AXIS2_PLACEMENT_3D ( 'NONE', #25902, #10329, #10495 ) ;
#12754 = ORIENTED_EDGE ( 'NONE', *, *, #26689, .F. ) ;
#12755 = AXIS2_PLACEMENT_3D ( 'NONE', #22081, #26530, #16508 ) ;
#12756 = CARTESIAN_POINT ( 'NONE',  ( -9.880269303432738681, -5.935454207752202116, -37.95069200549950494 ) ) ;
#12757 = DIRECTION ( 'NONE',  ( 0.000000000000000000, 0.000000000000000000, -1.000000000000000000 ) ) ;
#12758 = VERTEX_POINT ( 'NONE', #16300 ) ;
#12759 = EDGE_LOOP ( 'NONE', ( #9059, #24334, #24000, #26152 ) ) ;
#12760 = VECTOR ( 'NONE', #29019, 1000.000000000000000 ) ;
#12761 = CARTESIAN_POINT ( 'NONE',  ( 21.09785597605719332, 14.86454579224779948, -7.160742511838298796 ) ) ;
#12762 = DIRECTION ( 'NONE',  ( -1.000000000000000000, 0.000000000000000000, 0.000000000000000000 ) ) ;
#12763 = CARTESIAN_POINT ( 'NONE',  ( -30.25373303598937369, 9.514306310867874927, 74.00447224759949449 ) ) ;
#12764 = AXIS2_PLACEMENT_3D ( 'NONE', #5405, #15409, #25420 ) ;
#12765 = DIRECTION ( 'NONE',  ( 0.9612616959383207815, 0.2756373558169927240, 8.795445018804291370E-19 ) ) ;
#12766 = ORIENTED_EDGE ( 'NONE', *, *, #25214, .T. ) ;
#12767 = DIRECTION ( 'NONE',  ( -0.000000000000000000, -1.000000000000000000, -0.000000000000000000 ) ) ;
#12768 = ORIENTED_EDGE ( 'NONE', *, *, #8407, .T. ) ;
#12769 = CARTESIAN_POINT ( 'NONE',  ( -36.31984027485262345, -5.100301982865893535, 14.30915805386189454 ) ) ;
#12770 = ORIENTED_EDGE ( 'NONE', *, *, #16380, .F. ) ;
#12771 = CARTESIAN_POINT ( 'NONE',  ( 21.09785597605719332, 17.16451738380053627, 47.04930799450051637 ) ) ;
#12772 = DIRECTION ( 'NONE',  ( -1.000000000000000000, -1.101824276508909887E-16, 0.000000000000000000 ) ) ;
#12773 = DIRECTION ( 'NONE',  ( -1.000000000000000000, 0.000000000000000000, 0.000000000000000000 ) ) ;
#12774 = CARTESIAN_POINT ( 'NONE',  ( 8.474859994195281132, 38.56284415653841791, 47.04930799450051637 ) ) ;
#12775 = EDGE_CURVE ( 'NONE', #12556, #32160, #7412, .T. ) ;
#12776 = EDGE_CURVE ( 'NONE', #20484, #25801, #16830, .T. ) ;
#12777 = CARTESIAN_POINT ( 'NONE',  ( 45.35708200440645044, 29.70457786121581378, 45.92000246470679770 ) ) ;
#12778 = EDGE_CURVE ( 'NONE', #12159, #16815, #23113, .T. ) ;
#12779 = CIRCLE ( 'NONE', #8064, 12.36707279061065101 ) ;
#12780 = AXIS2_PLACEMENT_3D ( 'NONE', #18191, #3910, #11151 ) ;
#12781 = DIRECTION ( 'NONE',  ( 0.8746197071393858602, -0.4848096202463547666, 0.000000000000000000 ) ) ;
#12782 = FACE_OUTER_BOUND ( 'NONE', #19945, .T. ) ;
#12783 = ADVANCED_FACE ( 'NONE', ( #31252 ), #29419, .T. ) ;
#12784 = EDGE_CURVE ( 'NONE', #3119, #18133, #13680, .T. ) ;
#12785 = ORIENTED_EDGE ( 'NONE', *, *, #2527, .T. ) ;
#12786 = CARTESIAN_POINT ( 'NONE',  ( -40.44437521412186243, 7.396217677353668307, 34.54930799450052348 ) ) ;
#12787 = ORIENTED_EDGE ( 'NONE', *, *, #4615, .T. ) ;
#12788 = CARTESIAN_POINT ( 'NONE',  ( -41.34584395867850048, 11.59800658573647425, 57.95249952744806166 ) ) ;
#12789 = EDGE_LOOP ( 'NONE', ( #4324, #7991, #1736, #15236, #1558, #9131 ) ) ;
#12790 = ORIENTED_EDGE ( 'NONE', *, *, #25283, .T. ) ;
#12791 = DIRECTION ( 'NONE',  ( -0.2756373558169638582, 0.9612616959383291082, -1.479773560108318178E-16 ) ) ;
#12792 = ORIENTED_EDGE ( 'NONE', *, *, #22565, .T. ) ;
#12793 = AXIS2_PLACEMENT_3D ( 'NONE', #15871, #25552, #23257 ) ;
#12794 = CIRCLE ( 'NONE', #5963, 12.36707279061065101 ) ;
#12795 = VECTOR ( 'NONE', #15478, 1000.000000000000000 ) ;
#12796 = ORIENTED_EDGE ( 'NONE', *, *, #17146, .T. ) ;
#12797 = CARTESIAN_POINT ( 'NONE',  ( 45.63968093275011029, 22.91413368675619111, 48.10984057092807831 ) ) ;
#12798 = EDGE_CURVE ( 'NONE', #27774, #27386, #31513, .T. ) ;
#12799 = VERTEX_POINT ( 'NONE', #1688 ) ;
#12800 = DIRECTION ( 'NONE',  ( 0.000000000000000000, 0.000000000000000000, 1.000000000000000000 ) ) ;
#12801 = DIRECTION ( 'NONE',  ( -1.101824276508909887E-16, 1.000000000000000000, -0.000000000000000000 ) ) ;
#12802 = CARTESIAN_POINT ( 'NONE',  ( 48.18662509608405031, 26.49624452788248874, 49.18364984542562013 ) ) ;
#12803 = ORIENTED_EDGE ( 'NONE', *, *, #7398, .T. ) ;
#12804 = VERTEX_POINT ( 'NONE', #1522 ) ;
#12805 = FACE_OUTER_BOUND ( 'NONE', #19922, .T. ) ;
#12806 = EDGE_LOOP ( 'NONE', ( #4283, #20838, #10030, #15795 ) ) ;
#12807 = CARTESIAN_POINT ( 'NONE',  ( 42.88580625581234074, 11.83469976691315928, 99.40613855222599682 ) ) ;
#12808 = CARTESIAN_POINT ( 'NONE',  ( 54.84005179923816797, -2.833757427854255884, 102.4175021926326536 ) ) ;
#12809 = CYLINDRICAL_SURFACE ( 'NONE', #14318, 12.62506659569710266 ) ;
#12810 = AXIS2_PLACEMENT_3D ( 'NONE', #20176, #29711, #24615 ) ;
#12811 = ADVANCED_BREP_SHAPE_REPRESENTATION ( '', ( #11688, #8172 ), #331 ) ;
#12812 = DIRECTION ( 'NONE',  ( -1.000000000000000000, 0.000000000000000000, 0.000000000000000000 ) ) ;
#12813 = CARTESIAN_POINT ( 'NONE',  ( 21.09785597605719332, 30.36454579224779238, 60.04930799450051637 ) ) ;
#12814 = EDGE_CURVE ( 'NONE', #24996, #18438, #19969, .T. ) ;
#12815 = PRODUCT_CONTEXT ( 'NONE', #22499, 'mechanical' ) ;
#12816 = VERTEX_POINT ( 'NONE', #24171 ) ;
#12817 = ORIENTED_EDGE ( 'NONE', *, *, #5970, .F. ) ;
#12818 = DIRECTION ( 'NONE',  ( 0.000000000000000000, -0.000000000000000000, -1.000000000000000000 ) ) ;
#12819 = DIRECTION ( 'NONE',  ( -1.101824276508909887E-16, 1.000000000000000000, -0.000000000000000000 ) ) ;
#12820 = DIRECTION ( 'NONE',  ( -1.000000000000000000, 0.000000000000000000, 0.000000000000000000 ) ) ;
#12821 = CARTESIAN_POINT ( 'NONE',  ( 45.24946171279598417, 27.80784706826093000, 47.99220971130007740 ) ) ;
#12822 = VERTEX_POINT ( 'NONE', #11543 ) ;
#12823 = CARTESIAN_POINT ( 'NONE',  ( 33.61962556781118394, 32.55121380581068991, 47.04930799450051637 ) ) ;
#12824 = DIRECTION ( 'NONE',  ( -0.2756373558169973870, 0.9612616959383193382, -9.615507602343155278E-33 ) ) ;
#12825 = ADVANCED_FACE ( 'NONE', ( #9080 ), #2690, .T. ) ;
#12826 = EDGE_CURVE ( 'NONE', #20059, #9364, #3721, .T. ) ;
#12827 = ORIENTED_EDGE ( 'NONE', *, *, #482, .F. ) ;
#12828 = CIRCLE ( 'NONE', #15434, 55.85791022362053582 ) ;
#12829 =( BOUNDED_SURFACE ( )  B_SPLINE_SURFACE ( 3, 2, ( 
 ( #13342, #10720, #23499 ),
 ( #10387, #30416, #2983 ),
 ( #30741, #5619, #27948 ),
 ( #10877, #5950, #23011 ),
 ( #527, #5468, #1012 ),
 ( #15468, #3141, #8248 ),
 ( #18235, #13185, #28268 ),
 ( #5787, #15794, #8881 ) ),
 .UNSPECIFIED., .F., .F., .F. ) 
 B_SPLINE_SURFACE_WITH_KNOTS ( ( 4, 2, 2, 4 ),
 ( 3, 3 ),
 ( -3.388131789017201356E-18, 0.0005623261017282641955, 0.0008434891525923980280, 0.001124652203456531861 ),
 ( 0.000000000000000000, 1.000000000000000000 ),
 .UNSPECIFIED. ) 
 GEOMETRIC_REPRESENTATION_ITEM ( )  RATIONAL_B_SPLINE_SURFACE ( (
 ( 1.000000000000000000, 0.7071067811865558994, 1.000000000000000000),
 ( 1.000000000000000000, 0.6846567335763826812, 1.000000000000000000),
 ( 1.000000000000000000, 0.6190846722315239692, 1.000000000000000000),
 ( 1.000000000000000000, 0.5161161862684999768, 1.000000000000000000),
 ( 1.000000000000000000, 0.4814351115863779174, 1.000000000000000000),
 ( 1.000000000000000000, 0.4264341115146433325, 1.000000000000000000),
 ( 1.000000000000000000, 0.4080770041854601127, 1.000000000000000000),
 ( 1.000000000000000000, 0.4082482904638556342, 1.000000000000000000) ) ) 
 REPRESENTATION_ITEM ( '' )  SURFACE ( )  );
#12830 = EDGE_LOOP ( 'NONE', ( #29412, #8024 ) ) ;
#12831 = CARTESIAN_POINT ( 'NONE',  ( -39.67555847965937943, 2.645252416024337361, 47.04930799450051637 ) ) ;
#12832 = ADVANCED_FACE ( 'NONE', ( #14336 ), #24328, .F. ) ;
#12833 = CARTESIAN_POINT ( 'NONE',  ( -44.25806916964057791, -4.109955628810420869, 52.04930799449938661 ) ) ;
#12835 = CARTESIAN_POINT ( 'NONE',  ( 46.00908685603034343, 26.93284706826093000, 44.91496614357595263 ) ) ;
#12834 = AXIS2_PLACEMENT_3D ( 'NONE', #12925, #2417, #25383 ) ;
#12836 = EDGE_CURVE ( 'NONE', #30606, #25372, #454, .T. ) ;
#12837 = AXIS2_PLACEMENT_3D ( 'NONE', #3538, #433, #31128 ) ;
#12838 = CIRCLE ( 'NONE', #16996, 19.21451602543517367 ) ;
#12839 = ORIENTED_EDGE ( 'NONE', *, *, #7258, .T. ) ;
#12840 = FACE_OUTER_BOUND ( 'NONE', #26647, .T. ) ;
#12841 = CARTESIAN_POINT ( 'NONE',  ( 44.21498992391908445, 26.01753733014356129, 46.89958605635242606 ) ) ;
#12842 = DIRECTION ( 'NONE',  ( -1.188208965918165239E-16, -1.880121038077813132E-16, -1.000000000000000000 ) ) ;
#12843 = CARTESIAN_POINT ( 'NONE',  ( 49.70056603649367588, 24.90621246473837047, 47.18448000306445067 ) ) ;
#12844 = DIRECTION ( 'NONE',  ( 0.9612616959383221138, 0.2756373558169876170, 0.000000000000000000 ) ) ;
#12845 = DIRECTION ( 'NONE',  ( 0.000000000000000000, 0.000000000000000000, -1.000000000000000000 ) ) ;
#12846 = DIRECTION ( 'NONE',  ( 0.000000000000000000, 1.000000000000000000, 0.000000000000000000 ) ) ;
#12847 = FACE_OUTER_BOUND ( 'NONE', #19476, .T. ) ;
#12848 = CARTESIAN_POINT ( 'NONE',  ( 49.28428300279882990, 29.04787913140503974, 48.46772541801551171 ) ) ;
#12849 = EDGE_CURVE ( 'NONE', #3369, #5329, #21018, .T. ) ;
#12850 = ORIENTED_EDGE ( 'NONE', *, *, #23977, .F. ) ;
#12851 = VERTEX_POINT ( 'NONE', #4808 ) ;
#12852 = CARTESIAN_POINT ( 'NONE',  ( 21.09785597605719332, 25.18020726757345429, 47.04930799450051637 ) ) ;
#12853 = DIRECTION ( 'NONE',  ( 0.000000000000000000, -0.7071067811865474617, -0.7071067811865474617 ) ) ;
#12854 = CARTESIAN_POINT ( 'NONE',  ( -32.13107803565643650, -0.7131008658029172054, 13.60503564500631057 ) ) ;
#12855 = DIRECTION ( 'NONE',  ( -1.101824276508909887E-16, 1.000000000000000000, -0.000000000000000000 ) ) ;
#12856 = AXIS2_PLACEMENT_3D ( 'NONE', #13636, #18859, #26423 ) ;
#12857 = ORIENTED_EDGE ( 'NONE', *, *, #26716, .T. ) ;
#12858 = CARTESIAN_POINT ( 'NONE',  ( 8.474859994195282908, 38.56284415653841791, 47.04930799450051637 ) ) ;
#12859 = CARTESIAN_POINT ( 'NONE',  ( 21.09785597605720753, 13.86454579224779948, 47.04930799450052348 ) ) ;
#12860 = CARTESIAN_POINT ( 'NONE',  ( 21.09785597605719332, 34.11266481626051217, 60.03349819502754059 ) ) ;
#12861 = ORIENTED_EDGE ( 'NONE', *, *, #1416, .T. ) ;
#12862 = ORIENTED_EDGE ( 'NONE', *, *, #31212, .T. ) ;
#12864 = AXIS2_PLACEMENT_3D ( 'NONE', #13968, #9360, #21165 ) ;
#12863 = CARTESIAN_POINT ( 'NONE',  ( -41.75126335834794133, 15.45321085637654690, 38.54111136810265492 ) ) ;
#12865 = CARTESIAN_POINT ( 'NONE',  ( 45.79384627280941089, 25.76618040159426570, 49.05938063676249072 ) ) ;
#12866 = AXIS2_PLACEMENT_3D ( 'NONE', #3049, #25061, #17993 ) ;
#12867 = AXIS2_PLACEMENT_3D ( 'NONE', #12068, #19928, #31763 ) ;
#12868 = CARTESIAN_POINT ( 'NONE',  ( 48.40186567930498285, 28.82957786121581378, 45.03923535223908203 ) ) ;
#12869 = AXIS2_PLACEMENT_3D ( 'NONE', #31031, #666, #10699 ) ;
#12870 = DIRECTION ( 'NONE',  ( 0.000000000000000000, 0.000000000000000000, 1.000000000000000000 ) ) ;
#12871 = ADVANCED_FACE ( 'NONE', ( #2184 ), #12202, .F. ) ;
#12872 = ADVANCED_FACE ( 'NONE', ( #24995 ), #31902, .T. ) ;
#12873 = EDGE_LOOP ( 'NONE', ( #22423, #19115, #9772, #23565, #24895 ) ) ;
#12874 = B_SPLINE_CURVE_WITH_KNOTS ( 'NONE', 3,
 ( #14213, #16497, #19271, #21577 ),
 .UNSPECIFIED., .F., .F.,
 ( 4, 4 ),
 ( 0.000000000000000000, 0.0001555497290426954599 ),
 .UNSPECIFIED. ) ;
#12875 = B_SPLINE_CURVE_WITH_KNOTS ( 'NONE', 3,
 ( #872, #20894, #18425, #28455, #17752, #28103, #2972, #20699, #199, #20540, #7592, #2662 ),
 .UNSPECIFIED., .F., .F.,
 ( 4, 2, 2, 2, 2, 4 ),
 ( 0.0003422200191418629670, 0.002082436906217386297, 0.003822653793292909736, 0.005562870680368433608, 0.006432979123906195328, 0.007303087567443957047 ),
 .UNSPECIFIED. ) ;
#12876 = CARTESIAN_POINT ( 'NONE',  ( -39.58809650894544774, 2.596771453999702661, 45.04930799450051637 ) ) ;
#12877 = ADVANCED_FACE ( 'NONE', ( #22518 ), #24487, .F. ) ;
#12878 = ORIENTED_EDGE ( 'NONE', *, *, #19208, .F. ) ;
#12879 = ADVANCED_FACE ( 'NONE', ( #29757 ), #29819, .T. ) ;
#12880 = TOROIDAL_SURFACE ( 'NONE', #19122, 12.40141737965288193, 0.1250000000000005829 ) ;
#12881 = DIRECTION ( 'NONE',  ( -1.000000000000000000, 0.000000000000000000, 0.000000000000000000 ) ) ;
#12882 = DIRECTION ( 'NONE',  ( -1.101824276508909887E-16, 1.000000000000000000, -0.000000000000000000 ) ) ;
#12883 = CIRCLE ( 'NONE', #31223, 1.500000000000001332 ) ;
#12884 = AXIS2_PLACEMENT_3D ( 'NONE', #13727, #8949, #20779 ) ;
#12885 = STYLED_ITEM ( 'NONE', ( #4966 ), #4182 ) ;
#12886 = ORIENTED_EDGE ( 'NONE', *, *, #6933, .F. ) ;
#12887 = CARTESIAN_POINT ( 'NONE',  ( 33.50134396954521065, 30.34164230456639544, 47.04930799450051637 ) ) ;
#12888 = ORIENTED_EDGE ( 'NONE', *, *, #1385, .T. ) ;
#12889 = CONICAL_SURFACE ( 'NONE', #16003, 19.04889477833696176, 0.8552113334772211140 ) ;
#12890 = FACE_OUTER_BOUND ( 'NONE', #17714, .T. ) ;
#12891 = DIRECTION ( 'NONE',  ( 1.000000000000000000, -0.000000000000000000, -0.000000000000000000 ) ) ;
#12892 = CARTESIAN_POINT ( 'NONE',  ( -0.4122223024762697863, 11.86918370369814113, -4.535591127112307497 ) ) ;
#12893 = DIRECTION ( 'NONE',  ( 0.000000000000000000, 0.000000000000000000, 1.000000000000000000 ) ) ;
#12894 = VERTEX_POINT ( 'NONE', #10068 ) ;
#12895 = CARTESIAN_POINT ( 'NONE',  ( 44.79156314060809763, 22.86454579224779948, 46.92953032342012420 ) ) ;
#12896 = DIRECTION ( 'NONE',  ( 0.000000000000000000, 0.000000000000000000, -1.000000000000000000 ) ) ;
#12897 = DIRECTION ( 'NONE',  ( -1.000000000000000000, -1.101824276508910010E-16, 0.000000000000000000 ) ) ;
#12898 = FACE_OUTER_BOUND ( 'NONE', #4803, .T. ) ;
#12899 = AXIS2_PLACEMENT_3D ( 'NONE', #22298, #6887, #30473 ) ;
#12900 = CARTESIAN_POINT ( 'NONE',  ( -43.29662792673756400, 1.063067023446606196, 60.54930799450051637 ) ) ;
#12901 = ORIENTED_EDGE ( 'NONE', *, *, #335, .F. ) ;
#12902 = CARTESIAN_POINT ( 'NONE',  ( 21.09785597605719332, 47.56454579224779877, 47.04930799450051637 ) ) ;
#12903 = DIRECTION ( 'NONE',  ( 0.9612616959383205595, 0.2756373558169932236, -1.660411357259282445E-16 ) ) ;
#12904 = VERTEX_POINT ( 'NONE', #20064 ) ;
#12905 = CARTESIAN_POINT ( 'NONE',  ( 33.46699938050304013, 31.22145308207317171, 47.04930799450050927 ) ) ;
#12906 = DIRECTION ( 'NONE',  ( 0.000000000000000000, 0.000000000000000000, 1.000000000000000000 ) ) ;
#12907 = DIRECTION ( 'NONE',  ( 0.000000000000000000, 0.000000000000000000, -1.000000000000000000 ) ) ;
#12908 = CARTESIAN_POINT ( 'NONE',  ( 48.85960306834331135, 19.86454579224779948, 48.19221970711091529 ) ) ;
#12909 = ORIENTED_EDGE ( 'NONE', *, *, #15164, .F. ) ;
#12910 = VERTEX_POINT ( 'NONE', #7276 ) ;
#12911 = EDGE_CURVE ( 'NONE', #5110, #10609, #17371, .T. ) ;
#12912 = CIRCLE ( 'NONE', #1332, 43.50000000000000000 ) ;
#12913 = ORIENTED_EDGE ( 'NONE', *, *, #9538, .T. ) ;
#12914 = EDGE_CURVE ( 'NONE', #27037, #14564, #4124, .T. ) ;
#12915 = CIRCLE ( 'NONE', #21273, 12.36707279061065101 ) ;
#12916 = CARTESIAN_POINT ( 'NONE',  ( 21.09785597605719332, 30.56454579224779522, 47.04930799450051637 ) ) ;
#12917 = CARTESIAN_POINT ( 'NONE',  ( 51.92400919103563695, -5.935454207752202116, -13.56214536183033381 ) ) ;
#12918 = ORIENTED_EDGE ( 'NONE', *, *, #5761, .F. ) ;
#12919 = ORIENTED_EDGE ( 'NONE', *, *, #27914, .F. ) ;
#12920 = CARTESIAN_POINT ( 'NONE',  ( -43.49202504458321528, -4.177434381965055010, 52.06022946855918576 ) ) ;
#12921 = DIRECTION ( 'NONE',  ( -1.101824276508909887E-16, 1.000000000000000000, -0.000000000000000000 ) ) ;
#12922 = CARTESIAN_POINT ( 'NONE',  ( -33.74072439236259413, -1.979772501351858782, 80.74990046129943266 ) ) ;
#12923 = DIRECTION ( 'NONE',  ( -1.101824276508909887E-16, 1.000000000000000000, -0.000000000000000000 ) ) ;
#12924 = ORIENTED_EDGE ( 'NONE', *, *, #28499, .F. ) ;
#12925 = CARTESIAN_POINT ( 'NONE',  ( -40.23967075304302909, 7.740322171013526820, 60.29072935073781991 ) ) ;
#12926 = CARTESIAN_POINT ( 'NONE',  ( 21.09992658989239089, 30.34164230456639544, 47.04930799450051637 ) ) ;
#12927 = DIRECTION ( 'NONE',  ( 0.000000000000000000, 0.000000000000000000, -1.000000000000000000 ) ) ;
#12929 = CARTESIAN_POINT ( 'NONE',  ( -40.98031486389898248, 9.265261353013489298, 39.44930799450052206 ) ) ;
#12928 = VECTOR ( 'NONE', #13492, 1000.000000000000227 ) ;
#12930 = EDGE_LOOP ( 'NONE', ( #15436, #14366, #1415, #21697 ) ) ;
#12931 = CARTESIAN_POINT ( 'NONE',  ( 47.58479084802739578, 23.04411657098542676, 46.02349645909773557 ) ) ;
#12932 = DIRECTION ( 'NONE',  ( -4.793929595204190462E-17, -1.000000000000000000, -3.360725575046568817E-16 ) ) ;
#12933 = CARTESIAN_POINT ( 'NONE',  ( 45.90820269358763994, 22.93328494799376571, 48.28896993515231628 ) ) ;
#12934 = DIRECTION ( 'NONE',  ( -0.4848096202463421656, -0.8746197071393929656, -9.920727850371707821E-18 ) ) ;
#12935 = B_SPLINE_CURVE_WITH_KNOTS ( 'NONE', 3,
 ( #24244, #17009, #26547, #26391, #27036, #4549, #1918, #21446, #3900, #13925, #14565, #11939, #1763, #31800, #21774, #19308, #6531, #29333, #2085, #16855, #11447, #23920, #26875, #12112, #1431, #4387, #31961, #9483, #19479, #24568, #31481, #22102, #10460, #15380, #24905, #276 ),
 .UNSPECIFIED., .F., .F.,
 ( 4, 2, 2, 2, 2, 2, 2, 2, 2, 2, 2, 2, 2, 2, 2, 2, 2, 4 ),
 ( 0.000000000000000000, 0.0006656200208596486576, 0.001331240041719297315, 0.002662480083438598967, 0.003993720125157899752, 0.004659340146017551879, 0.005324960166877204006, 0.005990580187736854398, 0.006656200208596505657, 0.007987440250315808177, 0.009318680292035112431, 0.01064992033375441495, 0.01331240041719302172, 0.01464364045891232077, 0.01597488050063161982, 0.01863736058407022139, 0.01996860062578952391, 0.02129984066750881949 ),
 .UNSPECIFIED. ) ;
#12936 = CARTESIAN_POINT ( 'NONE',  ( 45.79384627280941089, 27.77957786121582018, 49.05938063676249072 ) ) ;
#12937 = DIRECTION ( 'NONE',  ( -0.2756373558169974980, 0.9612616959383193382, 1.315048337272770589E-17 ) ) ;
#12938 = DIRECTION ( 'NONE',  ( -1.101824276508909887E-16, 1.000000000000000000, -0.000000000000000000 ) ) ;
#12939 = EDGE_LOOP ( 'NONE', ( #18038, #11874, #14607, #23833 ) ) ;
#12940 = LINE ( 'NONE', #12786, #21919 ) ;
#12941 = EDGE_LOOP ( 'NONE', ( #28655, #20949, #10933, #30758 ) ) ;
#12942 = TOROIDAL_SURFACE ( 'NONE', #2954, 44.50000000000000000, 1.000000000000000000 ) ;
#12943 = DIRECTION ( 'NONE',  ( -0.000000000000000000, -1.000000000000000000, 0.000000000000000000 ) ) ;
#12944 = ORIENTED_EDGE ( 'NONE', *, *, #21005, .T. ) ;
#12945 = ORIENTED_EDGE ( 'NONE', *, *, #6930, .F. ) ;
#12946 = FACE_OUTER_BOUND ( 'NONE', #31416, .T. ) ;
#12947 = ORIENTED_EDGE ( 'NONE', *, *, #10772, .F. ) ;
#12948 = CIRCLE ( 'NONE', #9259, 21.50000000000000000 ) ;
#12949 = ADVANCED_FACE ( 'NONE', ( #10557 ), #28753, .T. ) ;
#12950 = EDGE_CURVE ( 'NONE', #26, #4564, #9379, .T. ) ;
#12951 = EDGE_CURVE ( 'NONE', #20780, #28878, #17762, .T. ) ;
#12952 = EDGE_CURVE ( 'NONE', #14341, #3694, #27176, .T. ) ;
#12953 = EDGE_LOOP ( 'NONE', ( #9261, #16654, #10841, #3901 ) ) ;
#12954 = ADVANCED_FACE ( 'NONE', ( #23175, #20547 ), #5303, .T. ) ;
#12955 = CARTESIAN_POINT ( 'NONE',  ( 21.09785597605719332, -5.935454207752198563, 47.04930799450051637 ) ) ;
#12956 = ADVANCED_FACE ( 'NONE', ( #20708 ), #13587, .T. ) ;
#12957 = ORIENTED_EDGE ( 'NONE', *, *, #5445, .T. ) ;
#12958 = CARTESIAN_POINT ( 'NONE',  ( -41.24971778908466291, 11.62557032131817358, 58.05249952744806308 ) ) ;
#12959 = DIRECTION ( 'NONE',  ( -1.101824276508909887E-16, 1.000000000000000000, -0.000000000000000000 ) ) ;
#12960 = CARTESIAN_POINT ( 'NONE',  ( 8.732853799281732776, 38.56284415653841791, 47.04930799450051637 ) ) ;
#12961 = CARTESIAN_POINT ( 'NONE',  ( 48.16694854572211426, 27.21789516297709355, 49.14507740233662503 ) ) ;
#12962 = ORIENTED_EDGE ( 'NONE', *, *, #31546, .F. ) ;
#12963 = VERTEX_POINT ( 'NONE', #3137 ) ;
#12964 = CARTESIAN_POINT ( 'NONE',  ( 8.474859994195281132, 32.34143805560860585, 47.04930799450051637 ) ) ;
#12965 = ORIENTED_EDGE ( 'NONE', *, *, #19998, .F. ) ;
#12966 = CARTESIAN_POINT ( 'NONE',  ( 46.86424029186792950, 10.39233698702945929, 98.46444777423641881 ) ) ;
#12967 = DIRECTION ( 'NONE',  ( -1.101824276508909887E-16, 1.000000000000000000, -0.000000000000000000 ) ) ;
#12968 = DIRECTION ( 'NONE',  ( -0.000000000000000000, -1.000000000000000000, 0.000000000000000000 ) ) ;
#12969 = DIRECTION ( 'NONE',  ( -1.101824276508909887E-16, 1.000000000000000000, -0.000000000000000000 ) ) ;
#12970 = DIRECTION ( 'NONE',  ( 1.000000000000000000, 0.000000000000000000, 0.000000000000000000 ) ) ;
#12971 = APPLICATION_PROTOCOL_DEFINITION ( 'draft international standard', 'automotive_design', 1998, #1750 ) ;
#12972 = ORIENTED_EDGE ( 'NONE', *, *, #20642, .T. ) ;
#12973 = CARTESIAN_POINT ( 'NONE',  ( 33.71785032049136532, 26.21664230456639899, 47.04930799450051637 ) ) ;
#12974 = CIRCLE ( 'NONE', #23431, 1.042135311067126979 ) ;
#12975 = DIRECTION ( 'NONE',  ( 0.7141240004913198547, -0.3958453973320100738, -0.5773502691896283956 ) ) ;
#12976 = DIRECTION ( 'NONE',  ( -1.000000000000000000, -1.101824276508909887E-16, 0.000000000000000000 ) ) ;
#12977 = DIRECTION ( 'NONE',  ( -1.000000000000000000, 0.000000000000000000, 0.000000000000000000 ) ) ;
#12978 = ORIENTED_EDGE ( 'NONE', *, *, #30706, .F. ) ;
#12979 = CARTESIAN_POINT ( 'NONE',  ( 33.72499318558949710, 25.59143805560860940, 47.04930799450051637 ) ) ;
#12980 = DIRECTION ( 'NONE',  ( -1.101824276508909887E-16, 1.000000000000000000, -0.000000000000000000 ) ) ;
#12981 = ADVANCED_FACE ( 'NONE', ( #5464 ), #27710, .T. ) ;
#12982 = CARTESIAN_POINT ( 'NONE',  ( 8.732853799281734553, 38.56284415653841791, 47.04930799450051637 ) ) ;
#12983 = ORIENTED_EDGE ( 'NONE', *, *, #19280, .F. ) ;
#12984 = ORIENTED_EDGE ( 'NONE', *, *, #4758, .F. ) ;
#12985 = EDGE_CURVE ( 'NONE', #3694, #14341, #9908, .T. ) ;
#12986 = ADVANCED_FACE ( 'NONE', ( #18232 ), #26128, .T. ) ;
#12987 = ORIENTED_EDGE ( 'NONE', *, *, #2813, .F. ) ;
#12988 = EDGE_CURVE ( 'NONE', #16322, #32074, #361, .T. ) ;
#12989 = CARTESIAN_POINT ( 'NONE',  ( 21.09785597605719332, 25.56454579224779167, 47.04930799450051637 ) ) ;
#12990 = AXIS2_PLACEMENT_3D ( 'NONE', #25638, #6260, #3139 ) ;
#12991 = CARTESIAN_POINT ( 'NONE',  ( -40.02540636251514172, 2.839176264122877047, 58.34930799450052064 ) ) ;
#12992 = CARTESIAN_POINT ( 'NONE',  ( 48.79980305660560447, 22.93328494799376571, 46.81390877062097644 ) ) ;
#12993 = CIRCLE ( 'NONE', #17157, 12.36707279061065101 ) ;
#12994 = ORIENTED_EDGE ( 'NONE', *, *, #24297, .F. ) ;
#12995 = CARTESIAN_POINT ( 'NONE',  ( -40.02540636251513462, 2.839176264122874382, 35.74930799450051921 ) ) ;
#12996 = CIRCLE ( 'NONE', #30794, 27.49999999999998934 ) ;
#12997 = DIRECTION ( 'NONE',  ( -0.000000000000000000, -1.000000000000000000, -0.000000000000000000 ) ) ;
#12998 = CARTESIAN_POINT ( 'NONE',  ( -40.28779227465695811, 2.984619150196779369, 55.54930799450051637 ) ) ;
#12999 = CARTESIAN_POINT ( 'NONE',  ( 33.46699938050304013, 38.56284415653841791, 47.04930799450051637 ) ) ;
#13000 = DIRECTION ( 'NONE',  ( 0.9612616959383193382, 0.2756373558169973870, 8.795445018804928853E-19 ) ) ;
#13001 = AXIS2_PLACEMENT_3D ( 'NONE', #4173, #14201, #6803 ) ;
#13002 = DIRECTION ( 'NONE',  ( -1.101824276508909887E-16, 1.000000000000000000, -0.000000000000000000 ) ) ;
#13003 = CARTESIAN_POINT ( 'NONE',  ( 21.09785597605719332, -16.63545420775219696, 126.2593585008393831 ) ) ;
#13004 = FACE_OUTER_BOUND ( 'NONE', #28868, .T. ) ;
#13005 = DIRECTION ( 'NONE',  ( -0.000000000000000000, -1.000000000000000000, 0.000000000000000000 ) ) ;
#13006 = CARTESIAN_POINT ( 'NONE',  ( -2.402144023942794249, 14.86454579224779948, 47.04930799450052348 ) ) ;
#13007 = LINE ( 'NONE', #15781, #27810 ) ;
#13008 = ORIENTED_EDGE ( 'NONE', *, *, #2811, .F. ) ;
#13009 = VERTEX_POINT ( 'NONE', #13180 ) ;
#13010 = CARTESIAN_POINT ( 'NONE',  ( 33.50134396954521065, 30.09164230456639544, 47.04930799450051637 ) ) ;
#13011 = DIRECTION ( 'NONE',  ( -1.000000000000000000, -1.101824276508909887E-16, 0.000000000000000000 ) ) ;
#13012 = CARTESIAN_POINT ( 'NONE',  ( 52.96898779464280693, 2.854128177266950672, 98.92834977772137961 ) ) ;
#13013 = VERTEX_POINT ( 'NONE', #26763 ) ;
#13014 = CARTESIAN_POINT ( 'NONE',  ( 33.46699938050304013, 30.97145308207317171, 47.04930799450050927 ) ) ;
#13015 = CARTESIAN_POINT ( 'NONE',  ( 47.65993751833249092, 23.10527845304106620, 47.07849978535075053 ) ) ;
#13016 = ORIENTED_EDGE ( 'NONE', *, *, #17874, .T. ) ;
#13017 = ORIENTED_EDGE ( 'NONE', *, *, #22571, .F. ) ;
#13018 = CARTESIAN_POINT ( 'NONE',  ( 21.09785597605720042, -13.37218737171702543, 102.7370144706720225 ) ) ;
#13019 = CARTESIAN_POINT ( 'NONE',  ( 48.18662509608405031, 26.58284706826093213, 49.18364984542562013 ) ) ;
#13020 = ADVANCED_FACE ( 'NONE', ( #16422 ), #4653, .F. ) ;
#13021 = AXIS2_PLACEMENT_3D ( 'NONE', #18360, #18524, #5743 ) ;
#13022 = ADVANCED_FACE ( 'NONE', ( #14298 ), #21173, .F. ) ;
#13023 = CARTESIAN_POINT ( 'NONE',  ( 48.94625023931840246, 28.07124452788248803, 46.10640627770150246 ) ) ;
#13024 = VECTOR ( 'NONE', #10778, 1000.000000000000114 ) ;
#13025 = CARTESIAN_POINT ( 'NONE',  ( -34.35545778780984705, 11.92558985988975806, 53.76626552113134494 ) ) ;
#13026 = AXIS2_PLACEMENT_3D ( 'NONE', #20373, #12699, #17434 ) ;
#13027 =( BOUNDED_CURVE ( )  B_SPLINE_CURVE ( 2, ( #31442, #29421, #12843, #35, #194 ),
 .UNSPECIFIED., .F., .F. ) 
 B_SPLINE_CURVE_WITH_KNOTS ( ( 3, 2, 3 ),
 ( 0.7921717258529592520, 0.8333333333333329263, 1.000000000000000000 ),
 .UNSPECIFIED. ) 
 CURVE ( )  GEOMETRIC_REPRESENTATION_ITEM ( )  RATIONAL_B_SPLINE_CURVE ( ( 0.9501679776138609590, 0.9669123415494011997, 1.000000000000000000, 0.8660254037844387076, 1.000000000000000000 ) ) 
 REPRESENTATION_ITEM ( '' )  );
#13028 = VECTOR ( 'NONE', #23455, 1000.000000000000000 ) ;
#13029 = AXIS2_PLACEMENT_3D ( 'NONE', #19218, #31874, #19388 ) ;
#13030 = ORIENTED_EDGE ( 'NONE', *, *, #5201, .F. ) ;
#13031 = EDGE_CURVE ( 'NONE', #19454, #5554, #32445, .T. ) ;
#13032 = CARTESIAN_POINT ( 'NONE',  ( 21.09992658989238734, 32.21664230456639899, 47.04930799450051637 ) ) ;
#13033 = DIRECTION ( 'NONE',  ( 0.000000000000000000, -1.000000000000000000, 0.000000000000000000 ) ) ;
#13034 = EDGE_LOOP ( 'NONE', ( #6181, #11865, #7998, #23001 ) ) ;
#13035 = DIRECTION ( 'NONE',  ( -0.9612616959383204485, -0.2756373558169933347, 1.660411357259282692E-16 ) ) ;
#13036 = CARTESIAN_POINT ( 'NONE',  ( 21.09785597605719332, 17.36451738380053555, 34.36516646732340519 ) ) ;
#13037 = CONICAL_SURFACE ( 'NONE', #23503, 15.23374605753642186, 1.187672012580060610 ) ;
#13038 = AXIS2_PLACEMENT_3D ( 'NONE', #2652, #20207, #27924 ) ;
#13039 = AXIS2_PLACEMENT_3D ( 'NONE', #657, #23141, #15276 ) ;
#13040 = ORIENTED_EDGE ( 'NONE', *, *, #13362, .T. ) ;
#13041 = DIRECTION ( 'NONE',  ( 0.000000000000000000, 0.000000000000000000, 1.000000000000000000 ) ) ;
#13042 = CARTESIAN_POINT ( 'NONE',  ( 21.09992658989238734, 38.56284415653841791, 47.04930799450051637 ) ) ;
#13043 = DIRECTION ( 'NONE',  ( -1.101824276508909887E-16, 1.000000000000000000, -0.000000000000000000 ) ) ;
#13044 = AXIS2_PLACEMENT_3D ( 'NONE', #15392, #10474, #18166 ) ;
#13045 = ADVANCED_FACE ( 'NONE', ( #1483 ), #11985, .T. ) ;
#13046 = CARTESIAN_POINT ( 'NONE',  ( 0.1396058544580265071, 11.92558985988972964, 99.69197238745105949 ) ) ;
#13047 = DIRECTION ( 'NONE',  ( 0.4544104193609903586, 0.000000000000000000, 0.8907924397839088737 ) ) ;
#13048 = ORIENTED_EDGE ( 'NONE', *, *, #29820, .T. ) ;
#13049 = CARTESIAN_POINT ( 'NONE',  ( 77.00054885935878701, -4.576799740321065180, 80.22553795869546889 ) ) ;
#13050 = DIRECTION ( 'NONE',  ( 0.1949050434465250392, -0.6797146636928682595, -0.7071067811865470176 ) ) ;
#13051 = CARTESIAN_POINT ( 'NONE',  ( 8.823509210239585343, 32.34164230456639899, 47.04930799450051637 ) ) ;
#13052 = EDGE_CURVE ( 'NONE', #11721, #6336, #16735, .T. ) ;
#13053 = CARTESIAN_POINT ( 'NONE',  ( 21.09785597605719332, 12.39166260509097484, -7.501994455397703376 ) ) ;
#13054 = AXIS2_PLACEMENT_3D ( 'NONE', #11674, #31695, #9206 ) ;
#13055 = CARTESIAN_POINT ( 'NONE',  ( 21.09992658989238734, 38.56284415653841791, 47.04930799450051637 ) ) ;
#13056 = ORIENTED_EDGE ( 'NONE', *, *, #17786, .T. ) ;
#13057 = DIRECTION ( 'NONE',  ( -1.000000000000000000, -1.101824276508909887E-16, 0.000000000000000000 ) ) ;
#13058 = FACE_OUTER_BOUND ( 'NONE', #23230, .T. ) ;
#13059 = VERTEX_POINT ( 'NONE', #8720 ) ;
#13060 = CARTESIAN_POINT ( 'NONE',  ( 21.09992658989239089, 30.46183152705961561, 47.04930799450051637 ) ) ;
#13061 = DIRECTION ( 'NONE',  ( 0.000000000000000000, 1.000000000000000000, -0.000000000000000000 ) ) ;
#13062 = EDGE_CURVE ( 'NONE', #18205, #16844, #23993, .T. ) ;
#13063 = ADVANCED_FACE ( 'NONE', ( #1323 ), #23530, .T. ) ;
#13064 = DIRECTION ( 'NONE',  ( -1.000000000000000000, 0.000000000000000000, 0.000000000000000000 ) ) ;
#13065 = LINE ( 'NONE', #10606, #1217 ) ;
#13066 = EDGE_CURVE ( 'NONE', #28361, #9250, #26596, .T. ) ;
#13067 = VERTEX_POINT ( 'NONE', #21332 ) ;
#13068 = DIRECTION ( 'NONE',  ( 2.779292025043186357E-18, -1.288349127009862211E-17, 1.000000000000000000 ) ) ;
#13069 = ORIENTED_EDGE ( 'NONE', *, *, #8134, .T. ) ;
#13070 = CIRCLE ( 'NONE', #10461, 12.27641737965286772 ) ;
#13071 = AXIS2_PLACEMENT_3D ( 'NONE', #14432, #24427, #26732 ) ;
#13072 = EDGE_LOOP ( 'NONE', ( #28018, #11734, #26058, #15009 ) ) ;
#13073 = AXIS2_PLACEMENT_3D ( 'NONE', #5094, #20337, #17888 ) ;
#13074 = ADVANCED_FACE ( 'NONE', ( #19198 ), #26438, .F. ) ;
#13075 = AXIS2_PLACEMENT_3D ( 'NONE', #17403, #4116, #32022 ) ;
#13076 = CARTESIAN_POINT ( 'NONE',  ( -41.77464577679392477, 3.808795504615560379, 45.04930799450051637 ) ) ;
#13077 = CARTESIAN_POINT ( 'NONE',  ( 81.46980107077142463, -5.935454207752202116, 16.07118271501079576 ) ) ;
#13078 = ORIENTED_EDGE ( 'NONE', *, *, #178, .F. ) ;
#13079 = ORIENTED_EDGE ( 'NONE', *, *, #17750, .T. ) ;
#13080 = CARTESIAN_POINT ( 'NONE',  ( -9.474781401982005136, 5.388785998227653806, 97.43646483284780402 ) ) ;
#13081 = DIRECTION ( 'NONE',  ( 0.000000000000000000, -0.000000000000000000, -1.000000000000000000 ) ) ;
#13082 = CARTESIAN_POINT ( 'NONE',  ( -37.03881032980826404, -5.627210490873816084, 79.10483057741561197 ) ) ;
#13083 = ADVANCED_FACE ( 'NONE', ( #26282 ), #28246, .T. ) ;
#13084 = DIRECTION ( 'NONE',  ( -0.000000000000000000, -1.000000000000000000, -0.000000000000000000 ) ) ;
#13085 = ORIENTED_EDGE ( 'NONE', *, *, #6937, .T. ) ;
#13086 = CARTESIAN_POINT ( 'NONE',  ( -11.12022268173655526, -5.523138741469210800, 104.1124227880728768 ) ) ;
#13087 = ORIENTED_EDGE ( 'NONE', *, *, #17857, .T. ) ;
#13088 = CARTESIAN_POINT ( 'NONE',  ( 21.09785597605720042, 13.06454579224780055, 101.7935565934706261 ) ) ;
#13089 = DIRECTION ( 'NONE',  ( 0.000000000000000000, 0.000000000000000000, 1.000000000000000000 ) ) ;
#13090 = VECTOR ( 'NONE', #4222, 1000.000000000000000 ) ;
#13091 = ORIENTED_EDGE ( 'NONE', *, *, #17568, .T. ) ;
#13092 = CARTESIAN_POINT ( 'NONE',  ( -40.02540636251514172, 2.839176264122877047, 59.04930799450051637 ) ) ;
#13093 = CIRCLE ( 'NONE', #21956, 1.524998423334080533 ) ;
#13094 = EDGE_CURVE ( 'NONE', #16672, #63, #14611, .T. ) ;
#13095 = DIRECTION ( 'NONE',  ( -1.000000000000000000, 0.000000000000000000, 0.000000000000000000 ) ) ;
#13096 = DIRECTION ( 'NONE',  ( 0.000000000000000000, -0.000000000000000000, -1.000000000000000000 ) ) ;
#13097 = LINE ( 'NONE', #13569, #27438 ) ;
#13098 = DIRECTION ( 'NONE',  ( -1.000000000000000000, 0.000000000000000000, 0.000000000000000000 ) ) ;
#13099 = DIRECTION ( 'NONE',  ( -1.000000000000000000, 0.000000000000000000, 0.000000000000000000 ) ) ;
#13100 = CARTESIAN_POINT ( 'NONE',  ( 21.09992658989238734, 30.84143805560860585, 47.04930799450051637 ) ) ;
#13101 = ORIENTED_EDGE ( 'NONE', *, *, #15890, .F. ) ;
#13102 = FACE_OUTER_BOUND ( 'NONE', #6201, .T. ) ;
#13103 = ADVANCED_FACE ( 'NONE', ( #21497, #24134, #6097, #1652 ), #24035, .T. ) ;
#13104 = VECTOR ( 'NONE', #27296, 1000.000000000000000 ) ;
#13105 = CIRCLE ( 'NONE', #32486, 0.1250000000000001110 ) ;
#13106 = CARTESIAN_POINT ( 'NONE',  ( -42.38687957179149635, 4.148162238787999279, 37.04930799450052348 ) ) ;
#13107 = EDGE_CURVE ( 'NONE', #1328, #31727, #22985, .T. ) ;
#13108 = ORIENTED_EDGE ( 'NONE', *, *, #22863, .T. ) ;
#13109 = AXIS2_PLACEMENT_3D ( 'NONE', #7694, #2597, #30182 ) ;
#13110 = ORIENTED_EDGE ( 'NONE', *, *, #31465, .T. ) ;
#13111 = AXIS2_PLACEMENT_3D ( 'NONE', #13060, #23220, #17965 ) ;
#13112 = ORIENTED_EDGE ( 'NONE', *, *, #29432, .F. ) ;
#13113 = EDGE_LOOP ( 'NONE', ( #13981, #31197, #11758, #11762 ) ) ;
#13114 = CARTESIAN_POINT ( 'NONE',  ( 71.49893360114315044, 9.702389020015065313, 20.34850893876554778 ) ) ;
#13115 = AXIS2_PLACEMENT_3D ( 'NONE', #3422, #15737, #20659 ) ;
#13116 = AXIS2_PLACEMENT_3D ( 'NONE', #25616, #28567, #18211 ) ;
#13117 = EDGE_LOOP ( 'NONE', ( #20273, #28247, #27892, #14080, #15517 ) ) ;
#13118 = CARTESIAN_POINT ( 'NONE',  ( 48.72149481846882679, 22.88065857334295217, 48.10262368218729279 ) ) ;
#13119 = AXIS2_PLACEMENT_3D ( 'NONE', #18329, #18494, #5709 ) ;
#13120 = LINE ( 'NONE', #30834, #4995 ) ;
#13121 = DIRECTION ( 'NONE',  ( 0.4544104193609915243, 0.000000000000000000, 0.8907924397839082076 ) ) ;
#13122 = CARTESIAN_POINT ( 'NONE',  ( 46.02876340639226527, 27.56789516297709497, 44.95353858666495483 ) ) ;
#13123 = CIRCLE ( 'NONE', #15278, 25.00000000000000000 ) ;
#13124 = CIRCLE ( 'NONE', #22543, 48.97546517713167447 ) ;
#13125 = ORIENTED_EDGE ( 'NONE', *, *, #16222, .F. ) ;
#13126 = VERTEX_POINT ( 'NONE', #9859 ) ;
#13127 = CARTESIAN_POINT ( 'NONE',  ( 21.09785597605720042, -13.88867167006704939, -11.65212399594570769 ) ) ;
#13128 = ORIENTED_EDGE ( 'NONE', *, *, #24154, .F. ) ;
#13129 = CARTESIAN_POINT ( 'NONE',  ( 33.50134396954526039, 25.34164230456639899, 47.04930799450051637 ) ) ;
#13130 = CARTESIAN_POINT ( 'NONE',  ( 54.82846636219741754, -2.304636120132642407, 102.0807631826289565 ) ) ;
#13131 = DIRECTION ( 'NONE',  ( -1.101824276508909887E-16, 1.000000000000000000, -0.000000000000000000 ) ) ;
#13132 = DIRECTION ( 'NONE',  ( 0.9612616959383205595, 0.2756373558169932236, -1.660411357259282445E-16 ) ) ;
#13133 = CARTESIAN_POINT ( 'NONE',  ( 8.474859994195286461, 26.59184655352419568, 47.04930799450051637 ) ) ;
#13134 = ORIENTED_EDGE ( 'NONE', *, *, #4371, .T. ) ;
#13135 = CARTESIAN_POINT ( 'NONE',  ( -43.73393778030726509, 1.305471833569777695, 60.44930799450051495 ) ) ;
#13136 = CIRCLE ( 'NONE', #25193, 0.1250000000000001110 ) ;
#13137 = DIRECTION ( 'NONE',  ( -0.2756373558169954441, 0.9612616959383198934, -1.479773560108263451E-16 ) ) ;
#13138 = ADVANCED_FACE ( 'NONE', ( #4443 ), #17219, .T. ) ;
#13139 = DIRECTION ( 'NONE',  ( -0.000000000000000000, -1.000000000000000000, 0.000000000000000000 ) ) ;
#13140 = DIRECTION ( 'NONE',  ( -0.9612616959383207815, -0.2756373558169926685, -8.795445018804289444E-19 ) ) ;
#13141 = ORIENTED_EDGE ( 'NONE', *, *, #24671, .T. ) ;
#13142 = DIRECTION ( 'NONE',  ( 0.000000000000000000, -1.000000000000000000, 0.000000000000000000 ) ) ;
#13143 = DIRECTION ( 'NONE',  ( -1.000000000000000000, 0.000000000000000000, 0.000000000000000000 ) ) ;
#13144 = CIRCLE ( 'NONE', #32, 12.36707279061065101 ) ;
#13145 = CARTESIAN_POINT ( 'NONE',  ( -43.43257085947613660, 1.024086014757300989, 53.64930799450051779 ) ) ;
#13146 = ORIENTED_EDGE ( 'NONE', *, *, #11166, .T. ) ;
#13147 = CIRCLE ( 'NONE', #28850, 0.9031915329475519449 ) ;
#13148 = AXIS2_PLACEMENT_3D ( 'NONE', #29082, #4128, #11691 ) ;
#13149 = AXIS2_PLACEMENT_3D ( 'NONE', #29727, #12167, #14794 ) ;
#13150=STYLED_ITEM('',(#32522),#12396);
#13151 = ORIENTED_EDGE ( 'NONE', *, *, #1114, .T. ) ;
#13152 = ORIENTED_EDGE ( 'NONE', *, *, #9865, .F. ) ;
#13153 = CYLINDRICAL_SURFACE ( 'NONE', #7581, 2.500000000000002220 ) ;
#13154 = DIRECTION ( 'NONE',  ( -1.000000000000000000, 0.000000000000000000, 0.000000000000000000 ) ) ;
#13155 = DIRECTION ( 'NONE',  ( -0.000000000000000000, -1.000000000000000000, -0.000000000000000000 ) ) ;
#13156 = AXIS2_PLACEMENT_3D ( 'NONE', #23165, #25469, #13333 ) ;
#13157 = VERTEX_POINT ( 'NONE', #26927 ) ;
#13158 = CARTESIAN_POINT ( 'NONE',  ( -38.65545646816406133, 11.23353054871637013, 71.85461326257689052 ) ) ;
#13159 = CARTESIAN_POINT ( 'NONE',  ( 33.46699938050303302, 38.56284415653841791, 47.04930799450051637 ) ) ;
#13160 = LINE ( 'NONE', #13327, #2768 ) ;
#13161 = CARTESIAN_POINT ( 'NONE',  ( 52.31884008669100439, -5.919445383190008236, -10.81522751587263720 ) ) ;
#13162 = VECTOR ( 'NONE', #30284, 999.9999999999998863 ) ;
#13163 = DIRECTION ( 'NONE',  ( 0.000000000000000000, 0.000000000000000000, -1.000000000000000000 ) ) ;
#13164 = DIRECTION ( 'NONE',  ( 0.000000000000000000, 1.000000000000000000, -0.000000000000000000 ) ) ;
#13165 = FACE_OUTER_BOUND ( 'NONE', #26662, .T. ) ;
#13166 = CARTESIAN_POINT ( 'NONE',  ( 48.99461295342375422, 29.56774068890345930, 46.14022547996226820 ) ) ;
#13167 = FACE_OUTER_BOUND ( 'NONE', #11318, .T. ) ;
#13168 = AXIS2_PLACEMENT_3D ( 'NONE', #25910, #8833, #30848 ) ;
#13169 = AXIS2_PLACEMENT_3D ( 'NONE', #19389, #16763, #17252 ) ;
#13170 = CARTESIAN_POINT ( 'NONE',  ( -42.38687957179150345, 4.148162238788004608, 59.04930799450051637 ) ) ;
#13171 = CARTESIAN_POINT ( 'NONE',  ( 44.09250526802607340, 29.45621246473837118, 46.89322480343881949 ) ) ;
#13172 = CIRCLE ( 'NONE', #9479, 0.1250000000000001110 ) ;
#13173 =( LENGTH_UNIT ( ) NAMED_UNIT ( * ) SI_UNIT ( .MILLI., .METRE. ) );
#13174 = ORIENTED_EDGE ( 'NONE', *, *, #28797, .F. ) ;
#13175 = ORIENTED_EDGE ( 'NONE', *, *, #14839, .T. ) ;
#13176 = LINE ( 'NONE', #8242, #13953 ) ;
#13177 = CIRCLE ( 'NONE', #7926, 0.1000000000000006301 ) ;
#13178 = DIRECTION ( 'NONE',  ( -1.101824276508909887E-16, 1.000000000000000000, -0.000000000000000000 ) ) ;
#13179 = EDGE_CURVE ( 'NONE', #5971, #30781, #7067, .T. ) ;
#13180 = CARTESIAN_POINT ( 'NONE',  ( 21.09785597605720042, -13.59284023713420630, -8.574624342367267005 ) ) ;
#13181 = EDGE_CURVE ( 'NONE', #3549, #4111, #3071, .T. ) ;
#13182 = EDGE_CURVE ( 'NONE', #7606, #25631, #2559, .T. ) ;
#13183 = ORIENTED_EDGE ( 'NONE', *, *, #7759, .F. ) ;
#13184 = LINE ( 'NONE', #21175, #7213 ) ;
#13185 = CARTESIAN_POINT ( 'NONE',  ( -40.02353495282824980, 6.996741953892005483, 39.48683338133720611 ) ) ;
#13186 = ADVANCED_FACE ( 'NONE', ( #27580 ), #7404, .F. ) ;
#13187 = ORIENTED_EDGE ( 'NONE', *, *, #6836, .F. ) ;
#13188 = ORIENTED_EDGE ( 'NONE', *, *, #21958, .T. ) ;
#13189 = DIRECTION ( 'NONE',  ( 1.000000000000000000, 0.000000000000000000, 0.000000000000000000 ) ) ;
#13190 = ADVANCED_FACE ( 'NONE', ( #24299 ), #1496, .T. ) ;
#13191 = CARTESIAN_POINT ( 'NONE',  ( 46.99023568444673060, 27.22451373492759785, 49.12151524109405898 ) ) ;
#13192 = CIRCLE ( 'NONE', #22086, 46.09082119073493544 ) ;
#13193 = CARTESIAN_POINT ( 'NONE',  ( 44.70507715278255745, 27.66291119454915304, 46.92503878583764987 ) ) ;
#13194 = CARTESIAN_POINT ( 'NONE',  ( -34.60695214214126736, 11.63096289306646902, 52.99612787234249822 ) ) ;
#13195 = EDGE_LOOP ( 'NONE', ( #18318, #17304, #10575, #13457 ) ) ;
#13196 = TOROIDAL_SURFACE ( 'NONE', #9528, 12.40141737965288371, 0.1249999999999996253 ) ;
#13197 = CIRCLE ( 'NONE', #27337, 1.624998423334082620 ) ;
#13198 = LINE ( 'NONE', #11048, #3572 ) ;
#13199 = DIRECTION ( 'NONE',  ( 0.000000000000000000, -0.000000000000000000, -1.000000000000000000 ) ) ;
#13200 = CIRCLE ( 'NONE', #30490, 0.1000000000000037248 ) ;
#13201 = ORIENTED_EDGE ( 'NONE', *, *, #6901, .F. ) ;
#13202 = VECTOR ( 'NONE', #11261, 1000.000000000000000 ) ;
#13203 = CARTESIAN_POINT ( 'NONE',  ( 21.09785597605720753, 14.66454579224780019, 47.04930799450052348 ) ) ;
#13204 = DIRECTION ( 'NONE',  ( 0.000000000000000000, 0.000000000000000000, -1.000000000000000000 ) ) ;
#13205 = EDGE_CURVE ( 'NONE', #32001, #1884, #5710, .T. ) ;
#13206 = CIRCLE ( 'NONE', #11122, 24.99999999999999645 ) ;
#13207 = CARTESIAN_POINT ( 'NONE',  ( -40.44300931641782171, 7.361061430353638357, 60.31640775708849844 ) ) ;
#13208 = EDGE_CURVE ( 'NONE', #14178, #24256, #16700, .T. ) ;
#13209 = VERTEX_POINT ( 'NONE', #22477 ) ;
#13210 = CARTESIAN_POINT ( 'NONE',  ( -41.01929587258828036, 9.401204285752060130, 38.64930799450052490 ) ) ;
#13211 = LINE ( 'NONE', #28138, #10493 ) ;
#13212 = CARTESIAN_POINT ( 'NONE',  ( -40.28779227465695101, 2.984619150196775816, 37.04930799450052348 ) ) ;
#13213 = FACE_OUTER_BOUND ( 'NONE', #19322, .T. ) ;
#13214 = CARTESIAN_POINT ( 'NONE',  ( -40.69571722278731585, 6.786566810383049209, 39.44930799450052206 ) ) ;
#13215 = VERTEX_POINT ( 'NONE', #2471 ) ;
#13216 = DIRECTION ( 'NONE',  ( -1.101824276508909887E-16, 1.000000000000000000, -0.000000000000000000 ) ) ;
#13217 = DIRECTION ( 'NONE',  ( 0.000000000000000000, -1.000000000000000000, 0.000000000000000000 ) ) ;
#13218 = CARTESIAN_POINT ( 'NONE',  ( -40.46271621608484281, 3.081581074246049212, 55.54930799450051637 ) ) ;
#13219 = CARTESIAN_POINT ( 'NONE',  ( 21.09785597605720753, 13.86454579224779948, 47.04930799450052348 ) ) ;
#13220 = FACE_OUTER_BOUND ( 'NONE', #19987, .T. ) ;
#13221 = VECTOR ( 'NONE', #14399, 1000.000000000000000 ) ;
#13222 = EDGE_LOOP ( 'NONE', ( #30783, #10968, #8506, #24020 ) ) ;
#13223 = CONICAL_SURFACE ( 'NONE', #3244, 15.23374605753642186, 1.187672012580060610 ) ;
#13224 = CARTESIAN_POINT ( 'NONE',  ( 47.16621377848951369, 29.60751587792711348, 44.99339554510944339 ) ) ;
#13225 = CARTESIAN_POINT ( 'NONE',  ( 21.09785597605719332, 40.56454579224780588, 47.04930799450051637 ) ) ;
#13226 = PLANE ( 'NONE',  #1239 ) ;
#13227 = ORIENTED_EDGE ( 'NONE', *, *, #13494, .F. ) ;
#13228 = CARTESIAN_POINT ( 'NONE',  ( -42.47434154250543514, 4.196643200812633978, 35.74930799450051921 ) ) ;
#13229 = EDGE_CURVE ( 'NONE', #11324, #7112, #1974, .T. ) ;
#13230 = CARTESIAN_POINT ( 'NONE',  ( -41.02113223168485234, 7.230835263863471418, 34.54930799450052348 ) ) ;
#13231 = CARTESIAN_POINT ( 'NONE',  ( 8.698509210239537381, 27.09164230456639899, 47.04930799450051637 ) ) ;
#13232 = CARTESIAN_POINT ( 'NONE',  ( 8.474859994195286461, 29.84143805560861296, 47.04930799450051637 ) ) ;
#13233 = EDGE_LOOP ( 'NONE', ( #24121, #14514, #32128, #26651 ) ) ;
#13234 = CARTESIAN_POINT ( 'NONE',  ( 48.72149481846882679, 22.88065857334295217, 48.10262368218729279 ) ) ;
#13235 = VERTEX_POINT ( 'NONE', #29722 ) ;
#13236 = AXIS2_PLACEMENT_3D ( 'NONE', #23889, #11584, #28656 ) ;
#13237 = ORIENTED_EDGE ( 'NONE', *, *, #13854, .F. ) ;
#13238 = VECTOR ( 'NONE', #10454, 1000.000000000000000 ) ;
#13239 = EDGE_CURVE ( 'NONE', #665, #2312, #19326, .T. ) ;
#13241 = EDGE_CURVE ( 'NONE', #6908, #19822, #9368, .T. ) ;
#13240 = AXIS2_PLACEMENT_3D ( 'NONE', #27566, #25104, #12477 ) ;
#13242 = AXIS2_PLACEMENT_3D ( 'NONE', #12289, #26889, #4733 ) ;
#13243 = FACE_OUTER_BOUND ( 'NONE', #5897, .T. ) ;
#13244 = CARTESIAN_POINT ( 'NONE',  ( -40.18454328187963398, 7.548069831825862330, 60.54930799450051637 ) ) ;
#13245 = DIRECTION ( 'NONE',  ( -1.101824276508909887E-16, 1.000000000000000000, -0.000000000000000000 ) ) ;
#13246 = EDGE_CURVE ( 'NONE', #23906, #10175, #14621, .T. ) ;
#13247 = EDGE_CURVE ( 'NONE', #5204, #12078, #19530, .T. ) ;
#13248 = ORIENTED_EDGE ( 'NONE', *, *, #6557, .T. ) ;
#13249 = CARTESIAN_POINT ( 'NONE',  ( -34.95900968110382223, 11.10530621426302034, 41.68526607318150212 ) ) ;
#13250 = EDGE_LOOP ( 'NONE', ( #12571, #19731, #13379, #7417 ) ) ;
#13251 = CARTESIAN_POINT ( 'NONE',  ( 21.09992658989239089, 26.97145308207318948, 47.04930799450051637 ) ) ;
#13252 = DIRECTION ( 'NONE',  ( -1.101824276508909887E-16, 1.000000000000000000, -0.000000000000000000 ) ) ;
#13253 = DIRECTION ( 'NONE',  ( -0.8746197071393790878, 0.4848096202463673676, 1.277302113040196197E-17 ) ) ;
#13254 = VERTEX_POINT ( 'NONE', #12327 ) ;
#13255 = CARTESIAN_POINT ( 'NONE',  ( -40.49096175631598271, 7.521145078229855230, 60.14930799450051779 ) ) ;
#13256 = ORIENTED_EDGE ( 'NONE', *, *, #31584, .F. ) ;
#13257 = DIRECTION ( 'NONE',  ( -1.224646799147353207E-16, -1.349345573449484691E-32, 1.000000000000000000 ) ) ;
#13258 = CARTESIAN_POINT ( 'NONE',  ( 8.732853799281734553, 38.56284415653841791, 47.04930799450051637 ) ) ;
#13259 = ORIENTED_EDGE ( 'NONE', *, *, #30953, .F. ) ;
#13260 = DIRECTION ( 'NONE',  ( 0.9996573249755574819, 1.344306794811909066E-16, -0.02617694830786587712 ) ) ;
#13261 = DIRECTION ( 'NONE',  ( -1.000000000000000000, 0.000000000000000000, 0.000000000000000000 ) ) ;
#13262 = FACE_OUTER_BOUND ( 'NONE', #3462, .T. ) ;
#13263 = CARTESIAN_POINT ( 'NONE',  ( 21.09992658989238734, 32.47145308207317527, 47.04930799450051637 ) ) ;
#13264 = AXIS2_PLACEMENT_3D ( 'NONE', #7555, #4764, #15098 ) ;
#13265 = DIRECTION ( 'NONE',  ( 0.000000000000000000, 0.000000000000000000, 1.000000000000000000 ) ) ;
#13266 = FACE_OUTER_BOUND ( 'NONE', #8919, .T. ) ;
#13267 = DIRECTION ( 'NONE',  ( 0.000000000000000000, 0.000000000000000000, -1.000000000000000000 ) ) ;
#13268 = CIRCLE ( 'NONE', #8028, 58.66319174311612272 ) ;
#13269 = VERTEX_POINT ( 'NONE', #4600 ) ;
#13270 = EDGE_CURVE ( 'NONE', #26491, #30456, #20023, .T. ) ;
#13271 = CARTESIAN_POINT ( 'NONE',  ( 21.09785597605720753, 13.86454579224779948, 47.04930799450052348 ) ) ;
#13272 = AXIS2_PLACEMENT_3D ( 'NONE', #28687, #6202, #18983 ) ;
#13273 = VERTEX_POINT ( 'NONE', #24625 ) ;
#13274 = AXIS2_PLACEMENT_3D ( 'NONE', #15882, #30818, #23425 ) ;
#13275 = EDGE_LOOP ( 'NONE', ( #16629, #5188, #4325, #7697 ) ) ;
#13276 = CARTESIAN_POINT ( 'NONE',  ( -8.419250967200506253, 6.662067023026856383, 98.79925651794950170 ) ) ;
#13277 = ORIENTED_EDGE ( 'NONE', *, *, #4584, .T. ) ;
#13278 = EDGE_CURVE ( 'NONE', #1764, #5962, #12162, .T. ) ;
#13279 = EDGE_CURVE ( 'NONE', #23862, #17110, #5731, .T. ) ;
#13280 = AXIS2_PLACEMENT_3D ( 'NONE', #10676, #23610, #20661 ) ;
#13281 = PRODUCT ( 'Frame', 'Frame', '', ( #162 ) ) ;
#13282 = EDGE_LOOP ( 'NONE', ( #8188, #31002, #31817, #16248 ) ) ;
#13283 = DIRECTION ( 'NONE',  ( 8.969280666154383504E-16, 0.000000000000000000, -1.000000000000000000 ) ) ;
#13284 = ADVANCED_FACE ( 'NONE', ( #2309, #22322 ), #20829, .F. ) ;
#13285 = ORIENTED_EDGE ( 'NONE', *, *, #31620, .F. ) ;
#13286 = EDGE_CURVE ( 'NONE', #22149, #30896, #7817, .T. ) ;
#13287 = CARTESIAN_POINT ( 'NONE',  ( 48.39051051835283346, 22.95310733321322516, 48.05892087412300384 ) ) ;
#13288 = CIRCLE ( 'NONE', #26382, 12.62506659569710266 ) ;
#13289 = AXIS2_PLACEMENT_3D ( 'NONE', #31010, #23614, #13774 ) ;
#13290 = CARTESIAN_POINT ( 'NONE',  ( 33.72499318558949710, 32.34143805560860585, 47.04930799450051637 ) ) ;
#13291 = CARTESIAN_POINT ( 'NONE',  ( 8.474859994195281132, 31.84184655352418503, 47.04930799450051637 ) ) ;
#13292 = CARTESIAN_POINT ( 'NONE',  ( 49.44739180854976013, 28.03456182964376708, 47.17133137409169308 ) ) ;
#13293 = ORIENTED_EDGE ( 'NONE', *, *, #16110, .F. ) ;
#13294 = EDGE_LOOP ( 'NONE', ( #28424, #18880, #31670, #15195 ) ) ;
#13295 = SURFACE_STYLE_USAGE ( .BOTH. , #8196 ) ;
#13296 = ORIENTED_EDGE ( 'NONE', *, *, #30630, .F. ) ;
#13297 = FACE_OUTER_BOUND ( 'NONE', #19924, .T. ) ;
#13298 = FACE_OUTER_BOUND ( 'NONE', #29901, .T. ) ;
#13299 = CARTESIAN_POINT ( 'NONE',  ( -41.88090303775678080, 13.82677487427665675, 59.54930799450050927 ) ) ;
#13300 = CARTESIAN_POINT ( 'NONE',  ( -40.48129536610376533, 8.613360132207176889, 39.44930799450052206 ) ) ;
#13301 = CARTESIAN_POINT ( 'NONE',  ( -21.90214402394279603, 13.86454579224779948, 47.04930799450052348 ) ) ;
#13302 = ORIENTED_EDGE ( 'NONE', *, *, #19378, .T. ) ;
#13303 = CARTESIAN_POINT ( 'NONE',  ( 21.09785597605720753, 13.68462854903246573, 47.04930799450052348 ) ) ;
#13304 = DIRECTION ( 'NONE',  ( 0.000000000000000000, 1.000000000000000000, 0.000000000000000000 ) ) ;
#13305 = FACE_OUTER_BOUND ( 'NONE', #28707, .T. ) ;
#13306 = AXIS2_PLACEMENT_3D ( 'NONE', #19113, #21259, #13735 ) ;
#13307 = FACE_OUTER_BOUND ( 'NONE', #20543, .T. ) ;
#13308 = AXIS2_PLACEMENT_3D ( 'NONE', #5450, #2335, #7589 ) ;
#13309 = ORIENTED_EDGE ( 'NONE', *, *, #19599, .F. ) ;
#13310 = CARTESIAN_POINT ( 'NONE',  ( 100.3079064823960493, -15.93545420775219945, 44.54930799450134771 ) ) ;
#13311 = CARTESIAN_POINT ( 'NONE',  ( 21.09992658989239089, 27.09164230456639899, 47.04930799450051637 ) ) ;
#13312 = ORIENTED_EDGE ( 'NONE', *, *, #5037, .T. ) ;
#13313 = CIRCLE ( 'NONE', #28512, 12.36707279061065101 ) ;
#13314 = AXIS2_PLACEMENT_3D ( 'NONE', #10472, #17844, #27375 ) ;
#13315 = EDGE_CURVE ( 'NONE', #27037, #31589, #26150, .T. ) ;
#13316 = ORIENTED_EDGE ( 'NONE', *, *, #2110, .T. ) ;
#13317 = ORIENTED_EDGE ( 'NONE', *, *, #32117, .F. ) ;
#13318 = CARTESIAN_POINT ( 'NONE',  ( -40.65487266620045403, 9.475231293617264683, 38.63717596014456035 ) ) ;
#13319 = CARTESIAN_POINT ( 'NONE',  ( 21.09992658989239089, 25.46664230456640254, 47.04930799450051637 ) ) ;
#13320 = FACE_OUTER_BOUND ( 'NONE', #9110, .T. ) ;
#13321 = EDGE_CURVE ( 'NONE', #8764, #20587, #17772, .T. ) ;
#13322 = AXIS2_PLACEMENT_3D ( 'NONE', #18890, #26612, #1989 ) ;
#13323 = ORIENTED_EDGE ( 'NONE', *, *, #7613, .F. ) ;
#13324 = EDGE_CURVE ( 'NONE', #22091, #22386, #19283, .T. ) ;
#13325 = DIRECTION ( 'NONE',  ( 0.2756373558169954441, -0.9612616959383198934, 5.348665517716782531E-31 ) ) ;
#13326 = CARTESIAN_POINT ( 'NONE',  ( 81.63177831856063449, -5.935454207752202116, 16.07118271501079576 ) ) ;
#13327 = CARTESIAN_POINT ( 'NONE',  ( 21.09785597605720042, -13.98292989133646103, 105.7214871010043709 ) ) ;
#13328 = FACE_OUTER_BOUND ( 'NONE', #2980, .T. ) ;
#13329 = CARTESIAN_POINT ( 'NONE',  ( -63.90214402394282445, -5.935454207752198563, 54.04930799450053058 ) ) ;
#13330 = CARTESIAN_POINT ( 'NONE',  ( 21.09992658989238734, 31.21664230456641675, 47.04930799450051637 ) ) ;
#13332 = AXIS2_PLACEMENT_3D ( 'NONE', #10800, #13573, #28354 ) ;
#13331 = CARTESIAN_POINT ( 'NONE',  ( -40.80097511801616150, 8.246641009394465982, 54.44930799450051495 ) ) ;
#13333 = DIRECTION ( 'NONE',  ( -1.000000000000000000, 0.000000000000000000, 0.000000000000000000 ) ) ;
#13334 = CYLINDRICAL_SURFACE ( 'NONE', #2661, 2.000000000000001776 ) ;
#13335 = DIRECTION ( 'NONE',  ( -0.8746197071393858602, 0.4848096202463547666, 0.000000000000000000 ) ) ;
#13336 = VERTEX_POINT ( 'NONE', #23301 ) ;
#13337 = ORIENTED_EDGE ( 'NONE', *, *, #6435, .T. ) ;
#13338 = CARTESIAN_POINT ( 'NONE',  ( 71.26428788917345969, -13.30632128221581212, 71.78284114260775084 ) ) ;
#13339 = CARTESIAN_POINT ( 'NONE',  ( 54.06624571392757161, 0.6013300790671899376, 99.71667309011171199 ) ) ;
#13340 = EDGE_LOOP ( 'NONE', ( #15127, #11169, #19897, #25747 ) ) ;
#13341 = CARTESIAN_POINT ( 'NONE',  ( 21.09785597605720753, 14.86454579224779948, 47.04930799450052348 ) ) ;
#13342 = CARTESIAN_POINT ( 'NONE',  ( -40.16503835899720087, 7.510440877657823755, 38.80028690913361800 ) ) ;
#13343 = VERTEX_POINT ( 'NONE', #2945 ) ;
#13344 = CARTESIAN_POINT ( 'NONE',  ( -40.02540636251513462, 2.839176264122873050, 35.04930799450051637 ) ) ;
#13345 = CARTESIAN_POINT ( 'NONE',  ( 46.96268396749378127, 29.63121246473836834, 49.65201805493727960 ) ) ;
#13346 = CARTESIAN_POINT ( 'NONE',  ( 46.99023568444673060, 27.83791119454915375, 49.12151524109405898 ) ) ;
#13347 = CARTESIAN_POINT ( 'NONE',  ( -39.42933158985913877, -5.935956174194163104, 77.90091477773695772 ) ) ;
#13348 = AXIS2_PLACEMENT_3D ( 'NONE', #6276, #16597, #3975 ) ;
#13349 = AXIS2_PLACEMENT_3D ( 'NONE', #5042, #19960, #24237 ) ;
#13350 = AXIS2_PLACEMENT_3D ( 'NONE', #2000, #26464, #26788 ) ;
#13351 = ORIENTED_EDGE ( 'NONE', *, *, #27505, .F. ) ;
#13352 = DIRECTION ( 'NONE',  ( 0.2756373558170140403, -0.9612616959383146753, -1.315048337272768740E-17 ) ) ;
#13353 = CARTESIAN_POINT ( 'NONE',  ( 21.09785597605718621, 7.237299147902269247, 66.50898490448155087 ) ) ;
#13354 = EDGE_CURVE ( 'NONE', #23633, #23532, #20340, .T. ) ;
#13355 = ORIENTED_EDGE ( 'NONE', *, *, #31507, .T. ) ;
#13356 = ADVANCED_FACE ( 'NONE', ( #7888 ), #9405, .T. ) ;
#13357 = ADVANCED_FACE ( 'NONE', ( #25284 ), #30699, .F. ) ;
#13358 = ADVANCED_FACE ( 'NONE', ( #2632 ), #13603, .T. ) ;
#13359 = ADVANCED_FACE ( 'NONE', ( #8208 ), #22488, .T. ) ;
#13360 = FACE_OUTER_BOUND ( 'NONE', #15184, .T. ) ;
#13361 = CARTESIAN_POINT ( 'NONE',  ( -63.90214402394282445, 9.925589859889720756, 42.04930799450051637 ) ) ;
#13362 = EDGE_CURVE ( 'NONE', #21602, #90, #10444, .T. ) ;
#13363 = FACE_OUTER_BOUND ( 'NONE', #24367, .T. ) ;
#13364 = VERTEX_POINT ( 'NONE', #10514 ) ;
#13365 = DIRECTION ( 'NONE',  ( -0.9612616959383207815, -0.2756373558169926685, -8.795445018804291370E-19 ) ) ;
#13366 = CARTESIAN_POINT ( 'NONE',  ( 21.09992658989239089, 26.09184655352419213, 47.04930799450051637 ) ) ;
#13367 = AXIS2_PLACEMENT_3D ( 'NONE', #23156, #15599, #5443 ) ;
#13368 = CARTESIAN_POINT ( 'NONE',  ( -3.659396493201523270, 10.95165879486606997, -3.626357375625654633 ) ) ;
#13369 = AXIS2_PLACEMENT_3D ( 'NONE', #28099, #507, #2968 ) ;
#13370 = ORIENTED_EDGE ( 'NONE', *, *, #29043, .T. ) ;
#13371 = CARTESIAN_POINT ( 'NONE',  ( 46.69388217747229675, 23.10527865767145173, 46.62354503484363022 ) ) ;
#13372 = CARTESIAN_POINT ( 'NONE',  ( 0.6836613156275053171, 11.92558985988973497, -4.944603100128008855 ) ) ;
#13373 = TOROIDAL_SURFACE ( 'NONE', #22248, 13.50178401536290806, 0.5000000000000002220 ) ;
#13374 = CIRCLE ( 'NONE', #19623, 19.50000000000000000 ) ;
#13375 = DIRECTION ( 'NONE',  ( 0.000000000000000000, 0.000000000000000000, 1.000000000000000000 ) ) ;
#13376 = DIRECTION ( 'NONE',  ( -1.101824276508909887E-16, 1.000000000000000000, -0.000000000000000000 ) ) ;
#13377 = CIRCLE ( 'NONE', #20688, 1.042135311067126979 ) ;
#13378 = CARTESIAN_POINT ( 'NONE',  ( 78.34648107337082479, -4.961365878511911909, 79.93084625785569131 ) ) ;
#13379 = ORIENTED_EDGE ( 'NONE', *, *, #25567, .T. ) ;
#13380 = DIRECTION ( 'NONE',  ( -1.000000000000000000, 0.000000000000000000, 0.000000000000000000 ) ) ;
#13381 = CARTESIAN_POINT ( 'NONE',  ( 8.698509210239558698, 29.09164230456639899, 47.04930799450051637 ) ) ;
#13382 = DIRECTION ( 'NONE',  ( 0.9612616959383250004, 0.2756373558169784577, -1.660411357259259765E-16 ) ) ;
#13383 = ORIENTED_EDGE ( 'NONE', *, *, #31430, .T. ) ;
#13384 = CARTESIAN_POINT ( 'NONE',  ( -41.02687597405218156, 7.220473278338834788, 60.54930799450051637 ) ) ;
#13385 = FACE_OUTER_BOUND ( 'NONE', #21897, .T. ) ;
#13386 = CARTESIAN_POINT ( 'NONE',  ( 21.09992658989239089, 27.21183152705960495, 47.04930799450051637 ) ) ;
#13387 = CARTESIAN_POINT ( 'NONE',  ( 54.82593361024983381, -2.878806504921699094, -8.356670642478869482 ) ) ;
#13388 = ORIENTED_EDGE ( 'NONE', *, *, #4750, .T. ) ;
#13389 = LINE ( 'NONE', #413, #12549 ) ;
#13390 = ORIENTED_EDGE ( 'NONE', *, *, #15164, .T. ) ;
#13391 = EDGE_CURVE ( 'NONE', #32074, #5664, #8352, .T. ) ;
#13392 = VERTEX_POINT ( 'NONE', #3272 ) ;
#13393 = CIRCLE ( 'NONE', #6047, 0.09999999999999795164 ) ;
#13394 = TOROIDAL_SURFACE ( 'NONE', #21232, 12.40141737965282154, 0.1250000000000006939 ) ;
#13395 = CIRCLE ( 'NONE', #14441, 12.36707279061065101 ) ;
#13396 = AXIS2_PLACEMENT_3D ( 'NONE', #32091, #14210, #19267 ) ;
#13397 = AXIS2_PLACEMENT_3D ( 'NONE', #17128, #9270, #1879 ) ;
#13398 = EDGE_CURVE ( 'NONE', #17663, #26196, #20919, .T. ) ;
#13399 = CARTESIAN_POINT ( 'NONE',  ( -36.84960911689896079, -5.942107891656587704, 78.14337069435562455 ) ) ;
#13400 = CARTESIAN_POINT ( 'NONE',  ( -40.64704422177600662, 9.403915785377417791, 34.54930799450051637 ) ) ;
#13401 = ADVANCED_FACE ( 'NONE', ( #13305 ), #814, .F. ) ;
#13402 = VERTEX_POINT ( 'NONE', #23937 ) ;
#13403 = CARTESIAN_POINT ( 'NONE',  ( -35.09136543214532367, 10.88994114954489234, 41.81952777619033412 ) ) ;
#13404 = ORIENTED_EDGE ( 'NONE', *, *, #18724, .T. ) ;
#13405 = CARTESIAN_POINT ( 'NONE',  ( -5.602943079677954685, 9.702389020015065313, 106.8025418868326284 ) ) ;
#13406 = DIRECTION ( 'NONE',  ( -1.000000000000000000, 0.000000000000000000, 0.000000000000000000 ) ) ;
#13407 = CARTESIAN_POINT ( 'NONE',  ( -34.34753876910989590, -2.938577454171012349, 80.77644560816827379 ) ) ;
#13408 = DIRECTION ( 'NONE',  ( -1.000000000000000000, 0.000000000000000000, 0.000000000000000000 ) ) ;
#13409 = ORIENTED_EDGE ( 'NONE', *, *, #30737, .F. ) ;
#13410 = CYLINDRICAL_SURFACE ( 'NONE', #17026, 0.1000000000000018235 ) ;
#13411 = ORIENTED_EDGE ( 'NONE', *, *, #29160, .T. ) ;
#13412 = CARTESIAN_POINT ( 'NONE',  ( 33.72499318558949710, 32.34184655352418503, 47.04930799450051637 ) ) ;
#13413 = CARTESIAN_POINT ( 'NONE',  ( 45.84510715990803220, 22.84434098701873594, 45.30553951807763013 ) ) ;
#13414 = VERTEX_POINT ( 'NONE', #31335 ) ;
#13415 = CARTESIAN_POINT ( 'NONE',  ( -40.47970302497625994, 7.463434137431150361, 60.44930799450051495 ) ) ;
#13416 = CARTESIAN_POINT ( 'NONE',  ( -35.89491889087902621, 10.89025382816431531, 52.27940093726513737 ) ) ;
#13417 = CARTESIAN_POINT ( 'NONE',  ( -40.52064562223811350, 7.631811404637807605, 53.92244792118258090 ) ) ;
#13418 = DIRECTION ( 'NONE',  ( -1.101824276508909887E-16, 1.000000000000000000, -0.000000000000000000 ) ) ;
#13419 = CARTESIAN_POINT ( 'NONE',  ( 46.99023568444673060, 25.03791119454916014, 49.12151524109405898 ) ) ;
#13420 = ORIENTED_EDGE ( 'NONE', *, *, #11886, .F. ) ;
#13421 = DIRECTION ( 'NONE',  ( 0.000000000000000000, 0.000000000000000000, -1.000000000000000000 ) ) ;
#13422 = LINE ( 'NONE', #30813, #4910 ) ;
#13423 = ORIENTED_EDGE ( 'NONE', *, *, #26387, .F. ) ;
#13424 = DIRECTION ( 'NONE',  ( -1.000000000000000000, 0.000000000000000000, 0.000000000000000000 ) ) ;
#13425 = CIRCLE ( 'NONE', #7657, 71.29999999999996874 ) ;
#13426 = PRESENTATION_LAYER_ASSIGNMENT (  '', '', ( #6075 ) ) ;
#13427 = ADVANCED_FACE ( 'NONE', ( #29032 ), #12554, .T. ) ;
#13428 = DIRECTION ( 'NONE',  ( -1.000000000000000000, -1.101824276508909887E-16, 0.000000000000000000 ) ) ;
#13429 = ORIENTED_EDGE ( 'NONE', *, *, #19622, .T. ) ;
#13430 = ORIENTED_EDGE ( 'NONE', *, *, #8532, .F. ) ;
#13431 = CYLINDRICAL_SURFACE ( 'NONE', #13119, 12.36707279061065101 ) ;
#13432 = ADVANCED_FACE ( 'NONE', ( #11156 ), #17783, .T. ) ;
#13433 = UNCERTAINTY_MEASURE_WITH_UNIT (LENGTH_MEASURE( 1.000000000000000082E-05 ), #3258, 'distance_accuracy_value', 'NONE');
#13434 = EDGE_CURVE ( 'NONE', #3392, #21636, #21633, .T. ) ;
#13435 = CIRCLE ( 'NONE', #21794, 12.36707279061065279 ) ;
#13436 = EDGE_LOOP ( 'NONE', ( #11111, #14539, #11617, #17943 ) ) ;
#13437 = ORIENTED_EDGE ( 'NONE', *, *, #19817, .T. ) ;
#13438 = DIRECTION ( 'NONE',  ( -1.000000000000000000, 0.000000000000000000, 0.000000000000000000 ) ) ;
#13439 = EDGE_CURVE ( 'NONE', #8460, #9948, #19165, .T. ) ;
#13440 = CIRCLE ( 'NONE', #17616, 13.00178401536290806 ) ;
#13441 = VERTEX_POINT ( 'NONE', #31180 ) ;
#13442 = CARTESIAN_POINT ( 'NONE',  ( 47.50182977464208989, 23.10527865767145173, 47.47507095415797096 ) ) ;
#13443 = DIRECTION ( 'NONE',  ( 0.000000000000000000, 0.000000000000000000, 1.000000000000000000 ) ) ;
#13444 = CARTESIAN_POINT ( 'NONE',  ( 52.57325962015784171, -5.881344816830202049, 106.1937027734941523 ) ) ;
#13445 = CARTESIAN_POINT ( 'NONE',  ( 48.91284552371730143, 25.99289516297709923, 46.12344667017377020 ) ) ;
#13446 = ORIENTED_EDGE ( 'NONE', *, *, #7689, .T. ) ;
#13447 = ORIENTED_EDGE ( 'NONE', *, *, #24187, .T. ) ;
#13448 = FACE_OUTER_BOUND ( 'NONE', #8845, .T. ) ;
#13449 = EDGE_LOOP ( 'NONE', ( #17858, #12408, #31130, #18809 ) ) ;
#13450 = TOROIDAL_SURFACE ( 'NONE', #17081, 29.50000000000000355, 1.500000000000001332 ) ;
#13451 = CARTESIAN_POINT ( 'NONE',  ( 45.85675386737194259, 10.95084857405596068, 98.61391123392256475 ) ) ;
#13452 = CARTESIAN_POINT ( 'NONE',  ( 54.00540614691084329, -4.922489993312315626, 104.2573514652678739 ) ) ;
#13453 = DIRECTION ( 'NONE',  ( 1.234978253042719660E-16, -1.000000000000000000, -1.109335647967047851E-31 ) ) ;
#13454 = DIRECTION ( 'NONE',  ( -0.000000000000000000, -1.000000000000000000, 0.000000000000000000 ) ) ;
#13455 = DIRECTION ( 'NONE',  ( -0.4848096202463430537, -0.8746197071393926326, -9.920727850371701658E-18 ) ) ;
#13456 = ADVANCED_FACE ( 'NONE', ( #5909 ), #3594, .T. ) ;
#13457 = ORIENTED_EDGE ( 'NONE', *, *, #11602, .F. ) ;
#13458 = FACE_OUTER_BOUND ( 'NONE', #13113, .T. ) ;
#13459 = CARTESIAN_POINT ( 'NONE',  ( 52.07598125554711999, -5.935454207752202116, 105.0538709090500333 ) ) ;
#13460 = FACE_OUTER_BOUND ( 'NONE', #14188, .T. ) ;
#13461 = EDGE_CURVE ( 'NONE', #28053, #16797, #25647, .T. ) ;
#13462 = CARTESIAN_POINT ( 'NONE',  ( 48.83059991212272166, 25.45948167178348953, 48.97189174113093912 ) ) ;
#13463 = CARTESIAN_POINT ( 'NONE',  ( 21.09992658989238734, 38.56284415653841791, 47.04930799450051637 ) ) ;
#13464 = EDGE_LOOP ( 'NONE', ( #4369, #24723, #4881, #19868 ) ) ;
#13465 = CARTESIAN_POINT ( 'NONE',  ( -42.22138300640814634, 14.68176690255379491, 35.90717268343339441 ) ) ;
#13466 = CARTESIAN_POINT ( 'NONE',  ( -40.57832940339287831, 7.446916344587784842, 53.80788663826320573 ) ) ;
#13467 = ADVANCED_FACE ( 'NONE', ( #11466 ), #25917, .T. ) ;
#13468 = AXIS2_PLACEMENT_3D ( 'NONE', #12973, #18515, #22960 ) ;
#13469 = EDGE_CURVE ( 'NONE', #17250, #20645, #17241, .T. ) ;
#13470 = EDGE_CURVE ( 'NONE', #7990, #2384, #31919, .T. ) ;
#13471 = ORIENTED_EDGE ( 'NONE', *, *, #29543, .T. ) ;
#13472 = CIRCLE ( 'NONE', #15547, 12.36707279061065279 ) ;
#13473 = EDGE_LOOP ( 'NONE', ( #8795, #14830 ) ) ;
#13474 = DIRECTION ( 'NONE',  ( 1.000000000000000000, 0.000000000000000000, 0.000000000000000000 ) ) ;
#13475 = CARTESIAN_POINT ( 'NONE',  ( 8.732853799281732776, 31.96183152705962272, 47.04930799450051637 ) ) ;
#13476 = CARTESIAN_POINT ( 'NONE',  ( 21.09785597605719332, 15.24673779880127178, 34.56516646732339382 ) ) ;
#13477 = ORIENTED_EDGE ( 'NONE', *, *, #16806, .T. ) ;
#13478 = CARTESIAN_POINT ( 'NONE',  ( -40.23672901771082877, 7.760455916344220384, 34.54930799450052348 ) ) ;
#13479 = DIRECTION ( 'NONE',  ( -1.000000000000000000, 0.000000000000000000, 0.000000000000000000 ) ) ;
#13480 = CARTESIAN_POINT ( 'NONE',  ( -40.09211399732166115, 9.667069410243959382, 39.44930799450052206 ) ) ;
#13481 = ORIENTED_EDGE ( 'NONE', *, *, #178, .T. ) ;
#13482 = CYLINDRICAL_SURFACE ( 'NONE', #24493, 0.09999999999999945044 ) ;
#13483 = ORIENTED_EDGE ( 'NONE', *, *, #6806, .T. ) ;
#13484 = DIRECTION ( 'NONE',  ( 0.4848096202463424431, 0.8746197071393927436, -2.220446049250312588E-16 ) ) ;
#13485 = LINE ( 'NONE', #23486, #11792 ) ;
#13486 = CARTESIAN_POINT ( 'NONE',  ( 47.41252533345003428, 29.19474943853624183, 44.59074167925342635 ) ) ;
#13487 = DIRECTION ( 'NONE',  ( -1.101824276508909887E-16, 1.000000000000000000, -0.000000000000000000 ) ) ;
#13488 = DIRECTION ( 'NONE',  ( 1.000000000000000000, 0.000000000000000000, 0.000000000000000000 ) ) ;
#13489 = ADVANCED_FACE ( 'NONE', ( #23773, #1285 ), #23622, .T. ) ;
#13490 = VERTEX_POINT ( 'NONE', #3431 ) ;
#13491 = ORIENTED_EDGE ( 'NONE', *, *, #32480, .F. ) ;
#13492 = DIRECTION ( 'NONE',  ( 0.2756373558169954441, -0.9612616959383198934, 1.479773560108263204E-16 ) ) ;
#13493 = DIRECTION ( 'NONE',  ( -1.101824276508909887E-16, 1.000000000000000000, -0.000000000000000000 ) ) ;
#13494 = EDGE_CURVE ( 'NONE', #11279, #24034, #17208, .T. ) ;
#13495 = DIRECTION ( 'NONE',  ( -1.101824276508909887E-16, 1.000000000000000000, -0.000000000000000000 ) ) ;
#13496 = VERTEX_POINT ( 'NONE', #26074 ) ;
#13497 =( BOUNDED_CURVE ( )  B_SPLINE_CURVE ( 3, ( #6533, #11942, #21936, #29673 ),
 .UNSPECIFIED., .F., .F. ) 
 B_SPLINE_CURVE_WITH_KNOTS ( ( 4, 4 ),
 ( 1.558993681807626333E-14, 1.570796326794877240 ),
 .UNSPECIFIED. ) 
 CURVE ( )  GEOMETRIC_REPRESENTATION_ITEM ( )  RATIONAL_B_SPLINE_CURVE ( ( 1.000000000000000000, 0.8047378541243732641, 0.8047378541243732641, 1.000000000000000000 ) ) 
 REPRESENTATION_ITEM ( '' )  );
#13498 = DIRECTION ( 'NONE',  ( -0.000000000000000000, -1.000000000000000000, 0.000000000000000000 ) ) ;
#13499 = DIRECTION ( 'NONE',  ( -1.101824276508909887E-16, 1.000000000000000000, -0.000000000000000000 ) ) ;
#13500 = ORIENTED_EDGE ( 'NONE', *, *, #5988, .F. ) ;
#13501 = FACE_OUTER_BOUND ( 'NONE', #9494, .T. ) ;
#13502 = CARTESIAN_POINT ( 'NONE',  ( 45.73035263060504718, 27.23954579807170262, 44.36855633853329550 ) ) ;
#13503 = EDGE_CURVE ( 'NONE', #8733, #8315, #6777, .T. ) ;
#13504 = CARTESIAN_POINT ( 'NONE',  ( -39.41060154113746705, -5.935741391424327773, 77.97157130629763344 ) ) ;
#13505 = CIRCLE ( 'NONE', #17682, 0.1999999999999987899 ) ;
#13506 = VECTOR ( 'NONE', #6434, 1000.000000000000000 ) ;
#13507 = AXIS2_PLACEMENT_3D ( 'NONE', #21988, #21334, #26440 ) ;
#13508 = ORIENTED_EDGE ( 'NONE', *, *, #1216, .T. ) ;
#13509 = VECTOR ( 'NONE', #24327, 1000.000000000000000 ) ;
#13510 = DIRECTION ( 'NONE',  ( -1.101824276508909887E-16, 1.000000000000000000, -0.000000000000000000 ) ) ;
#13511 = DIRECTION ( 'NONE',  ( 0.000000000000000000, -1.000000000000000000, 0.000000000000000000 ) ) ;
#13512 = AXIS2_PLACEMENT_3D ( 'NONE', #13714, #25853, #11097 ) ;
#13513 = ORIENTED_EDGE ( 'NONE', *, *, #21783, .F. ) ;
#13514 = CARTESIAN_POINT ( 'NONE',  ( -6.902144023942794249, 14.86454579224779948, 47.04930799450052348 ) ) ;
#13515 = CARTESIAN_POINT ( 'NONE',  ( -40.18454328187963398, 7.548069831825863218, 53.64930799450051779 ) ) ;
#13516 = CARTESIAN_POINT ( 'NONE',  ( 71.55763488011925233, 9.127627432390726270, 19.66944483935173338 ) ) ;
#13517 = VERTEX_POINT ( 'NONE', #1614 ) ;
#13518 = CARTESIAN_POINT ( 'NONE',  ( 21.09785597605719332, -13.74048473023143835, -11.17459240385188934 ) ) ;
#13519 = CARTESIAN_POINT ( 'NONE',  ( -42.73182147790732444, -0.8057266458565844891, 32.14930799450051779 ) ) ;
#13520 = FACE_OUTER_BOUND ( 'NONE', #17395, .T. ) ;
#13521 = CARTESIAN_POINT ( 'NONE',  ( 44.21498992391908445, 25.31753733014356555, 46.89958605635242606 ) ) ;
#13522 = ORIENTED_EDGE ( 'NONE', *, *, #19977, .F. ) ;
#13523 = CARTESIAN_POINT ( 'NONE',  ( 47.16432553341419975, 22.86454579224779948, 45.05006465737218235 ) ) ;
#13525 = CARTESIAN_POINT ( 'NONE',  ( 48.94625023931840246, 29.47124452788248306, 46.10640627770150246 ) ) ;
#13524 = AXIS2_PLACEMENT_3D ( 'NONE', #6423, #1485, #9045 ) ;
#13526 = AXIS2_PLACEMENT_3D ( 'NONE', #24727, #4869, #25050 ) ;
#13527 = LINE ( 'NONE', #21534, #8805 ) ;
#13528 = DIRECTION ( 'NONE',  ( -2.779292025043186357E-18, 1.288349127009862211E-17, -1.000000000000000000 ) ) ;
#13529 = VERTEX_POINT ( 'NONE', #11637 ) ;
#13530 = CARTESIAN_POINT ( 'NONE',  ( 8.823575513742490273, 15.24673779880127356, 47.37072134000479906 ) ) ;
#13531 = FACE_OUTER_BOUND ( 'NONE', #22045, .T. ) ;
#13532 = DIRECTION ( 'NONE',  ( -1.000000000000000000, -1.101824276508909764E-16, 0.000000000000000000 ) ) ;
#13533 = AXIS2_PLACEMENT_3D ( 'NONE', #10150, #17025, #19494 ) ;
#13534 = ORIENTED_EDGE ( 'NONE', *, *, #29693, .F. ) ;
#13535 = CARTESIAN_POINT ( 'NONE',  ( -40.44437521412185532, 7.396217677353669195, 39.44930799450052206 ) ) ;
#13536 = FACE_OUTER_BOUND ( 'NONE', #27917, .T. ) ;
#13537 = EDGE_CURVE ( 'NONE', #14722, #6401, #8527, .T. ) ;
#13538 = AXIS2_PLACEMENT_3D ( 'NONE', #191, #27762, #24648 ) ;
#13539 = EDGE_LOOP ( 'NONE', ( #4278, #19199, #9358, #25322 ) ) ;
#13540 = ADVANCED_FACE ( 'NONE', ( #21796 ), #19504, .F. ) ;
#13541 = CARTESIAN_POINT ( 'NONE',  ( 73.03377152639730241, 11.55930814891847191, 23.89416354099248707 ) ) ;
#13542 = VERTEX_POINT ( 'NONE', #14428 ) ;
#13543 = VERTEX_POINT ( 'NONE', #7194 ) ;
#13544 = TOROIDAL_SURFACE ( 'NONE', #12502, 12.40141737965283397, 0.1249999999999992922 ) ;
#13545 = TOROIDAL_SURFACE ( 'NONE', #15115, 0.8928932188134564019, 0.1000000000000000056 ) ;
#13546 = TOROIDAL_SURFACE ( 'NONE', #11451, 12.40141737965285174, 0.1249999999999993200 ) ;
#13547 = CIRCLE ( 'NONE', #24006, 67.18681090792816235 ) ;
#13548 = AXIS2_PLACEMENT_3D ( 'NONE', #2911, #28359, #23098 ) ;
#13549 = FACE_OUTER_BOUND ( 'NONE', #6575, .T. ) ;
#13550 = CARTESIAN_POINT ( 'NONE',  ( -40.60249826926477823, 9.398840415180675478, 34.59072935073783128 ) ) ;
#13551 = ORIENTED_EDGE ( 'NONE', *, *, #12257, .T. ) ;
#13552 = AXIS2_PLACEMENT_3D ( 'NONE', #8402, #520, #8245 ) ;
#13553 = CARTESIAN_POINT ( 'NONE',  ( -35.51007442658541180, 10.17492932633761171, 42.04930799450051637 ) ) ;
#13554 = ORIENTED_EDGE ( 'NONE', *, *, #429, .F. ) ;
#13555 = CARTESIAN_POINT ( 'NONE',  ( 21.09785597605719687, 30.56454579224779522, 30.04930799450051282 ) ) ;
#13556 = LINE ( 'NONE', #22013, #9135 ) ;
#13557 = DIRECTION ( 'NONE',  ( 0.000000000000000000, 0.000000000000000000, -1.000000000000000000 ) ) ;
#13558 = CARTESIAN_POINT ( 'NONE',  ( 55.09785597605721108, -5.098646251524523443, 47.04930799450051637 ) ) ;
#13559 = ADVANCED_FACE ( 'NONE', ( #1782 ), #26727, .F. ) ;
#13560 = VERTEX_POINT ( 'NONE', #31816 ) ;
#13561 = CARTESIAN_POINT ( 'NONE',  ( 21.09992658989239089, 24.84143805560860940, 47.04930799450051637 ) ) ;
#13562 = VERTEX_POINT ( 'NONE', #25366 ) ;
#13563 = DIRECTION ( 'NONE',  ( -1.224646799147353207E-16, -1.349345573449484691E-32, 1.000000000000000000 ) ) ;
#13564 = CARTESIAN_POINT ( 'NONE',  ( 33.72499318558949000, 38.56284415653841791, 47.04930799450051637 ) ) ;
#13565 = EDGE_LOOP ( 'NONE', ( #11445, #22323, #11840, #20505 ) ) ;
#13566 = CYLINDRICAL_SURFACE ( 'NONE', #2743, 12.62506659569710266 ) ;
#13567 = DIRECTION ( 'NONE',  ( 0.2756373558170082672, -0.9612616959383162296, 0.000000000000000000 ) ) ;
#13568 = DIRECTION ( 'NONE',  ( -1.102049569453931065E-16, 0.000000000000000000, 1.000000000000000000 ) ) ;
#13569 = CARTESIAN_POINT ( 'NONE',  ( -41.04685960816998147, 9.497330455345890599, 35.54930799450052348 ) ) ;
#13570 = CARTESIAN_POINT ( 'NONE',  ( 33.46699938050304013, 29.71183152705961561, 47.04930799450051637 ) ) ;
#13571 = ORIENTED_EDGE ( 'NONE', *, *, #24563, .T. ) ;
#13572 = DIRECTION ( 'NONE',  ( -1.101824276508909887E-16, 1.000000000000000000, -0.000000000000000000 ) ) ;
#13573 = DIRECTION ( 'NONE',  ( 0.2756373558169932236, -0.9612616959383205595, 1.479773560108267395E-16 ) ) ;
#13574 = ORIENTED_EDGE ( 'NONE', *, *, #21653, .T. ) ;
#13575 = CARTESIAN_POINT ( 'NONE',  ( -41.24971778908466291, 11.62557032131817181, 56.04611646155296256 ) ) ;
#13576 = CIRCLE ( 'NONE', #30346, 0.1000000000000007272 ) ;
#13577 = AXIS2_PLACEMENT_3D ( 'NONE', #5511, #2876, #30296 ) ;
#13578 = CARTESIAN_POINT ( 'NONE',  ( -9.925114359954182675, -5.937449718911893548, -13.57859485750651629 ) ) ;
#13579 = VECTOR ( 'NONE', #18042, 1000.000000000000000 ) ;
#13580 = EDGE_CURVE ( 'NONE', #22946, #9753, #15170, .T. ) ;
#13581 = EDGE_CURVE ( 'NONE', #28526, #30980, #21950, .T. ) ;
#13582 = VERTEX_POINT ( 'NONE', #29354 ) ;
#13583 = EDGE_CURVE ( 'NONE', #31727, #1328, #21948, .T. ) ;
#13584 = VERTEX_POINT ( 'NONE', #32313 ) ;
#13585 = CARTESIAN_POINT ( 'NONE',  ( -7.928239498742526870, 7.324825086315946976, 98.65516431386642182 ) ) ;
#13586 = ADVANCED_FACE ( 'NONE', ( #19497 ), #30359, .T. ) ;
#13587 = TOROIDAL_SURFACE ( 'NONE', #3592, 12.61792373059891403, 0.1250000000000023315 ) ;
#13588 = EDGE_LOOP ( 'NONE', ( #208, #17754, #4586, #8304 ) ) ;
#13589 = VERTEX_POINT ( 'NONE', #9328 ) ;
#13590 = CARTESIAN_POINT ( 'NONE',  ( 71.49893360114316465, 5.388785998227650254, 16.47908017486093257 ) ) ;
#13591 = AXIS2_PLACEMENT_3D ( 'NONE', #10293, #24731, #5369 ) ;
#13592 = ORIENTED_EDGE ( 'NONE', *, *, #15628, .T. ) ;
#13593 = CARTESIAN_POINT ( 'NONE',  ( 47.22573328838134188, 23.12036939723557083, 47.29998918090146987 ) ) ;
#13594 = CARTESIAN_POINT ( 'NONE',  ( 46.99747725352182925, 22.88065857334294861, 48.98207832244369087 ) ) ;
#13595 = CARTESIAN_POINT ( 'NONE',  ( 52.89687679232817175, -5.771419034597327524, 105.5847057727601026 ) ) ;
#13596 = CARTESIAN_POINT ( 'NONE',  ( 48.80717017713595141, 25.17622849631044346, 48.15820438821415195 ) ) ;
#13597 = EDGE_CURVE ( 'NONE', #3694, #17205, #2042, .T. ) ;
#13598 = ORIENTED_EDGE ( 'NONE', *, *, #25292, .T. ) ;
#13599 = VERTEX_POINT ( 'NONE', #9823 ) ;
#13600 = CARTESIAN_POINT ( 'NONE',  ( -43.64647580959332629, 1.256990871545142774, 60.54930799450051637 ) ) ;
#13601 = EDGE_CURVE ( 'NONE', #1187, #18622, #7030, .T. ) ;
#13602 = ORIENTED_EDGE ( 'NONE', *, *, #19433, .T. ) ;
#13603 = TOROIDAL_SURFACE ( 'NONE', #18292, 12.61792373059893535, 0.1249999999999994033 ) ;
#13604 = CARTESIAN_POINT ( 'NONE',  ( 21.09992658989239089, 24.97145308207319303, 47.04930799450051637 ) ) ;
#13605 = CARTESIAN_POINT ( 'NONE',  ( 8.732853799281732776, 38.56284415653841791, 47.04930799450051637 ) ) ;
#13606 = DIRECTION ( 'NONE',  ( 0.1949050434465282866, -0.6797146636928672603, 0.7071067811865469066 ) ) ;
#13607 = AXIS2_PLACEMENT_3D ( 'NONE', #32317, #27552, #7369 ) ;
#13608 = DIRECTION ( 'NONE',  ( -1.000000000000000000, 0.000000000000000000, 0.000000000000000000 ) ) ;
#13609 = DIRECTION ( 'NONE',  ( -0.8746197071393823075, 0.4848096202463614279, 0.000000000000000000 ) ) ;
#13610 = CONTEXT_DEPENDENT_SHAPE_REPRESENTATION ( #21434, #16625 ) ;
#13611 = EDGE_LOOP ( 'NONE', ( #8948, #18840, #26827, #22219 ) ) ;
#13612 = CARTESIAN_POINT ( 'NONE',  ( 21.09785597605720753, 13.86454579224779948, 47.04930799450052348 ) ) ;
#13613 = CARTESIAN_POINT ( 'NONE',  ( -30.63875195204110469, 3.314680658590930751, 15.43500191121110809 ) ) ;
#13614 = DIRECTION ( 'NONE',  ( -1.101824276508909887E-16, 1.000000000000000000, -0.000000000000000000 ) ) ;
#13615 = DIRECTION ( 'NONE',  ( -1.000000000000000000, -1.101824276508910010E-16, 0.000000000000000000 ) ) ;
#13616 = CARTESIAN_POINT ( 'NONE',  ( 21.09992658989239089, 28.22145308207318237, 47.04930799450051637 ) ) ;
#13617 = DIRECTION ( 'NONE',  ( -1.000000000000000000, 0.000000000000000000, 2.775557561562888984E-15 ) ) ;
#13618 = EDGE_LOOP ( 'NONE', ( #18704, #19680, #28649, #21761 ) ) ;
#13619 = CARTESIAN_POINT ( 'NONE',  ( 21.09785597605719332, -5.721341737285094098, 47.04930799450051637 ) ) ;
#13620 = LINE ( 'NONE', #1136, #5158 ) ;
#13621 = EDGE_CURVE ( 'NONE', #3661, #13254, #14634, .T. ) ;
#13622 = AXIS2_PLACEMENT_3D ( 'NONE', #8113, #20895, #20737 ) ;
#13623 = AXIS2_PLACEMENT_3D ( 'NONE', #7285, #22206, #17112 ) ;
#13624 = EDGE_LOOP ( 'NONE', ( #28344, #5501, #28453, #16509 ) ) ;
#13625 = CIRCLE ( 'NONE', #17812, 84.30000000000001137 ) ;
#13626 = AXIS2_PLACEMENT_3D ( 'NONE', #5128, #30402, #27770 ) ;
#13627 = ORIENTED_EDGE ( 'NONE', *, *, #1926, .F. ) ;
#13628 = EDGE_CURVE ( 'NONE', #15153, #22400, #3112, .T. ) ;
#13629 = DIRECTION ( 'NONE',  ( 0.1949050434465268156, -0.6797146636928667052, 0.7071067811865480168 ) ) ;
#13630 = CIRCLE ( 'NONE', #2100, 12.36707279061065279 ) ;
#13631 = DIRECTION ( 'NONE',  ( -1.101824276508909887E-16, 1.000000000000000000, -0.000000000000000000 ) ) ;
#13632 = DIRECTION ( 'NONE',  ( -1.101824276508909887E-16, 1.000000000000000000, -0.000000000000000000 ) ) ;
#13633 = EDGE_CURVE ( 'NONE', #13336, #30065, #27223, .T. ) ;
#13634 = ORIENTED_EDGE ( 'NONE', *, *, #18846, .F. ) ;
#13635 = CARTESIAN_POINT ( 'NONE',  ( -27.33830150920368496, -13.30632128221581212, 75.01995691340935934 ) ) ;
#13636 = CARTESIAN_POINT ( 'NONE',  ( 33.50134396954518223, 32.34164230456639899, 47.04930799450051637 ) ) ;
#13637 = CARTESIAN_POINT ( 'NONE',  ( 8.482002859293778840, 29.96664230456641675, 47.04930799450051637 ) ) ;
#13638 = EDGE_CURVE ( 'NONE', #2431, #13895, #3676, .T. ) ;
#13639 = VERTEX_POINT ( 'NONE', #5989 ) ;
#13640 = DIRECTION ( 'NONE',  ( 0.4848096202463489934, 0.8746197071393893019, 9.920727850371641569E-18 ) ) ;
#13641 = VECTOR ( 'NONE', #26624, 999.9999999999998863 ) ;
#13642 = EDGE_CURVE ( 'NONE', #26091, #22946, #1206, .T. ) ;
#13643 = ORIENTED_EDGE ( 'NONE', *, *, #2449, .F. ) ;
#13644 = DIRECTION ( 'NONE',  ( -0.000000000000000000, -1.000000000000000000, -0.000000000000000000 ) ) ;
#13645 = EDGE_CURVE ( 'NONE', #9452, #12114, #3509, .T. ) ;
#13646 = CARTESIAN_POINT ( 'NONE',  ( -42.03703168893574116, 3.954238390689462257, 45.14930799450051779 ) ) ;
#13647 = CARTESIAN_POINT ( 'NONE',  ( 46.78253665710180087, 29.21161237798985866, 44.60769444413243434 ) ) ;
#13648 = DIRECTION ( 'NONE',  ( 0.2756373558169954441, -0.9612616959383198934, -1.163221239882716147E-31 ) ) ;
#13649 = PRESENTATION_STYLE_ASSIGNMENT (( #5938 ) ) ;
#13650 = EDGE_LOOP ( 'NONE', ( #5557, #23552, #23561, #24044 ) ) ;
#13651 = VERTEX_POINT ( 'NONE', #18601 ) ;
#13652 = DIRECTION ( 'NONE',  ( -0.9996573249755574819, -1.344306794811909066E-16, -0.02617694830786587365 ) ) ;
#13653 = CARTESIAN_POINT ( 'NONE',  ( 106.0978559760576161, -5.935454207751966749, 16.07118271501087747 ) ) ;
#13654 = VECTOR ( 'NONE', #16401, 1000.000000000000000 ) ;
#13655 = DIRECTION ( 'NONE',  ( 0.000000000000000000, 0.000000000000000000, -1.000000000000000000 ) ) ;
#13656 = EDGE_LOOP ( 'NONE', ( #17193, #17623, #4096, #18341, #9831 ) ) ;
#13657 = CARTESIAN_POINT ( 'NONE',  ( 21.09992658989238734, 31.96664230456639544, 47.04930799450051637 ) ) ;
#13658 = AXIS2_PLACEMENT_3D ( 'NONE', #24126, #9529, #4436 ) ;
#13659 = CARTESIAN_POINT ( 'NONE',  ( 33.46699938050303302, 38.56284415653841791, 47.04930799450051637 ) ) ;
#13660 = ORIENTED_EDGE ( 'NONE', *, *, #3846, .T. ) ;
#13661 = CARTESIAN_POINT ( 'NONE',  ( 21.09785597605719332, 7.094379510609982731, 47.04930799450051637 ) ) ;
#13662 = CIRCLE ( 'NONE', #16772, 0.1250000000000001110 ) ;
#13663 = CARTESIAN_POINT ( 'NONE',  ( 44.77625694075214824, 27.41454579807170688, 48.23360063142255427 ) ) ;
#13664 = ADVANCED_FACE ( 'NONE', ( #27989 ), #20428, .T. ) ;
#13665 = AXIS2_PLACEMENT_3D ( 'NONE', #28117, #2987, #3144 ) ;
#13666 = CARTESIAN_POINT ( 'NONE',  ( -39.40038788600242015, -5.936129073955724422, 77.93577773595035296 ) ) ;
#13667 = CIRCLE ( 'NONE', #16790, 0.9031915329475502796 ) ;
#13668 = ORIENTED_EDGE ( 'NONE', *, *, #14034, .F. ) ;
#13669 = EDGE_CURVE ( 'NONE', #7056, #16020, #23741, .T. ) ;
#13670 = DIRECTION ( 'NONE',  ( -1.000000000000000000, 0.000000000000000000, 0.000000000000000000 ) ) ;
#13671 = CARTESIAN_POINT ( 'NONE',  ( -40.21210701746133509, 7.644196001419694575, 53.80788663826320573 ) ) ;
#13672 = DIRECTION ( 'NONE',  ( 1.775451498209539969E-15, 0.000000000000000000, -1.000000000000000000 ) ) ;
#13673 = AXIS2_PLACEMENT_3D ( 'NONE', #22231, #29301, #17477 ) ;
#13674 = EDGE_CURVE ( 'NONE', #26992, #12577, #28801, .T. ) ;
#13675 = VERTEX_POINT ( 'NONE', #8286 ) ;
#13676 = CIRCLE ( 'NONE', #26782, 37.00000000000000711 ) ;
#13677 = DIRECTION ( 'NONE',  ( -0.4848096202463636484, -0.8746197071393810862, 0.000000000000000000 ) ) ;
#13678 = AXIS2_PLACEMENT_3D ( 'NONE', #15860, #5526, #5686 ) ;
#13679 = CARTESIAN_POINT ( 'NONE',  ( -58.11219453028166981, -16.63545420775219696, 49.54930799450023926 ) ) ;
#13680 = CIRCLE ( 'NONE', #32025, 12.62506659569710266 ) ;
#13681 = ADVANCED_FACE ( 'NONE', ( #13536 ), #25523, .F. ) ;
#13682 = ORIENTED_EDGE ( 'NONE', *, *, #17938, .T. ) ;
#13683 = CARTESIAN_POINT ( 'NONE',  ( 54.59785597605721108, 14.86454579224779948, 47.04930799450051637 ) ) ;
#13684 = LINE ( 'NONE', #31080, #29898 ) ;
#13685 = FACE_OUTER_BOUND ( 'NONE', #29558, .T. ) ;
#13686 =( BOUNDED_CURVE ( )  B_SPLINE_CURVE ( 2, ( #9701, #7236, #2793, #4937, #22811, #12329, #12663, #27583, #15271, #22324, #24791, #17231, #17401, #15109, #2634, #27743, #15427, #10346, #27246, #32350, #12495, #25119, #22650, #27908, #9861, #10190, #17721, #19860, #20187, #29890, #5261, #25286, #12821, #27421, #325, #20341, #30370, #7889, #32189, #5426, #14953, #25440, #24959, #12164, #22160, #2473, #28704, #6224, #10995, #30856, #18198, #30538, #972, #22964, #815, #3273, #28070, #1131, #5582, #15580, #28230, #31018, #15912, #16066, #8363, #484, #25918, #3099, #28391, #8209, #28556, #23461, #10840, #20673, #11158, #30700, #18681, #654, #20990 ),
 .UNSPECIFIED., .F., .F. ) 
 B_SPLINE_CURVE_WITH_KNOTS ( ( 3, 2, 2, 2, 2, 2, 2, 2, 2, 2, 2, 2, 2, 2, 2, 2, 2, 2, 2, 2, 2, 2, 2, 2, 2, 2, 2, 2, 2, 2, 2, 2, 2, 2, 2, 2, 2, 2, 2, 3 ),
 ( 0.06466318693218657543, 0.07142857142857142461, 0.09523809523809523281, 0.1190476190476190410, 0.1428571428571428492, 0.1666666666666666574, 0.1904761904761904656, 0.2142857142857143016, 0.2380952380952380820, 0.2619047619047619180, 0.2857142857142856984, 0.3095238095238095344, 0.3333333333333333148, 0.3571428571428571508, 0.3809523809523809312, 0.4047619047619047672, 0.4285714285714285476, 0.4523809523809523836, 0.4761904761904761640, 0.5000000000000000000, 0.5238095238095238360, 0.5476190476190476719, 0.5714285714285713969, 0.5952380952380952328, 0.6190476190476190688, 0.6428571428571429047, 0.6666666666666666297, 0.6904761904761904656, 0.7142857142857143016, 0.7380952380952381375, 0.7619047619047618625, 0.7857142857142856984, 0.8095238095238095344, 0.8333333333333333703, 0.8571428571428570953, 0.8809523809523809312, 0.9047619047619047672, 0.9285714285714287142, 0.9523809523809523281, 0.9642857142857166330 ),
 .UNSPECIFIED. ) 
 CURVE ( )  GEOMETRIC_REPRESENTATION_ITEM ( )  RATIONAL_B_SPLINE_CURVE ( ( 0.9454972278162998567, 0.9619316344418604725, 1.000000000000000000, 0.8660254037844387076, 1.000000000000000000, 0.8660254037844387076, 1.000000000000000000, 0.8660254037844387076, 1.000000000000000000, 0.8660254037844387076, 1.000000000000000000, 0.8660254037844387076, 1.000000000000000000, 0.8660254037844387076, 1.000000000000000000, 0.8660254037844387076, 1.000000000000000000, 0.8660254037844387076, 1.000000000000000000, 0.8660254037844387076, 1.000000000000000000, 0.8660254037844387076, 1.000000000000000000, 0.8660254037844387076, 1.000000000000000000, 0.8660254037844387076, 1.000000000000000000, 0.8660254037844387076, 1.000000000000000000, 0.8660254037844387076, 1.000000000000000000, 0.8660254037844387076, 1.000000000000000000, 0.8660254037844387076, 1.000000000000000000, 0.8660254037844387076, 1.000000000000000000, 0.8660254037844387076, 1.000000000000000000, 0.8660254037844387076, 1.000000000000000000, 0.8660254037844387076, 1.000000000000000000, 0.8660254037844387076, 1.000000000000000000, 0.8660254037844387076, 1.000000000000000000, 0.8660254037844387076, 1.000000000000000000, 0.8660254037844387076, 1.000000000000000000, 0.8660254037844387076, 1.000000000000000000, 0.8660254037844387076, 1.000000000000000000, 0.8660254037844387076, 1.000000000000000000, 0.8660254037844387076, 1.000000000000000000, 0.8660254037844387076, 1.000000000000000000, 0.8660254037844387076, 1.000000000000000000, 0.8660254037844387076, 1.000000000000000000, 0.8660254037844387076, 1.000000000000000000, 0.8660254037844387076, 1.000000000000000000, 0.8660254037844387076, 1.000000000000000000, 0.8660254037844387076, 1.000000000000000000, 0.8660254037844387076, 1.000000000000000000, 0.8660254037844387076, 1.000000000000000000, 0.9330127018922058646, 0.9330127018922192983 ) ) 
 REPRESENTATION_ITEM ( '' )  );
#13687 = LINE ( 'NONE', #21202, #19466 ) ;
#13688 = ORIENTED_EDGE ( 'NONE', *, *, #298, .F. ) ;
#13689 = DIRECTION ( 'NONE',  ( -1.101824276508909887E-16, 1.000000000000000000, -0.000000000000000000 ) ) ;
#13690 = CARTESIAN_POINT ( 'NONE',  ( 48.18662509608405742, 27.89624452788248377, 49.18364984542562013 ) ) ;
#13691 = AXIS2_PLACEMENT_3D ( 'NONE', #32136, #29177, #4719 ) ;
#13692 = CARTESIAN_POINT ( 'NONE',  ( 21.09785597605719332, 25.56454579224779877, 35.24930799450054053 ) ) ;
#13693 = DIRECTION ( 'NONE',  ( 1.000000000000000000, 0.000000000000000000, 0.000000000000000000 ) ) ;
#13694 = DIRECTION ( 'NONE',  ( -1.000000000000000000, -0.000000000000000000, -3.491481338843133355E-15 ) ) ;
#13695 = ORIENTED_EDGE ( 'NONE', *, *, #21668, .F. ) ;
#13696 = DIRECTION ( 'NONE',  ( -0.000000000000000000, -1.000000000000000000, 0.000000000000000000 ) ) ;
#13697 = CARTESIAN_POINT ( 'NONE',  ( 46.45846941443645761, 22.99884124225578930, 45.79590206249746132 ) ) ;
#13698 = DIRECTION ( 'NONE',  ( -1.000000000000000000, 0.000000000000000000, 0.000000000000000000 ) ) ;
#13699 = ORIENTED_EDGE ( 'NONE', *, *, #20082, .F. ) ;
#13700 = FACE_OUTER_BOUND ( 'NONE', #3143, .T. ) ;
#13701 = DIRECTION ( 'NONE',  ( -1.224646799147353207E-16, -1.349345573449484691E-32, 1.000000000000000000 ) ) ;
#13702 = CARTESIAN_POINT ( 'NONE',  ( 21.09785597605720753, 13.86454579224779948, 47.04930799450052348 ) ) ;
#13703 = CARTESIAN_POINT ( 'NONE',  ( 50.12395145085690729, 7.324825086315956746, -4.556548324865391741 ) ) ;
#13704 = ORIENTED_EDGE ( 'NONE', *, *, #31181, .T. ) ;
#13705 = FACE_OUTER_BOUND ( 'NONE', #29891, .T. ) ;
#13706 = CIRCLE ( 'NONE', #8455, 22.64135752993680484 ) ;
#13707 = EDGE_LOOP ( 'NONE', ( #19287, #5308, #8872, #18027 ) ) ;
#13708 = CIRCLE ( 'NONE', #14758, 15.23374605753642186 ) ;
#13709 = CIRCLE ( 'NONE', #17895, 12.27641737965284641 ) ;
#13710 = ORIENTED_EDGE ( 'NONE', *, *, #24694, .F. ) ;
#13711 = B_SPLINE_CURVE_WITH_KNOTS ( 'NONE', 3,
 ( #9553, #14807, #29410, #2324, #32363, #12343, #9873, #22493, #31869, #4951 ),
 .UNSPECIFIED., .F., .F.,
 ( 4, 2, 2, 2, 4 ),
 ( 0.0006716755660531790973, 0.002413276598758981421, 0.004154877631464783637, 0.005896478664170586720, 0.007638079696876388935 ),
 .UNSPECIFIED. ) ;
#13712 = AXIS2_PLACEMENT_3D ( 'NONE', #27931, #2494, #22506 ) ;
#13713 = DIRECTION ( 'NONE',  ( 0.000000000000000000, 1.000000000000000000, -0.000000000000000000 ) ) ;
#13714 = CARTESIAN_POINT ( 'NONE',  ( 21.09992658989238734, 32.34164230456639899, 47.04930799450051637 ) ) ;
#13715 = CARTESIAN_POINT ( 'NONE',  ( 81.76548788166886084, -5.935709855254037493, 77.87985502756478695 ) ) ;
#13716 = EDGE_CURVE ( 'NONE', #16751, #14290, #1056, .T. ) ;
#13717 = EDGE_LOOP ( 'NONE', ( #2056, #22609, #7930, #20815 ) ) ;
#13718 = CARTESIAN_POINT ( 'NONE',  ( -40.11286833322908052, 2.887657226147511302, 57.04930799450051637 ) ) ;
#13719 = VERTEX_POINT ( 'NONE', #738 ) ;
#13720 = ADVANCED_FACE ( 'NONE', ( #10605 ), #14662, .T. ) ;
#13721 = CARTESIAN_POINT ( 'NONE',  ( 8.698509210239581790, 31.84164230456639544, 47.04930799450051637 ) ) ;
#13722 = CONICAL_SURFACE ( 'NONE', #1132, 31.50000000000000711, 0.7853981633974482790 ) ;
#13723 = DIRECTION ( 'NONE',  ( 0.4848096202463636484, 0.8746197071393810862, 0.000000000000000000 ) ) ;
#13724 = CARTESIAN_POINT ( 'NONE',  ( 21.09785597605720397, -15.93545420775219945, -24.95069200549946586 ) ) ;
#13725 = VECTOR ( 'NONE', #7265, 1000.000000000000000 ) ;
#13726 = ORIENTED_EDGE ( 'NONE', *, *, #9867, .F. ) ;
#13727 = CARTESIAN_POINT ( 'NONE',  ( 21.09992658989239089, 28.84184655352418858, 47.04930799450051637 ) ) ;
#13728 = CARTESIAN_POINT ( 'NONE',  ( -40.11286833322907341, 2.887657226147505973, 35.04930799450051637 ) ) ;
#13729 = DIRECTION ( 'NONE',  ( -1.101824276508909887E-16, 1.000000000000000000, -0.000000000000000000 ) ) ;
#13730 = CARTESIAN_POINT ( 'NONE',  ( 45.44030796846719511, 22.86454579224779948, 45.92951929762858043 ) ) ;
#13731 = ORIENTED_EDGE ( 'NONE', *, *, #12700, .T. ) ;
#13732 = DIRECTION ( 'NONE',  ( -0.4848096202463430537, -0.8746197071393926326, -9.920727850371701658E-18 ) ) ;
#13733 = CYLINDRICAL_SURFACE ( 'NONE', #7913, 0.1000000000000004774 ) ;
#13734 = LINE ( 'NONE', #24216, #8979 ) ;
#13735 = DIRECTION ( 'NONE',  ( -1.000000000000000000, -1.101824276508909764E-16, 0.000000000000000000 ) ) ;
#13736 = CARTESIAN_POINT ( 'NONE',  ( 44.70507715278255745, 25.56291119454915517, 46.92503878583764987 ) ) ;
#13737 = ORIENTED_EDGE ( 'NONE', *, *, #12546, .T. ) ;
#13738 = CARTESIAN_POINT ( 'NONE',  ( 45.00053793792376666, 28.63655426599985176, 45.68869892245983522 ) ) ;
#13739 = CARTESIAN_POINT ( 'NONE',  ( -40.56960242289638074, 7.470141326141484406, 35.42729059962400839 ) ) ;
#13740 = ORIENTED_EDGE ( 'NONE', *, *, #29020, .T. ) ;
#13741 = DIRECTION ( 'NONE',  ( -0.4441739386571981751, 0.2110602665713104675, -0.8707256032141232893 ) ) ;
#13742 = AXIS2_PLACEMENT_3D ( 'NONE', #17348, #14408, #12277 ) ;
#13743 = CARTESIAN_POINT ( 'NONE',  ( -44.16550389150962985, 1.558238629217585380, 39.44930799450052916 ) ) ;
#13744 = ORIENTED_EDGE ( 'NONE', *, *, #632, .F. ) ;
#13745 = ORIENTED_EDGE ( 'NONE', *, *, #17068, .T. ) ;
#13746 = UNCERTAINTY_MEASURE_WITH_UNIT (LENGTH_MEASURE( 1.000000000000000082E-05 ), #18023, 'distance_accuracy_value', 'NONE');
#13747 = ORIENTED_EDGE ( 'NONE', *, *, #2763, .F. ) ;
#13748 = AXIS2_PLACEMENT_3D ( 'NONE', #4645, #9900, #5137 ) ;
#13749 = ORIENTED_EDGE ( 'NONE', *, *, #11565, .F. ) ;
#13750 = CARTESIAN_POINT ( 'NONE',  ( 33.46699938050304013, 26.46183152705960140, 47.04930799450051637 ) ) ;
#13751 = EDGE_CURVE ( 'NONE', #22393, #10653, #28292, .T. ) ;
#13752 = ORIENTED_EDGE ( 'NONE', *, *, #10572, .T. ) ;
#13753 = ADVANCED_FACE ( 'NONE', ( #5661 ), #15838, .T. ) ;
#13754 = EDGE_CURVE ( 'NONE', #12313, #13235, #24083, .T. ) ;
#13755 = AXIS2_PLACEMENT_3D ( 'NONE', #30201, #17554, #20177 ) ;
#13756 = DIRECTION ( 'NONE',  ( -1.101824276508909887E-16, 1.000000000000000000, -0.000000000000000000 ) ) ;
#13757 = EDGE_CURVE ( 'NONE', #29229, #26728, #11004, .T. ) ;
#13758 = DIRECTION ( 'NONE',  ( 0.8746197071393926326, -0.4848096202463430537, -8.676864087101709653E-18 ) ) ;
#13759 = LINE ( 'NONE', #31157, #16394 ) ;
#13760 = EDGE_CURVE ( 'NONE', #28587, #21198, #21995, .T. ) ;
#13761 = EDGE_CURVE ( 'NONE', #23976, #24923, #14144, .T. ) ;
#13762 = CARTESIAN_POINT ( 'NONE',  ( 48.91284552371730143, 29.53619643316630672, 46.12344667017377020 ) ) ;
#13763 = ORIENTED_EDGE ( 'NONE', *, *, #19817, .F. ) ;
#13764 = VERTEX_POINT ( 'NONE', #6303 ) ;
#13765 = CARTESIAN_POINT ( 'NONE',  ( 21.09785597605719332, 25.76454579224779806, 47.04930799450051637 ) ) ;
#13766 = EDGE_LOOP ( 'NONE', ( #25171, #20963, #32447, #4837 ) ) ;
#13768 = VECTOR ( 'NONE', #4056, 1000.000000000000000 ) ;
#13767 = CARTESIAN_POINT ( 'NONE',  ( 48.38152489017220148, 29.46964073901252590, 48.83753094390939253 ) ) ;
#13769 = DIRECTION ( 'NONE',  ( 0.000000000000000000, 0.000000000000000000, -1.000000000000000000 ) ) ;
#13770 = DIRECTION ( 'NONE',  ( -1.000000000000000000, 0.000000000000000000, 0.000000000000000000 ) ) ;
#13771 = CARTESIAN_POINT ( 'NONE',  ( 21.09785597605720042, -5.935454207752331790, 112.8077566132119927 ) ) ;
#13772 = VECTOR ( 'NONE', #28028, 1000.000000000000000 ) ;
#13773 = CARTESIAN_POINT ( 'NONE',  ( -0.4130478171086108263, 11.86909835304794569, -5.401369334345301532 ) ) ;
#13774 = DIRECTION ( 'NONE',  ( -1.000000000000000000, 0.000000000000000000, 0.000000000000000000 ) ) ;
#13775 = VERTEX_POINT ( 'NONE', #6953 ) ;
#13776 = LINE ( 'NONE', #21298, #2965 ) ;
#13777 = PLANE ( 'NONE',  #27151 ) ;
#13778 = CARTESIAN_POINT ( 'NONE',  ( 21.09992658989239089, 27.72145308207318237, 47.04930799450051637 ) ) ;
#13779 = CARTESIAN_POINT ( 'NONE',  ( 47.71045395478045492, 23.04411619146718238, 46.10501571378621577 ) ) ;
#13780 = ORIENTED_EDGE ( 'NONE', *, *, #2814, .F. ) ;
#13781 = DIRECTION ( 'NONE',  ( -1.000000000000000000, 0.000000000000000000, 0.000000000000000000 ) ) ;
#13782 = ORIENTED_EDGE ( 'NONE', *, *, #23423, .F. ) ;
#13783 = CARTESIAN_POINT ( 'NONE',  ( 8.474859994195282908, 38.56284415653841791, 47.04930799450051637 ) ) ;
#13784 = CARTESIAN_POINT ( 'NONE',  ( -40.37748943095153464, 8.220953018982690708, 59.50788663826320146 ) ) ;
#13785 = VERTEX_POINT ( 'NONE', #21715 ) ;
#13786 = TOROIDAL_SURFACE ( 'NONE', #11163, 46.39830989763677849, 0.4000000000000020206 ) ;
#13787 = AXIS2_PLACEMENT_3D ( 'NONE', #3290, #18384, #675 ) ;
#13788 = EDGE_CURVE ( 'NONE', #9936, #21917, #12581, .T. ) ;
#13789 = CIRCLE ( 'NONE', #16377, 0.1250000000000001110 ) ;
#13790 = VERTEX_POINT ( 'NONE', #29273 ) ;
#13791 = CYLINDRICAL_SURFACE ( 'NONE', #3401, 0.1000000000000008243 ) ;
#13792 = CARTESIAN_POINT ( 'NONE',  ( 21.09785597605719332, 6.547041198165487685, 26.66847926540309288 ) ) ;
#13793 = CARTESIAN_POINT ( 'NONE',  ( -40.60722745863126448, 9.415333058485025219, 39.54930799450052348 ) ) ;
#13794 = ORIENTED_EDGE ( 'NONE', *, *, #12951, .F. ) ;
#13795 = CARTESIAN_POINT ( 'NONE',  ( 3.114080794088355475, -13.30632128221581389, 100.0115811999271500 ) ) ;
#13796 = DIRECTION ( 'NONE',  ( -0.000000000000000000, -1.000000000000000000, 0.000000000000000000 ) ) ;
#13797 = CARTESIAN_POINT ( 'NONE',  ( 77.62364571523254142, -4.258649047046835889, 13.70170648863429896 ) ) ;
#13798 = EDGE_CURVE ( 'NONE', #17347, #18870, #1698, .T. ) ;
#13799 = ORIENTED_EDGE ( 'NONE', *, *, #15397, .T. ) ;
#13800 = DIRECTION ( 'NONE',  ( -2.779292025043186357E-18, 1.288349127009862211E-17, -1.000000000000000000 ) ) ;
#13801 = ORIENTED_EDGE ( 'NONE', *, *, #20650, .F. ) ;
#13802 = CARTESIAN_POINT ( 'NONE',  ( -40.68997348041997952, 6.796928795907699161, 53.64930799450051779 ) ) ;
#13803 = CARTESIAN_POINT ( 'NONE',  ( 48.35473289974373756, 22.86454579224779948, 45.11188864597615833 ) ) ;
#13804 = AXIS2_PLACEMENT_3D ( 'NONE', #24576, #17519, #22109 ) ;
#13805 = DIRECTION ( 'NONE',  ( -1.101824276508909887E-16, 1.000000000000000000, -0.000000000000000000 ) ) ;
#13806 = TOROIDAL_SURFACE ( 'NONE', #31109, 12.61792373059896377, 0.1249999999999977518 ) ;
#13807 =( NAMED_UNIT ( * ) SI_UNIT ( $, .STERADIAN. ) SOLID_ANGLE_UNIT ( ) );
#13808 = ORIENTED_EDGE ( 'NONE', *, *, #18116, .T. ) ;
#13809 = ORIENTED_EDGE ( 'NONE', *, *, #31820, .F. ) ;
#13810 = CARTESIAN_POINT ( 'NONE',  ( 33.46699938050304013, 27.72145308207318237, 47.04930799450050927 ) ) ;
#13811 = DIRECTION ( 'NONE',  ( -1.101824276508909887E-16, 1.000000000000000000, -0.000000000000000000 ) ) ;
#13812 = CONICAL_SURFACE ( 'NONE', #3848, 30.00000000000000000, 0.5934119456780768687 ) ;
#13813 = DIRECTION ( 'NONE',  ( -1.000000000000000000, 0.000000000000000000, 0.000000000000000000 ) ) ;
#13814 = ORIENTED_EDGE ( 'NONE', *, *, #10351, .F. ) ;
#13815 = AXIS2_PLACEMENT_3D ( 'NONE', #16624, #19246, #16309 ) ;
#13816 = CARTESIAN_POINT ( 'NONE',  ( 21.09992658989238734, 31.34164230456639544, 47.04930799450051637 ) ) ;
#13817 = CARTESIAN_POINT ( 'NONE',  ( 36.19429842010744380, -13.74047052604243113, -9.312396943078796951 ) ) ;
#13818 = CIRCLE ( 'NONE', #20085, 0.09999999999999795164 ) ;
#13819 = ADVANCED_FACE ( 'NONE', ( #11388 ), #14345, .T. ) ;
#13820 = ORIENTED_EDGE ( 'NONE', *, *, #13674, .T. ) ;
#13821 = DIRECTION ( 'NONE',  ( -1.224646799147353207E-16, 0.000000000000000000, -1.000000000000000000 ) ) ;
#13822 = CARTESIAN_POINT ( 'NONE',  ( 46.99023568444673060, 25.12451373492760354, 49.12151524109405898 ) ) ;
#13823 = ADVANCED_FACE ( 'NONE', ( #31583 ), #11878, .F. ) ;
#13824 = DIRECTION ( 'NONE',  ( -1.000000000000000000, 0.000000000000000000, 0.000000000000000000 ) ) ;
#13825 = EDGE_CURVE ( 'NONE', #19067, #28626, #4695, .T. ) ;
#13826 = EDGE_CURVE ( 'NONE', #20581, #10115, #23582, .T. ) ;
#13827 = ORIENTED_EDGE ( 'NONE', *, *, #18576, .T. ) ;
#13828 = AXIS2_PLACEMENT_3D ( 'NONE', #31071, #31233, #16116 ) ;
#13829 = CARTESIAN_POINT ( 'NONE',  ( 21.09992658989238734, 38.56284415653841791, 47.04930799450051637 ) ) ;
#13830 = LINE ( 'NONE', #1342, #952 ) ;
#13831 = CARTESIAN_POINT ( 'NONE',  ( 21.09785597605719332, -16.63545420775219696, -37.16074251183835031 ) ) ;
#13832 = CARTESIAN_POINT ( 'NONE',  ( 45.81741271322955100, 25.04452976649966089, 49.02305402274571122 ) ) ;
#13833 = ORIENTED_EDGE ( 'NONE', *, *, #16184, .F. ) ;
#13834 = VECTOR ( 'NONE', #16981, 1000.000000000000114 ) ;
#13835 = CARTESIAN_POINT ( 'NONE',  ( 21.09785597605719332, 15.43591091851532759, 47.04930799450051637 ) ) ;
#13836 = CARTESIAN_POINT ( 'NONE',  ( -41.08312911723392347, 9.261021737272178811, 34.59072935073783128 ) ) ;
#13837 = EDGE_CURVE ( 'NONE', #10473, #11669, #13105, .T. ) ;
#13838 = CARTESIAN_POINT ( 'NONE',  ( 71.79669559076680230, 7.198184577528758510, 17.90250836569788007 ) ) ;
#13839 = ORIENTED_EDGE ( 'NONE', *, *, #28636, .T. ) ;
#13840 = DIRECTION ( 'NONE',  ( 0.000000000000000000, -0.000000000000000000, -1.000000000000000000 ) ) ;
#13841 = FACE_OUTER_BOUND ( 'NONE', #12789, .T. ) ;
#13842 = DIRECTION ( 'NONE',  ( -1.101824276508909887E-16, 1.000000000000000000, -0.000000000000000000 ) ) ;
#13843 = FACE_OUTER_BOUND ( 'NONE', #7511, .T. ) ;
#13844 = ORIENTED_EDGE ( 'NONE', *, *, #25855, .F. ) ;
#13845 = CARTESIAN_POINT ( 'NONE',  ( 48.83862994770794330, 27.25457786121581805, 48.17861352429476796 ) ) ;
#13846 = DIRECTION ( 'NONE',  ( -1.000000000000000000, 0.000000000000000000, 0.000000000000000000 ) ) ;
#13847 = DIRECTION ( 'NONE',  ( -1.101824276508909887E-16, 1.000000000000000000, -0.000000000000000000 ) ) ;
#13848 = CARTESIAN_POINT ( 'NONE',  ( 21.09785597605720753, 16.03967147762301693, 47.04930799450052348 ) ) ;
#13849 = CIRCLE ( 'NONE', #32196, 0.1000000000000006301 ) ;
#13850 = ORIENTED_EDGE ( 'NONE', *, *, #30810, .F. ) ;
#13851 = CARTESIAN_POINT ( 'NONE',  ( 21.09785597605720753, 14.66454579224779842, 47.04930799450052348 ) ) ;
#13852 = CYLINDRICAL_SURFACE ( 'NONE', #9011, 2.000000000000001776 ) ;
#13853 = DIRECTION ( 'NONE',  ( 0.1949050434465282033, -0.6797146636928673713, -0.7071067811865469066 ) ) ;
#13854 = EDGE_CURVE ( 'NONE', #30180, #15469, #30378, .T. ) ;
#13855 = VERTEX_POINT ( 'NONE', #28958 ) ;
#13856 = CYLINDRICAL_SURFACE ( 'NONE', #24093, 0.1000000000000018235 ) ;
#13857 = DIRECTION ( 'NONE',  ( -0.2756373558169959437, 0.9612616959383197823, 0.000000000000000000 ) ) ;
#13858 = TOROIDAL_SURFACE ( 'NONE', #13350, 12.40141737965279667, 0.1249999999999991951 ) ;
#13859 = CARTESIAN_POINT ( 'NONE',  ( 33.50134396954521065, 30.34164230456639544, 47.04930799450051637 ) ) ;
#13860 = EDGE_CURVE ( 'NONE', #14722, #5569, #20951, .T. ) ;
#13861 = DIRECTION ( 'NONE',  ( 0.000000000000000000, -1.000000000000000000, -0.000000000000000000 ) ) ;
#13862 = AXIS2_PLACEMENT_3D ( 'NONE', #22171, #17084, #21842 ) ;
#13863 = ORIENTED_EDGE ( 'NONE', *, *, #2310, .T. ) ;
#13864 = EDGE_LOOP ( 'NONE', ( #2201, #15634, #20976, #2105 ) ) ;
#13865 = EDGE_CURVE ( 'NONE', #12758, #5905, #7849, .T. ) ;
#13866 = VERTEX_POINT ( 'NONE', #16623 ) ;
#13867 = EDGE_CURVE ( 'NONE', #20511, #17141, #29115, .T. ) ;
#13868 = AXIS2_PLACEMENT_3D ( 'NONE', #20691, #5926, #28413 ) ;
#13869 =( BOUNDED_CURVE ( )  B_SPLINE_CURVE ( 2, ( #7250, #2482, #5108 ),
 .UNSPECIFIED., .F., .T. ) 
 B_SPLINE_CURVE_WITH_KNOTS ( ( 3, 3 ),
 ( 0.7892923757256058437, 0.7921717258529592520 ),
 .UNSPECIFIED. ) 
 CURVE ( )  GEOMETRIC_REPRESENTATION_ITEM ( )  RATIONAL_B_SPLINE_CURVE ( ( 0.9479053363475489213, 0.9489966704326912028, 0.9501679776138607370 ) ) 
 REPRESENTATION_ITEM ( '' )  );
#13870 = AXIS2_PLACEMENT_3D ( 'NONE', #20852, #29708, #24122 ) ;
#13871 = CARTESIAN_POINT ( 'NONE',  ( 21.09992658989239089, 25.21664230456640254, 47.04930799450051637 ) ) ;
#13872 = LINE ( 'NONE', #30955, #17161 ) ;
#13873 = AXIS2_PLACEMENT_3D ( 'NONE', #25540, #18467, #32045 ) ;
#13874 = DIRECTION ( 'NONE',  ( -0.000000000000000000, -1.000000000000000000, -0.000000000000000000 ) ) ;
#13875 = AXIS2_PLACEMENT_3D ( 'NONE', #23485, #997, #11021 ) ;
#13876 = CIRCLE ( 'NONE', #32237, 0.1250000000000001110 ) ;
#13877 = ORIENTED_EDGE ( 'NONE', *, *, #29680, .T. ) ;
#13878 = CARTESIAN_POINT ( 'NONE',  ( 21.09785597605719332, 16.33322284159648063, 47.04930799450051637 ) ) ;
#13879 = ORIENTED_EDGE ( 'NONE', *, *, #9183, .F. ) ;
#13880 = AXIS2_PLACEMENT_3D ( 'NONE', #16557, #26575, #11652 ) ;
#13881 = FACE_OUTER_BOUND ( 'NONE', #18529, .T. ) ;
#13882 = DIRECTION ( 'NONE',  ( 0.8746197071393926326, -0.4848096202463430537, -8.676864087101709653E-18 ) ) ;
#13883 = CARTESIAN_POINT ( 'NONE',  ( 21.09992658989238734, 32.09164230456639899, 47.04930799450051637 ) ) ;
#13884 = ORIENTED_EDGE ( 'NONE', *, *, #27912, .F. ) ;
#13885 = CYLINDRICAL_SURFACE ( 'NONE', #17574, 7.999999999999996447 ) ;
#13886 = CARTESIAN_POINT ( 'NONE',  ( 21.09785597605719332, 42.30003263981368633, 47.04930799450051637 ) ) ;
#13887 = DIRECTION ( 'NONE',  ( -1.000000000000000000, 0.000000000000000000, 0.000000000000000000 ) ) ;
#13888 = CARTESIAN_POINT ( 'NONE',  ( 45.42945060211348363, 22.93328494799376216, 46.63886900051237916 ) ) ;
#13889 = VERTEX_POINT ( 'NONE', #1864 ) ;
#13890 = CARTESIAN_POINT ( 'NONE',  ( 47.33512057650604277, 22.89977464660286444, 45.20042056806582309 ) ) ;
#13891 = FACE_OUTER_BOUND ( 'NONE', #25148, .T. ) ;
#13892 = DIRECTION ( 'NONE',  ( -1.224646799147353207E-16, 0.000000000000000000, -1.000000000000000000 ) ) ;
#13893 = PLANE ( 'NONE',  #14882 ) ;
#13894 = SURFACE_SIDE_STYLE ('',( #6984 ) ) ;
#13895 = VERTEX_POINT ( 'NONE', #18921 ) ;
#13896 = DIRECTION ( 'NONE',  ( -0.000000000000000000, -1.000000000000000000, -0.000000000000000000 ) ) ;
#13897 = CARTESIAN_POINT ( 'NONE',  ( -40.23971823762673239, 6.784144620117123381, 60.44930799450051495 ) ) ;
#13898 = EDGE_CURVE ( 'NONE', #31626, #23399, #24179, .T. ) ;
#13899 = ORIENTED_EDGE ( 'NONE', *, *, #1985, .T. ) ;
#13900 = CARTESIAN_POINT ( 'NONE',  ( 47.09785597605719687, 15.77906836436399374, 47.04930799450078638 ) ) ;
#13901 = EDGE_CURVE ( 'NONE', #28492, #31580, #8373, .T. ) ;
#13902 = DIRECTION ( 'NONE',  ( -0.3935310072385434510, 0.5000000000000004441, -0.7714488617801033010 ) ) ;
#13903 = EDGE_LOOP ( 'NONE', ( #14403, #326, #1003, #18131 ) ) ;
#13904 = VECTOR ( 'NONE', #30191, 1000.000000000000000 ) ;
#13905 = EDGE_LOOP ( 'NONE', ( #26203, #12178 ) ) ;
#13906 = AXIS2_PLACEMENT_3D ( 'NONE', #23327, #8553, #838 ) ;
#13907 = CIRCLE ( 'NONE', #24922, 12.36707279061065279 ) ;
#13908 = CIRCLE ( 'NONE', #13396, 40.48742189997368257 ) ;
#13909 = EDGE_CURVE ( 'NONE', #21141, #5136, #6629, .T. ) ;
#13910 = VECTOR ( 'NONE', #12298, 1000.000000000000000 ) ;
#13911 = ORIENTED_EDGE ( 'NONE', *, *, #31875, .T. ) ;
#13912 = EDGE_CURVE ( 'NONE', #29041, #20681, #18757, .T. ) ;
#13913 = ORIENTED_EDGE ( 'NONE', *, *, #14633, .F. ) ;
#13914 = DIRECTION ( 'NONE',  ( 0.9612616959383205595, 0.2756373558169930571, -1.660411357259282199E-16 ) ) ;
#13915 = ORIENTED_EDGE ( 'NONE', *, *, #6962, .T. ) ;
#13916 = FACE_OUTER_BOUND ( 'NONE', #27284, .T. ) ;
#13917 = FACE_OUTER_BOUND ( 'NONE', #25015, .T. ) ;
#13918 = DIRECTION ( 'NONE',  ( -1.101824276508909887E-16, 1.000000000000000000, -0.000000000000000000 ) ) ;
#13919 = FACE_OUTER_BOUND ( 'NONE', #14893, .T. ) ;
#13920 = AXIS2_PLACEMENT_3D ( 'NONE', #11987, #4924, #157 ) ;
#13921 = CARTESIAN_POINT ( 'NONE',  ( 44.74832014356462651, 29.12786309983297883, 46.92728461490987257 ) ) ;
#13922 = EDGE_LOOP ( 'NONE', ( #20591, #11670, #4115, #4914 ) ) ;
#13923 = ORIENTED_EDGE ( 'NONE', *, *, #2442, .T. ) ;
#13925 = CARTESIAN_POINT ( 'NONE',  ( -12.35638036371648774, -4.032327822094595504, -8.334620977867299274 ) ) ;
#13924 = CIRCLE ( 'NONE', #14472, 40.48742189997368257 ) ;
#13926 =( GEOMETRIC_REPRESENTATION_CONTEXT ( 3 ) GLOBAL_UNCERTAINTY_ASSIGNED_CONTEXT ( ( #25563 ) ) GLOBAL_UNIT_ASSIGNED_CONTEXT ( ( #30924, #18906, #14003 ) ) REPRESENTATION_CONTEXT ( 'NONE', 'WORKASPACE' ) );
#13927 = ORIENTED_EDGE ( 'NONE', *, *, #11827, .T. ) ;
#13928 = CARTESIAN_POINT ( 'NONE',  ( 49.13594796351935656, 29.51161737861004397, 47.76250447815154843 ) ) ;
#13929 = CARTESIAN_POINT ( 'NONE',  ( -40.60023598829667435, 7.576973264584798251, 38.76008276981544753 ) ) ;
#13930 = AXIS2_PLACEMENT_3D ( 'NONE', #29290, #29625, #31440 ) ;
#13931 = CARTESIAN_POINT ( 'NONE',  ( -42.38263560350583248, 14.61917486843862868, 60.54930799450051637 ) ) ;
#13932 = PLANE ( 'NONE',  #2243 ) ;
#13933 = CARTESIAN_POINT ( 'NONE',  ( 45.46000861347822308, 27.47287913140504045, 49.57397645940629616 ) ) ;
#13934 = CYLINDRICAL_SURFACE ( 'NONE', #22046, 1.199999999999999734 ) ;
#13935 = CARTESIAN_POINT ( 'NONE',  ( 21.09785597605719332, 40.56454579224780588, 77.04930799450052348 ) ) ;
#13936 = ORIENTED_EDGE ( 'NONE', *, *, #31395, .F. ) ;
#13937 = DIRECTION ( 'NONE',  ( -1.000000000000000000, 0.000000000000000000, 0.000000000000000000 ) ) ;
#13938 = CARTESIAN_POINT ( 'NONE',  ( 8.732853799281732776, 31.46183152705961561, 47.04930799450051637 ) ) ;
#13939 = CARTESIAN_POINT ( 'NONE',  ( 21.09785597605719332, 30.56454579224779522, 47.04930799450051637 ) ) ;
#13940 = AXIS2_PLACEMENT_3D ( 'NONE', #23948, #24113, #32326 ) ;
#13941 = CARTESIAN_POINT ( 'NONE',  ( 47.37889090789306579, 23.12036939723557083, 47.06390358666074292 ) ) ;
#13942 = CARTESIAN_POINT ( 'NONE',  ( -41.08785830660041682, 9.277514380576530328, 39.54930799450052348 ) ) ;
#13943 = EDGE_LOOP ( 'NONE', ( #8685, #16111, #28149, #13949 ) ) ;
#13944 = DIRECTION ( 'NONE',  ( 0.8746197071393926326, -0.4848096202463430537, -8.676864087101709653E-18 ) ) ;
#13945 = VERTEX_POINT ( 'NONE', #29444 ) ;
#13946 = DIRECTION ( 'NONE',  ( -1.000000000000000000, 0.000000000000000000, 0.000000000000000000 ) ) ;
#13947 = DIRECTION ( 'NONE',  ( -1.000000000000000000, -1.101824276508909764E-16, 0.000000000000000000 ) ) ;
#13948 = EDGE_CURVE ( 'NONE', #1796, #21091, #15198, .T. ) ;
#13949 = ORIENTED_EDGE ( 'NONE', *, *, #30504, .F. ) ;
#13950 = EDGE_CURVE ( 'NONE', #25630, #16490, #22701, .T. ) ;
#13951 = EDGE_CURVE ( 'NONE', #14214, #30931, #30918, .T. ) ;
#13952 = EDGE_CURVE ( 'NONE', #18438, #24996, #6266, .T. ) ;
#13953 = VECTOR ( 'NONE', #10715, 1000.000000000000000 ) ;
#13954 = AXIS2_PLACEMENT_3D ( 'NONE', #12157, #11494, #11990 ) ;
#13955 = ORIENTED_EDGE ( 'NONE', *, *, #12660, .T. ) ;
#13956 = DIRECTION ( 'NONE',  ( 1.224646799147353207E-16, -0.000000000000000000, -1.000000000000000000 ) ) ;
#13957 = DIRECTION ( 'NONE',  ( -0.000000000000000000, -1.000000000000000000, 0.000000000000000000 ) ) ;
#13958 = LINE ( 'NONE', #23949, #28322 ) ;
#13959 = AXIS2_PLACEMENT_3D ( 'NONE', #27143, #9762, #27317 ) ;
#13960 = EDGE_LOOP ( 'NONE', ( #14061, #24807, #6341, #18938 ) ) ;
#13961 = DIRECTION ( 'NONE',  ( -1.000000000000000000, 0.000000000000000000, 0.000000000000000000 ) ) ;
#13962 = PLANE ( 'NONE',  #25925 ) ;
#13963 = CARTESIAN_POINT ( 'NONE',  ( -40.06503689199337259, 6.934220188908800431, 39.11858639832014717 ) ) ;
#13964 = B_SPLINE_CURVE_WITH_KNOTS ( 'NONE', 3,
 ( #19685, #19524, #29383, #1809, #29058, #31846, #14615, #6578 ),
 .UNSPECIFIED., .F., .F.,
 ( 4, 2, 2, 4 ),
 ( 8.560449982191426041E-05, 0.0006851562598348886557, 0.0009849321398413680810, 0.001284708019847847615 ),
 .UNSPECIFIED. ) ;
#13965 = VERTEX_POINT ( 'NONE', #27301 ) ;
#13966 = DIRECTION ( 'NONE',  ( -1.000000000000000000, 0.000000000000000000, 0.000000000000000000 ) ) ;
#13967 = ORIENTED_EDGE ( 'NONE', *, *, #9944, .T. ) ;
#13968 = CARTESIAN_POINT ( 'NONE',  ( 21.09785597605719332, 11.92558985988973497, 47.04930799450051637 ) ) ;
#13969 = CARTESIAN_POINT ( 'NONE',  ( 21.09785597605719332, 15.24673779880127356, 47.04930799450051637 ) ) ;
#13970 = DIRECTION ( 'NONE',  ( -0.8746197071393805311, 0.4848096202463645921, 1.277302113040265530E-17 ) ) ;
#13971 = CARTESIAN_POINT ( 'NONE',  ( 0.000000000000000000, 0.000000000000000000, 0.000000000000000000 ) ) ;
#13972 = ORIENTED_EDGE ( 'NONE', *, *, #30298, .F. ) ;
#13973 = ORIENTED_EDGE ( 'NONE', *, *, #14063, .T. ) ;
#13974 = CARTESIAN_POINT ( 'NONE',  ( 55.14312657641617932, -13.30632128221581212, 2.672082950226034370 ) ) ;
#13975 = AXIS2_PLACEMENT_3D ( 'NONE', #13612, #8206, #23617 ) ;
#13976 = CARTESIAN_POINT ( 'NONE',  ( -41.51232591312490428, 10.75780884251261682, 36.23067884439899444 ) ) ;
#13977 = DIRECTION ( 'NONE',  ( -1.000000000000000000, -1.101824276508909887E-16, 0.000000000000000000 ) ) ;
#13978 = VERTEX_POINT ( 'NONE', #30258 ) ;
#13979 = CARTESIAN_POINT ( 'NONE',  ( -12.63275441008301669, -2.304636120132624644, -7.982147193627917581 ) ) ;
#13980 = DIRECTION ( 'NONE',  ( -1.224646799147353207E-16, -1.349345573449484691E-32, 1.000000000000000000 ) ) ;
#13981 = ORIENTED_EDGE ( 'NONE', *, *, #9949, .F. ) ;
#13982 = CARTESIAN_POINT ( 'NONE',  ( 21.09785597605719332, 17.16451738380053627, 59.53344952167761761 ) ) ;
#13983 = CARTESIAN_POINT ( 'NONE',  ( 46.96268396749378127, 27.53121246473837402, 49.65201805493727960 ) ) ;
#13984 = AXIS2_PLACEMENT_3D ( 'NONE', #24473, #4786, #12179 ) ;
#13985 = DIRECTION ( 'NONE',  ( -1.000000000000000000, 0.000000000000000000, 0.000000000000000000 ) ) ;
#13986 = ADVANCED_FACE ( 'NONE', ( #12041 ), #8026, .F. ) ;
#13987 = EDGE_CURVE ( 'NONE', #30065, #13965, #7324, .T. ) ;
#13988 = EDGE_CURVE ( 'NONE', #29931, #25766, #2362, .T. ) ;
#13989 = EDGE_CURVE ( 'NONE', #5841, #3723, #24601, .T. ) ;
#13990 = ORIENTED_EDGE ( 'NONE', *, *, #8537, .T. ) ;
#13991 = DIRECTION ( 'NONE',  ( 0.000000000000000000, 0.000000000000000000, 1.000000000000000000 ) ) ;
#13992 = FACE_BOUND ( 'NONE', #11984, .T. ) ;
#13993 = AXIS2_PLACEMENT_3D ( 'NONE', #28623, #22199, #27126 ) ;
#13994 = DIRECTION ( 'NONE',  ( -1.224646799147353207E-16, -1.349345573449484691E-32, 1.000000000000000000 ) ) ;
#13995 = CARTESIAN_POINT ( 'NONE',  ( 45.24946171279598417, 28.50784706826092929, 47.99220971130007030 ) ) ;
#13996 = ORIENTED_EDGE ( 'NONE', *, *, #6859, .F. ) ;
#13997 = CARTESIAN_POINT ( 'NONE',  ( 21.09992658989239089, 30.34164230456639544, 47.04930799450051637 ) ) ;
#13998 = CARTESIAN_POINT ( 'NONE',  ( -33.00214402394279745, 14.66454579224780019, 47.04930799450052348 ) ) ;
#13999 = DIRECTION ( 'NONE',  ( 0.000000000000000000, -0.000000000000000000, 1.000000000000000000 ) ) ;
#14000 = FACE_OUTER_BOUND ( 'NONE', #26837, .T. ) ;
#14001 = LINE ( 'NONE', #23836, #23619 ) ;
#14002 = CARTESIAN_POINT ( 'NONE',  ( 21.09992658989239089, 29.59164230456639899, 47.04930799450051637 ) ) ;
#14003 =( NAMED_UNIT ( * ) SI_UNIT ( $, .STERADIAN. ) SOLID_ANGLE_UNIT ( ) );
#14004 = VERTEX_POINT ( 'NONE', #5144 ) ;
#14005 = EDGE_CURVE ( 'NONE', #8819, #7068, #4205, .T. ) ;
#14006 = FACE_OUTER_BOUND ( 'NONE', #12643, .T. ) ;
#14007 = CARTESIAN_POINT ( 'NONE',  ( 44.70507715278255034, 27.66291119454915304, 46.92503878583765697 ) ) ;
#14008 = EDGE_CURVE ( 'NONE', #26439, #28177, #17837, .T. ) ;
#14009 = CARTESIAN_POINT ( 'NONE',  ( 21.09992658989238734, 38.56284415653841791, 47.04930799450051637 ) ) ;
#14010 = DIRECTION ( 'NONE',  ( -1.101824276508909887E-16, 1.000000000000000000, -0.000000000000000000 ) ) ;
#14011 = FACE_OUTER_BOUND ( 'NONE', #7268, .T. ) ;
#14012 = EDGE_LOOP ( 'NONE', ( #6632, #302, #21720, #31603 ) ) ;
#14013 = CARTESIAN_POINT ( 'NONE',  ( -39.57165970433088376, -5.936116385392971040, 77.92184100968836447 ) ) ;
#14014 = FACE_OUTER_BOUND ( 'NONE', #13864, .T. ) ;
#14015 = CYLINDRICAL_SURFACE ( 'NONE', #7863, 22.00000000000000000 ) ;
#14016 = EDGE_LOOP ( 'NONE', ( #3529, #13551, #25733, #16917 ) ) ;
#14017 = CARTESIAN_POINT ( 'NONE',  ( 21.09992658989239089, 28.09164230456639544, 47.04930799450051637 ) ) ;
#14018 = FACE_OUTER_BOUND ( 'NONE', #16607, .T. ) ;
#14019 = VECTOR ( 'NONE', #17603, 1000.000000000000000 ) ;
#14020 = DIRECTION ( 'NONE',  ( 0.4848096202463673676, 0.8746197071393789768, 0.000000000000000000 ) ) ;
#14021 = DIRECTION ( 'NONE',  ( -0.000000000000000000, -1.000000000000000000, 0.000000000000000000 ) ) ;
#14022 = ORIENTED_EDGE ( 'NONE', *, *, #6625, .T. ) ;
#14023 = CARTESIAN_POINT ( 'NONE',  ( 73.18954489356450210, 11.69686719848734313, 24.43675172218812008 ) ) ;
#14024 = AXIS2_PLACEMENT_3D ( 'NONE', #1046, #23693, #11072 ) ;
#14025 = ORIENTED_EDGE ( 'NONE', *, *, #19599, .T. ) ;
#14026 = EDGE_CURVE ( 'NONE', #22237, #13235, #14673, .T. ) ;
#14027 = ORIENTED_EDGE ( 'NONE', *, *, #25645, .T. ) ;
#14028 = EDGE_CURVE ( 'NONE', #29883, #2441, #22207, .T. ) ;
#14029 = DIRECTION ( 'NONE',  ( -0.000000000000000000, -1.000000000000000000, -0.000000000000000000 ) ) ;
#14030 = CARTESIAN_POINT ( 'NONE',  ( -29.74268752149416173, 11.25807467393579309, 71.06788596905158784 ) ) ;
#14031 = DIRECTION ( 'NONE',  ( -1.000000000000000000, 0.000000000000000000, 0.000000000000000000 ) ) ;
#14032 = TOROIDAL_SURFACE ( 'NONE', #4069, 1.299999999999999822, 0.1000000000000000056 ) ;
#14033 = AXIS2_PLACEMENT_3D ( 'NONE', #31015, #21300, #30853 ) ;
#14034 = EDGE_CURVE ( 'NONE', #5457, #8522, #8401, .T. ) ;
#14035 = EDGE_LOOP ( 'NONE', ( #6779, #31463, #10869, #8348 ) ) ;
#14036 = CARTESIAN_POINT ( 'NONE',  ( 21.09785597605719332, 48.06454579224779877, 47.04930799450051637 ) ) ;
#14037 = ORIENTED_EDGE ( 'NONE', *, *, #396, .F. ) ;
#14038 = DIRECTION ( 'NONE',  ( -1.101824276508909887E-16, 1.000000000000000000, -0.000000000000000000 ) ) ;
#14039 = CIRCLE ( 'NONE', #11959, 12.36707279061065101 ) ;
#14040 = EDGE_LOOP ( 'NONE', ( #5058, #30549, #3527, #28291 ) ) ;
#14041 = ADVANCED_FACE ( 'NONE', ( #22530 ), #14, .F. ) ;
#14042 = DIRECTION ( 'NONE',  ( -1.101824276508909887E-16, 1.000000000000000000, -0.000000000000000000 ) ) ;
#14043 = DIRECTION ( 'NONE',  ( -1.000000000000000000, 0.000000000000000000, 0.000000000000000000 ) ) ;
#14044 = DIRECTION ( 'NONE',  ( -0.000000000000000000, -1.000000000000000000, -0.000000000000000000 ) ) ;
#14045 = PLANE ( 'NONE',  #12678 ) ;
#14046 = EDGE_CURVE ( 'NONE', #16322, #30017, #27470, .T. ) ;
#14047 = ORIENTED_EDGE ( 'NONE', *, *, #161, .F. ) ;
#14048 = CARTESIAN_POINT ( 'NONE',  ( 46.33059210211230550, 22.93807716476589675, 45.54522087609679204 ) ) ;
#14049 = DIRECTION ( 'NONE',  ( -0.6184495258776595561, 0.3428121700606653888, -0.7071067811865444641 ) ) ;
#14050 = AXIS2_PLACEMENT_3D ( 'NONE', #16160, #11246, #28163 ) ;
#14051 = CARTESIAN_POINT ( 'NONE',  ( 33.50134396954526750, 25.09164230456639899, 47.04930799450051637 ) ) ;
#14052 = DIRECTION ( 'NONE',  ( -1.101824276508909887E-16, 1.000000000000000000, -0.000000000000000000 ) ) ;
#14053 = EDGE_CURVE ( 'NONE', #26270, #649, #15000, .T. ) ;
#14054 = DIRECTION ( 'NONE',  ( 6.848137993413698342E-17, -0.8290375725550389596, 0.5591929034707507906 ) ) ;
#14055 = ORIENTED_EDGE ( 'NONE', *, *, #21700, .T. ) ;
#14056 = DIRECTION ( 'NONE',  ( 0.000000000000000000, 1.000000000000000000, 0.000000000000000000 ) ) ;
#14057 = CARTESIAN_POINT ( 'NONE',  ( -40.89289694005993425, 10.41158093418393094, 36.52712545380572351 ) ) ;
#14058 = ORIENTED_EDGE ( 'NONE', *, *, #21689, .F. ) ;
#14059 = CARTESIAN_POINT ( 'NONE',  ( -43.68921302925062378, 1.179890886355840163, 39.44930799450052916 ) ) ;
#14060 = DIRECTION ( 'NONE',  ( 0.8746197071393925215, -0.4848096202463429982, -8.676864087101708112E-18 ) ) ;
#14061 = ORIENTED_EDGE ( 'NONE', *, *, #21884, .F. ) ;
#14062 = ORIENTED_EDGE ( 'NONE', *, *, #3589, .T. ) ;
#14063 = EDGE_CURVE ( 'NONE', #5136, #17834, #60, .T. ) ;
#14064 = AXIS2_PLACEMENT_3D ( 'NONE', #30427, #378, #12385 ) ;
#14065 = UNCERTAINTY_MEASURE_WITH_UNIT (LENGTH_MEASURE( 1.000000000000000082E-05 ), #9888, 'distance_accuracy_value', 'NONE');
#14066 = CIRCLE ( 'NONE', #29782, 48.63405236513555963 ) ;
#14067 = ORIENTED_EDGE ( 'NONE', *, *, #13909, .T. ) ;
#14068 =( BOUNDED_CURVE ( )  B_SPLINE_CURVE ( 2, ( #29251, #28940, #16451, #24165, #16771, #8745, #11065, #11705, #11372 ),
 .UNSPECIFIED., .F., .F. ) 
 B_SPLINE_CURVE_WITH_KNOTS ( ( 3, 2, 2, 2, 3 ),
 ( 0.5357142845530131758, 0.5476190476190476719, 0.5714285714285713969, 0.5952380952380952328, 0.6071428559815844617 ),
 .UNSPECIFIED. ) 
 CURVE ( )  GEOMETRIC_REPRESENTATION_ITEM ( )  RATIONAL_B_SPLINE_CURVE ( ( 0.9330127018922200755, 0.9330126953578163906, 1.000000000000000000, 0.8660254037844387076, 1.000000000000000000, 0.8660254037844387076, 1.000000000000000000, 0.9330127084266230941, 0.9330127018922200755 ) ) 
 REPRESENTATION_ITEM ( '' )  );
#14069 = AXIS2_PLACEMENT_3D ( 'NONE', #5023, #15033, #9939 ) ;
#14070 = CIRCLE ( 'NONE', #24765, 1.000000000001013856 ) ;
#14071 = ADVANCED_FACE ( 'NONE', ( #2682 ), #372, .T. ) ;
#14072 = DIRECTION ( 'NONE',  ( -1.188208965918164993E-16, -1.880121038077813132E-16, -1.000000000000000000 ) ) ;
#14073 = ADVANCED_FACE ( 'NONE', ( #27953 ), #24595, .T. ) ;
#14074 = EDGE_LOOP ( 'NONE', ( #17514, #21164, #31110, #15095 ) ) ;
#14075 = DIRECTION ( 'NONE',  ( 0.000000000000000000, -1.000000000000000000, 0.000000000000000000 ) ) ;
#14076 = DIRECTION ( 'NONE',  ( -1.000000000000000000, 0.000000000000000000, 0.000000000000000000 ) ) ;
#14077 = DIRECTION ( 'NONE',  ( -1.096245967261387844E-16, 0.000000000000000000, 1.000000000000000000 ) ) ;
#14078 = CARTESIAN_POINT ( 'NONE',  ( -40.50800117262852496, 7.569618128341433660, 53.85120749494056724 ) ) ;
#14079 = CARTESIAN_POINT ( 'NONE',  ( 46.99218062947583974, 26.50286309983298949, 49.08406571254116102 ) ) ;
#14080 = ORIENTED_EDGE ( 'NONE', *, *, #20200, .F. ) ;
#14081 = VERTEX_POINT ( 'NONE', #32201 ) ;
#14082 = DIRECTION ( 'NONE',  ( -0.01254734031692028573, 0.9702957262759968060, 0.2415962909928611735 ) ) ;
#14083 = ADVANCED_FACE ( 'NONE', ( #32364 ), #15725, .T. ) ;
#14084 = ORIENTED_EDGE ( 'NONE', *, *, #4528, .T. ) ;
#14085 = CARTESIAN_POINT ( 'NONE',  ( -43.86882709718853590, -0.1754741395363378920, 32.14930799450051779 ) ) ;
#14086 = DIRECTION ( 'NONE',  ( 0.2756373558170082672, -0.9612616959383162296, 0.000000000000000000 ) ) ;
#14087 = CIRCLE ( 'NONE', #24026, 12.62506659569710266 ) ;
#14088 = CARTESIAN_POINT ( 'NONE',  ( -40.55615437192444261, 7.233232712785302887, 38.86959707880754422 ) ) ;
#14089 = CARTESIAN_POINT ( 'NONE',  ( 47.79865503179234310, 9.702389020015065313, 97.51081847724526597 ) ) ;
#14090 = FACE_BOUND ( 'NONE', #23411, .T. ) ;
#14091 = ADVANCED_FACE ( 'NONE', ( #19711 ), #11032, .T. ) ;
#14092 = CARTESIAN_POINT ( 'NONE',  ( 44.09250526802607340, 25.95621246473837829, 46.89322480343881949 ) ) ;
#14093 = CIRCLE ( 'NONE', #4123, 0.1000000000000008243 ) ;
#14094 = CARTESIAN_POINT ( 'NONE',  ( 47.09785597605719687, 23.12036939723557083, 47.04930799450080059 ) ) ;
#14095 = DIRECTION ( 'NONE',  ( -1.000000000000000000, 0.000000000000000000, 0.000000000000000000 ) ) ;
#14096 = VERTEX_POINT ( 'NONE', #12344 ) ;
#14097 = DIRECTION ( 'NONE',  ( 1.000000000000000000, -0.000000000000000000, -0.000000000000000000 ) ) ;
#14098 = CARTESIAN_POINT ( 'NONE',  ( 71.55936645880184699, 9.702389020015065313, 73.75010705023584023 ) ) ;
#14099 = DIRECTION ( 'NONE',  ( -1.000000000000000000, 0.000000000000000000, -1.110223024625155594E-14 ) ) ;
#14100 = AXIS2_PLACEMENT_3D ( 'NONE', #16907, #17399, #24957 ) ;
#14101 = CARTESIAN_POINT ( 'NONE',  ( 21.09785597605719332, 24.56454579224780232, 47.04930799450051637 ) ) ;
#14102 = CARTESIAN_POINT ( 'NONE',  ( 46.55854765242722237, 25.74696019071911124, 44.51792966461573542 ) ) ;
#14103 = ORIENTED_EDGE ( 'NONE', *, *, #12216, .F. ) ;
#14104 = DIRECTION ( 'NONE',  ( -0.000000000000000000, -1.000000000000000000, 0.000000000000000000 ) ) ;
#14105 = VERTEX_POINT ( 'NONE', #7251 ) ;
#14106 = LINE ( 'NONE', #24760, #494 ) ;
#14107 = CARTESIAN_POINT ( 'NONE',  ( 21.09785597605719332, 40.06454579224778456, 47.04930799450051637 ) ) ;
#14108 = ORIENTED_EDGE ( 'NONE', *, *, #29621, .T. ) ;
#14109 = AXIS2_PLACEMENT_3D ( 'NONE', #2287, #15086, #20164 ) ;
#14110 = AXIS2_PLACEMENT_3D ( 'NONE', #17281, #1867, #19418 ) ;
#14111 = ORIENTED_EDGE ( 'NONE', *, *, #8574, .T. ) ;
#14112 = DIRECTION ( 'NONE',  ( 0.000000000000000000, -0.7071067811865378028, -0.7071067811865573427 ) ) ;
#14113 = DIRECTION ( 'NONE',  ( -1.000000000000000000, -1.101824276508909887E-16, 0.000000000000000000 ) ) ;
#14114 = AXIS2_PLACEMENT_3D ( 'NONE', #11995, #7, #24788 ) ;
#14115 = ORIENTED_EDGE ( 'NONE', *, *, #7949, .F. ) ;
#14116 = CARTESIAN_POINT ( 'NONE',  ( 21.09992658989238734, 38.56284415653841791, 47.04930799450051637 ) ) ;
#14117 = AXIS2_PLACEMENT_3D ( 'NONE', #12498, #22481, #11 ) ;
#14118 = DIRECTION ( 'NONE',  ( -0.000000000000000000, -1.000000000000000000, 0.000000000000000000 ) ) ;
#14119 = DIRECTION ( 'NONE',  ( 0.000000000000000000, 0.000000000000000000, 1.000000000000000000 ) ) ;
#14120 = ORIENTED_EDGE ( 'NONE', *, *, #4018, .F. ) ;
#14121 = CARTESIAN_POINT ( 'NONE',  ( 8.732853799281732776, 38.56284415653841791, 47.04930799450051637 ) ) ;
#14122 = EDGE_CURVE ( 'NONE', #13542, #17767, #27095, .T. ) ;
#14123 = EDGE_LOOP ( 'NONE', ( #13780, #11419 ) ) ;
#14124 = DIRECTION ( 'NONE',  ( 0.000000000000000000, 0.000000000000000000, -1.000000000000000000 ) ) ;
#14125 = CARTESIAN_POINT ( 'NONE',  ( 48.23388202445966044, 29.05087065737811969, 49.27628909396056400 ) ) ;
#14126 = ADVANCED_FACE ( 'NONE', ( #13320 ), #10490, .F. ) ;
#14127 = CARTESIAN_POINT ( 'NONE',  ( -40.32034427004700916, 8.384459687302960873, 59.64930799450051779 ) ) ;
#14128 = DIRECTION ( 'NONE',  ( 1.000000000000000000, 0.000000000000000000, 0.000000000000000000 ) ) ;
#14129 = EDGE_LOOP ( 'NONE', ( #23575, #17191, #27055, #16174 ) ) ;
#14130 = ORIENTED_EDGE ( 'NONE', *, *, #10654, .F. ) ;
#14131 =( REPRESENTATION_RELATIONSHIP ('NONE','NONE', #20382, #12446 ) REPRESENTATION_RELATIONSHIP_WITH_TRANSFORMATION ( #30365 )SHAPE_REPRESENTATION_RELATIONSHIP( ) );
#14132 = CARTESIAN_POINT ( 'NONE',  ( -43.35833523721896654, -3.935454207752183020, 52.04930799450050927 ) ) ;
#14133 = CIRCLE ( 'NONE', #7834, 55.53141649511111666 ) ;
#14134 = DIRECTION ( 'NONE',  ( 0.000000000000000000, 0.000000000000000000, 1.000000000000000000 ) ) ;
#14135 = AXIS2_PLACEMENT_3D ( 'NONE', #5660, #251, #15666 ) ;
#14136 = CARTESIAN_POINT ( 'NONE',  ( 47.09785597605719687, 29.86454579224779948, 47.04930799450078638 ) ) ;
#14137 = ORIENTED_EDGE ( 'NONE', *, *, #23578, .F. ) ;
#14138 = CARTESIAN_POINT ( 'NONE',  ( -5.929450684728940324, 9.438446991585315970, -4.311106055539630333 ) ) ;
#14139 = CARTESIAN_POINT ( 'NONE',  ( 21.09992658989239089, 30.59164230456639544, 47.04930799450051637 ) ) ;
#14140 = ORIENTED_EDGE ( 'NONE', *, *, #29399, .F. ) ;
#14141 = DIRECTION ( 'NONE',  ( -1.000000000000000000, 0.000000000000000000, 0.000000000000000000 ) ) ;
#14142 = CARTESIAN_POINT ( 'NONE',  ( 21.09992658989239089, 26.34164230456639899, 47.04930799450051637 ) ) ;
#14143 = TOROIDAL_SURFACE ( 'NONE', #4169, 12.40141737965281266, 0.1249999999999994865 ) ;
#14144 = CIRCLE ( 'NONE', #3654, 2.500000000000002220 ) ;
#14145 = DIRECTION ( 'NONE',  ( 1.000000000000000000, 0.000000000000000000, -1.224646799147353207E-16 ) ) ;
#14146 = AXIS2_PLACEMENT_3D ( 'NONE', #9826, #457, #14917 ) ;
#14147 = AXIS2_PLACEMENT_3D ( 'NONE', #1204, #3506, #16465 ) ;
#14148 = ORIENTED_EDGE ( 'NONE', *, *, #3336, .F. ) ;
#14149 = CARTESIAN_POINT ( 'NONE',  ( 21.09785597605720397, -16.63545420775219696, 119.2593585008392978 ) ) ;
#14150 = FACE_OUTER_BOUND ( 'NONE', #2947, .T. ) ;
#14151 = DIRECTION ( 'NONE',  ( -0.8746197071393926326, 0.4848096202463430537, 8.676864087101709653E-18 ) ) ;
#14152 = CARTESIAN_POINT ( 'NONE',  ( 49.49063479933183629, 28.79951373492759359, 47.17357720316391578 ) ) ;
#14153 = AXIS2_PLACEMENT_3D ( 'NONE', #27643, #22059, #17130 ) ;
#14154 = TOROIDAL_SURFACE ( 'NONE', #3125, 12.40141737965284463, 0.1250000000000005274 ) ;
#14155 = ORIENTED_EDGE ( 'NONE', *, *, #14163, .T. ) ;
#14156 = DIRECTION ( 'NONE',  ( 0.9612616959383193382, 0.2756373558169973870, 8.795445018804928853E-19 ) ) ;
#14157 = DIRECTION ( 'NONE',  ( 0.000000000000000000, 0.000000000000000000, 1.000000000000000000 ) ) ;
#14158 = DIRECTION ( 'NONE',  ( 0.3428121700606596711, 0.6184495258776487869, 0.7071067811865565655 ) ) ;
#14159 = CONICAL_SURFACE ( 'NONE', #23087, 31.50000000000000711, 0.7853981633974482790 ) ;
#14160 = AXIS2_PLACEMENT_3D ( 'NONE', #8069, #340, #16080 ) ;
#14161 = DIRECTION ( 'NONE',  ( -0.9986540920324801229, -6.158269594508763597E-17, -0.05186525298099629866 ) ) ;
#14162 = DIRECTION ( 'NONE',  ( 0.000000000000000000, 0.000000000000000000, -1.000000000000000000 ) ) ;
#14163 = EDGE_CURVE ( 'NONE', #4559, #5569, #22984, .T. ) ;
#14164 = CARTESIAN_POINT ( 'NONE',  ( 21.09992658989239089, 28.21664230456639899, 47.04930799450051637 ) ) ;
#14165 = DIRECTION ( 'NONE',  ( 0.000000000000000000, 0.000000000000000000, 1.000000000000000000 ) ) ;
#14166 = EDGE_CURVE ( 'NONE', #32191, #13009, #24633, .T. ) ;
#14167 = CIRCLE ( 'NONE', #27254, 25.50000000000000355 ) ;
#14168 = EDGE_CURVE ( 'NONE', #3389, #22214, #20962, .T. ) ;
#14169 = CARTESIAN_POINT ( 'NONE',  ( 46.96819297411687444, 25.49253733014356271, 49.54594323136014822 ) ) ;
#14170 = EDGE_CURVE ( 'NONE', #11810, #231, #20433, .T. ) ;
#14171 = AXIS2_PLACEMENT_3D ( 'NONE', #11360, #1178, #31554 ) ;
#14172 =( LENGTH_UNIT ( ) NAMED_UNIT ( * ) SI_UNIT ( .MILLI., .METRE. ) );
#14173 = ORIENTED_EDGE ( 'NONE', *, *, #25092, .T. ) ;
#14174 = CARTESIAN_POINT ( 'NONE',  ( 46.48089935138444417, 23.09557481883486929, 46.64906498822688974 ) ) ;
#14175 = CARTESIAN_POINT ( 'NONE',  ( 45.84822719475717889, 25.05653309617948210, 44.59962885041953484 ) ) ;
#14176 = CARTESIAN_POINT ( 'NONE',  ( -41.02687597405218156, 7.220473278338834788, 53.54930799450051637 ) ) ;
#14177 = CARTESIAN_POINT ( 'NONE',  ( 47.09785597605719687, 15.77906836436399374, 47.04930799450078638 ) ) ;
#14178 = VERTEX_POINT ( 'NONE', #18534 ) ;
#14179 = DIRECTION ( 'NONE',  ( -1.101824276508909887E-16, 1.000000000000000000, -0.000000000000000000 ) ) ;
#14180 = CARTESIAN_POINT ( 'NONE',  ( 46.84209603737756566, 23.10527845304106620, 46.54793520446708044 ) ) ;
#14181 = DIRECTION ( 'NONE',  ( -1.000000000000000000, 0.000000000000000000, 0.000000000000000000 ) ) ;
#14182 = ORIENTED_EDGE ( 'NONE', *, *, #25212, .F. ) ;
#14183 = CARTESIAN_POINT ( 'NONE',  ( 47.91579473090698116, 29.86454579224779948, 48.65273438611181689 ) ) ;
#14184 = DIRECTION ( 'NONE',  ( -0.8746197071393810862, 0.4848096202463637039, 8.676864087101942305E-18 ) ) ;
#14185 = CIRCLE ( 'NONE', #17821, 55.85791022362053582 ) ;
#14186 = DIRECTION ( 'NONE',  ( -0.000000000000000000, 1.000000000000000000, -0.000000000000000000 ) ) ;
#14187 = DIRECTION ( 'NONE',  ( -1.101824276508909887E-16, 1.000000000000000000, -0.000000000000000000 ) ) ;
#14188 = EDGE_LOOP ( 'NONE', ( #14768, #1062, #22405, #8321 ) ) ;
#14189 = DIRECTION ( 'NONE',  ( 0.000000000000000000, -0.000000000000000000, -1.000000000000000000 ) ) ;
#14190 = ORIENTED_EDGE ( 'NONE', *, *, #32080, .F. ) ;
#14191 = AXIS2_PLACEMENT_3D ( 'NONE', #7557, #648, #7713 ) ;
#14192 = AXIS2_PLACEMENT_3D ( 'NONE', #26842, #9777, #19605 ) ;
#14193 = ORIENTED_EDGE ( 'NONE', *, *, #15938, .F. ) ;
#14194 = AXIS2_PLACEMENT_3D ( 'NONE', #26920, #12319, #4765 ) ;
#14195 = CIRCLE ( 'NONE', #27837, 12.36707279061065101 ) ;
#14196 = AXIS2_PLACEMENT_3D ( 'NONE', #2152, #9704, #1822 ) ;
#14197 = DIRECTION ( 'NONE',  ( 0.000000000000000000, 0.000000000000000000, -1.000000000000000000 ) ) ;
#14198 = EDGE_CURVE ( 'NONE', #27550, #15557, #29896, .T. ) ;
#14199 = ADVANCED_FACE ( 'NONE', ( #499 ), #22825, .F. ) ;
#14200 = DIRECTION ( 'NONE',  ( 0.000000000000000000, 1.000000000000000000, -0.000000000000000000 ) ) ;
#14201 = DIRECTION ( 'NONE',  ( 0.8907924160295465077, 1.100109261771873178E-16, -0.4544104659272754643 ) ) ;
#14202 = DIRECTION ( 'NONE',  ( 0.000000000000000000, -0.000000000000000000, -1.000000000000000000 ) ) ;
#14203 = AXIS2_PLACEMENT_3D ( 'NONE', #31964, #31485, #31803 ) ;
#14204 = ORIENTED_EDGE ( 'NONE', *, *, #16036, .T. ) ;
#14205 = FACE_OUTER_BOUND ( 'NONE', #17169, .T. ) ;
#14206 = ORIENTED_EDGE ( 'NONE', *, *, #28098, .F. ) ;
#14207 = FACE_OUTER_BOUND ( 'NONE', #18680, .T. ) ;
#14208 = DIRECTION ( 'NONE',  ( -0.000000000000000000, 1.000000000000000000, -0.000000000000000000 ) ) ;
#14209 = ADVANCED_FACE ( 'NONE', ( #17905 ), #19916, .T. ) ;
#14210 = DIRECTION ( 'NONE',  ( -0.000000000000000000, -1.000000000000000000, -0.000000000000000000 ) ) ;
#14211 = ORIENTED_EDGE ( 'NONE', *, *, #11045, .T. ) ;
#14212 = CARTESIAN_POINT ( 'NONE',  ( -42.66751614955960292, 15.14923148629343430, 38.44930799450052916 ) ) ;
#14213 = CARTESIAN_POINT ( 'NONE',  ( -40.57832940339291383, 7.446916344587776848, 53.80788663826320573 ) ) ;
#14214 = VERTEX_POINT ( 'NONE', #23151 ) ;
#14215 = DIRECTION ( 'NONE',  ( -0.000000000000000000, -1.000000000000000000, -0.000000000000000000 ) ) ;
#14216 = DIRECTION ( 'NONE',  ( -0.000000000000000000, -1.000000000000000000, -0.000000000000000000 ) ) ;
#14217 = DIRECTION ( 'NONE',  ( -1.000000000000000000, 0.000000000000000000, 0.000000000000000000 ) ) ;
#14218 = CARTESIAN_POINT ( 'NONE',  ( 43.09785597605720397, -5.098646251524523443, 47.04930799450052348 ) ) ;
#14219 = EDGE_LOOP ( 'NONE', ( #12708, #4671, #26368 ) ) ;
#14220 = VECTOR ( 'NONE', #13454, 1000.000000000000000 ) ;
#14221 = CARTESIAN_POINT ( 'NONE',  ( -40.06118906035626281, 6.942907937678607588, 34.99292058590180687 ) ) ;
#14222 = CARTESIAN_POINT ( 'NONE',  ( 48.14727188781975542, 19.96454579224779380, 49.10650501410607660 ) ) ;
#14223 = ORIENTED_EDGE ( 'NONE', *, *, #18640, .T. ) ;
#14224 = CARTESIAN_POINT ( 'NONE',  ( 45.41164638504195494, 22.93807716476589675, 46.96173444154113241 ) ) ;
#14225 = AXIS2_PLACEMENT_3D ( 'NONE', #32102, #29967, #15183 ) ;
#14226 = LINE ( 'NONE', #24224, #3282 ) ;
#14227 = ORIENTED_EDGE ( 'NONE', *, *, #22787, .F. ) ;
#14228 = EDGE_CURVE ( 'NONE', #5398, #12307, #5624, .T. ) ;
#14229 = ORIENTED_EDGE ( 'NONE', *, *, #31061, .F. ) ;
#14230 = CIRCLE ( 'NONE', #13712, 67.18681090792816235 ) ;
#14231 = EDGE_CURVE ( 'NONE', #28351, #10451, #25457, .T. ) ;
#14232 = ORIENTED_EDGE ( 'NONE', *, *, #16193, .T. ) ;
#14233 = EDGE_CURVE ( 'NONE', #1027, #30099, #518, .T. ) ;
#14234 = EDGE_CURVE ( 'NONE', #21709, #21280, #20524, .T. ) ;
#14235 = TOROIDAL_SURFACE ( 'NONE', #26292, 70.59901951359279337, 0.6000000000000020872 ) ;
#14236 = AXIS2_PLACEMENT_3D ( 'NONE', #23576, #5543, #3715 ) ;
#14237 = CARTESIAN_POINT ( 'NONE',  ( -41.73034863705382946, 11.48775164340967336, 56.04611646155296256 ) ) ;
#14238 = EDGE_LOOP ( 'NONE', ( #19993, #11960, #26546, #6270, #9300, #14259 ) ) ;
#14239 = LINE ( 'NONE', #11439, #1665 ) ;
#14240 = CARTESIAN_POINT ( 'NONE',  ( -43.73393778030726509, 1.305471833569777695, 53.64930799450051779 ) ) ;
#14241 = DIRECTION ( 'NONE',  ( -1.101824276508909887E-16, 1.000000000000000000, -0.000000000000000000 ) ) ;
#14242 = CARTESIAN_POINT ( 'NONE',  ( -40.50918210725697577, 7.581244431903962244, 53.87068005425620498 ) ) ;
#14243 = CARTESIAN_POINT ( 'NONE',  ( 45.81741271322955100, 26.44452976649965237, 49.02305402274571122 ) ) ;
#14244 = ADVANCED_FACE ( 'NONE', ( #18061 ), #28408, .F. ) ;
#14245 = VERTEX_POINT ( 'NONE', #13476 ) ;
#14246 = DIRECTION ( 'NONE',  ( 0.000000000000000000, 0.000000000000000000, -1.000000000000000000 ) ) ;
#14247 = ORIENTED_EDGE ( 'NONE', *, *, #8083, .T. ) ;
#14248 = CARTESIAN_POINT ( 'NONE',  ( -41.56848915456957627, 9.139695702668031885, 34.54930799450052348 ) ) ;
#14249 = TOROIDAL_SURFACE ( 'NONE', #27345, 58.88977237527051756, 0.9999999999999997780 ) ;
#14250 = ORIENTED_EDGE ( 'NONE', *, *, #16847, .F. ) ;
#14251 = CARTESIAN_POINT ( 'NONE',  ( 48.59475124299144966, 29.58954579224780090, 45.61232171765963272 ) ) ;
#14252 = DIRECTION ( 'NONE',  ( -1.224646799147353207E-16, -1.349345573449484691E-32, 1.000000000000000000 ) ) ;
#14253 = FACE_OUTER_BOUND ( 'NONE', #17070, .T. ) ;
#14254 = DIRECTION ( 'NONE',  ( 0.9612616959383200044, 0.2756373558169954996, -1.660411357259285896E-16 ) ) ;
#14255 = DIRECTION ( 'NONE',  ( 0.000000000000000000, 0.000000000000000000, -1.000000000000000000 ) ) ;
#14256 = CARTESIAN_POINT ( 'NONE',  ( 45.73035263060504718, 27.93954579807170546, 44.36855633853329550 ) ) ;
#14257 = CARTESIAN_POINT ( 'NONE',  ( 47.15639191806693020, 22.95310733321322161, 48.68846859551268835 ) ) ;
#14258 = CARTESIAN_POINT ( 'NONE',  ( 47.09785597605719687, 15.77906836436399374, 47.04930799450078638 ) ) ;
#14259 = ORIENTED_EDGE ( 'NONE', *, *, #23303, .T. ) ;
#14260 = DIRECTION ( 'NONE',  ( -1.000000000000000000, 0.000000000000000000, 0.000000000000000000 ) ) ;
#14261 = DIRECTION ( 'NONE',  ( -1.101824276508909887E-16, 1.000000000000000000, -0.000000000000000000 ) ) ;
#14262 = CARTESIAN_POINT ( 'NONE',  ( 8.732853799281729223, 26.97145308207318948, 47.04930799450051637 ) ) ;
#14263 = CIRCLE ( 'NONE', #1664, 45.99866570866061011 ) ;
#14264 = DIRECTION ( 'NONE',  ( -0.000000000000000000, -1.000000000000000000, 0.000000000000000000 ) ) ;
#14265 = CARTESIAN_POINT ( 'NONE',  ( -29.27337757263006424, -5.935454207752202116, 16.07118271501078866 ) ) ;
#14266 = AXIS2_PLACEMENT_3D ( 'NONE', #31954, #31789, #3893 ) ;
#14267 = VERTEX_POINT ( 'NONE', #3286 ) ;
#14268 = CARTESIAN_POINT ( 'NONE',  ( -43.86882709718853590, -0.1754741395363378920, 32.04930799450052348 ) ) ;
#14269 = CIRCLE ( 'NONE', #5363, 12.52641737965288904 ) ;
#14270 = EDGE_CURVE ( 'NONE', #25938, #25493, #23060, .T. ) ;
#14271 = ORIENTED_EDGE ( 'NONE', *, *, #31685, .F. ) ;
#14272 = DIRECTION ( 'NONE',  ( -1.224646799147353207E-16, 0.000000000000000000, -1.000000000000000000 ) ) ;
#14273 = CYLINDRICAL_SURFACE ( 'NONE', #21419, 43.50000000000000000 ) ;
#14274 = ADVANCED_FACE ( 'NONE', ( #10853, #11011 ), #20842, .F. ) ;
#14275 = ORIENTED_EDGE ( 'NONE', *, *, #6228, .F. ) ;
#14276 = EDGE_CURVE ( 'NONE', #30857, #6807, #16234, .T. ) ;
#14277 = EDGE_CURVE ( 'NONE', #21198, #2570, #30947, .T. ) ;
#14278 = ORIENTED_EDGE ( 'NONE', *, *, #23857, .F. ) ;
#14279 = CARTESIAN_POINT ( 'NONE',  ( 47.98162936688354563, 22.84434098701873239, 45.09251145694314289 ) ) ;
#14280 = DIRECTION ( 'NONE',  ( -1.101824276508909887E-16, 1.000000000000000000, -0.000000000000000000 ) ) ;
#14281 = DIRECTION ( 'NONE',  ( -1.000000000000000000, 0.000000000000000000, 0.000000000000000000 ) ) ;
#14282 = TOROIDAL_SURFACE ( 'NONE', #5898, 35.50000000000000711, 2.000000000000001776 ) ;
#14283 = VERTEX_POINT ( 'NONE', #16886 ) ;
#14284 = DIRECTION ( 'NONE',  ( -1.224646799147353207E-16, 0.000000000000000000, -1.000000000000000000 ) ) ;
#14285 = TOROIDAL_SURFACE ( 'NONE', #13242, 12.61792373059859607, 0.1249999999999979738 ) ;
#14286 = DIRECTION ( 'NONE',  ( 0.4848096202463424986, 0.8746197071393928546, -2.220446049250312834E-16 ) ) ;
#14287 = CARTESIAN_POINT ( 'NONE',  ( 76.46605017418944783, -2.833757427854269206, 13.30711217131973356 ) ) ;
#14288 = ORIENTED_EDGE ( 'NONE', *, *, #21993, .F. ) ;
#14289 = CARTESIAN_POINT ( 'NONE',  ( 21.09992658989238734, 38.56284415653841791, 47.04930799450051637 ) ) ;
#14290 = VERTEX_POINT ( 'NONE', #29370 ) ;
#14291 = CARTESIAN_POINT ( 'NONE',  ( 21.09992658989239089, 29.84164230456639899, 47.04930799450051637 ) ) ;
#14292 = CARTESIAN_POINT ( 'NONE',  ( -40.21210701746133509, 7.644196001419694575, 60.24930799450051211 ) ) ;
#14293 = DIRECTION ( 'NONE',  ( -1.000000000000000000, 0.000000000000000000, 0.000000000000000000 ) ) ;
#14294 = VERTEX_POINT ( 'NONE', #6398 ) ;
#14295 = ORIENTED_EDGE ( 'NONE', *, *, #2271, .T. ) ;
#14296 = CARTESIAN_POINT ( 'NONE',  ( 74.06012918148380209, -13.30632128221581212, 29.06553281253166432 ) ) ;
#14297 = CARTESIAN_POINT ( 'NONE',  ( 33.37634396954520355, 30.59164230456639544, 47.04930799450051637 ) ) ;
#14298 = FACE_OUTER_BOUND ( 'NONE', #24447, .T. ) ;
#14299 = TOROIDAL_SURFACE ( 'NONE', #9043, 12.61792373059895844, 0.1249999999999980571 ) ;
#14300 = ORIENTED_EDGE ( 'NONE', *, *, #31498, .T. ) ;
#14301 = CARTESIAN_POINT ( 'NONE',  ( -11.70362862524498304, -5.043292969097927347, -10.29680806063067067 ) ) ;
#14302 = DIRECTION ( 'NONE',  ( 0.3958453973320081309, 0.7141240004913237405, 0.5773502691896250649 ) ) ;
#14303 = CIRCLE ( 'NONE', #144, 27.49999999999998934 ) ;
#14304 = ADVANCED_FACE ( 'NONE', ( #21648 ), #2090, .T. ) ;
#14305 = VERTEX_POINT ( 'NONE', #19343 ) ;
#14306 = CARTESIAN_POINT ( 'NONE',  ( -11.40214402394279603, 13.86454579224779948, 47.04930799450052348 ) ) ;
#14307 = CARTESIAN_POINT ( 'NONE',  ( 48.73570333863616355, 25.72287913140504756, 44.52463952959527660 ) ) ;
#14308 = DIRECTION ( 'NONE',  ( 0.000000000000000000, 0.000000000000000000, -1.000000000000000000 ) ) ;
#14309 = AXIS2_PLACEMENT_3D ( 'NONE', #7977, #17968, #10113 ) ;
#14310 = ADVANCED_FACE ( 'NONE', ( #19178 ), #3939, .T. ) ;
#14311 = ORIENTED_EDGE ( 'NONE', *, *, #1026, .F. ) ;
#14312 = EDGE_CURVE ( 'NONE', #7978, #1764, #13958, .T. ) ;
#14313 = LINE ( 'NONE', #11689, #30275 ) ;
#14314 = CARTESIAN_POINT ( 'NONE',  ( 21.09785597605720042, -16.03545420775220265, -23.54971151909227700 ) ) ;
#14315 = CARTESIAN_POINT ( 'NONE',  ( 33.50134396954520355, 30.59164230456639544, 47.04930799450051637 ) ) ;
#14316 = CARTESIAN_POINT ( 'NONE',  ( 49.44739180854976013, 25.97786309983299091, 47.17133137409169308 ) ) ;
#14317 = ORIENTED_EDGE ( 'NONE', *, *, #6405, .T. ) ;
#14318 = AXIS2_PLACEMENT_3D ( 'NONE', #22315, #32339, #19848 ) ;
#14319 = DIRECTION ( 'NONE',  ( -0.000000000000000000, -1.000000000000000000, -0.000000000000000000 ) ) ;
#14321 = LINE ( 'NONE', #1998, #10400 ) ;
#14320 = CIRCLE ( 'NONE', #32156, 12.48414152717711900 ) ;
#14322 = CARTESIAN_POINT ( 'NONE',  ( 51.00445379728992634, 6.094407115496624172, -3.914104645325461540 ) ) ;
#14323 = DIRECTION ( 'NONE',  ( 0.000000000000000000, 0.000000000000000000, -1.000000000000000000 ) ) ;
#14324 = DIRECTION ( 'NONE',  ( -0.4848096202463655358, -0.8746197071393799760, 0.000000000000000000 ) ) ;
#14325 = CARTESIAN_POINT ( 'NONE',  ( -39.44363481821952178, 3.888719912690143499, 37.04930799450052348 ) ) ;
#14326 = DIRECTION ( 'NONE',  ( 1.000000000000000000, 0.000000000000000000, 0.000000000000000000 ) ) ;
#14327 = AXIS2_PLACEMENT_3D ( 'NONE', #31261, #28317, #21069 ) ;
#14328 = AXIS2_PLACEMENT_3D ( 'NONE', #16059, #26064, #8684 ) ;
#14329 = PRODUCT_RELATED_PRODUCT_CATEGORY ( 'part', '', ( #9564 ) ) ;
#14330 = FILL_AREA_STYLE ('',( #7593 ) ) ;
#14331 =( LENGTH_UNIT ( ) NAMED_UNIT ( * ) SI_UNIT ( .MILLI., .METRE. ) );
#14332 = VERTEX_POINT ( 'NONE', #23637 ) ;
#14333 = CARTESIAN_POINT ( 'NONE',  ( 45.80520143376154607, 22.95310733321322161, 46.03969511487858313 ) ) ;
#14334 = FACE_OUTER_BOUND ( 'NONE', #15152, .T. ) ;
#14335 = FACE_OUTER_BOUND ( 'NONE', #139, .T. ) ;
#14336 = FACE_OUTER_BOUND ( 'NONE', #7025, .T. ) ;
#14337 = VERTEX_POINT ( 'NONE', #31827 ) ;
#14338 = CARTESIAN_POINT ( 'NONE',  ( -39.57293394879278026, -5.936033350080357707, 77.90897538353701179 ) ) ;
#14339 = DIRECTION ( 'NONE',  ( -0.9612616959383221138, -0.2756373558169876170, 0.000000000000000000 ) ) ;
#14340 = FACE_OUTER_BOUND ( 'NONE', #20133, .T. ) ;
#14341 = VERTEX_POINT ( 'NONE', #29207 ) ;
#14342 = EDGE_LOOP ( 'NONE', ( #8710, #2241, #17183, #27147 ) ) ;
#14343 = CARTESIAN_POINT ( 'NONE',  ( 21.09785597605720753, 14.86454579224779948, 47.04930799450052348 ) ) ;
#14344 = DIRECTION ( 'NONE',  ( -1.000000000000000000, 0.000000000000000000, 0.000000000000000000 ) ) ;
#14345 = SPHERICAL_SURFACE ( 'NONE', #9951, 0.1000000000000000056 ) ;
#14346 = FACE_OUTER_BOUND ( 'NONE', #27298, .T. ) ;
#14347 = VECTOR ( 'NONE', #12444, 1000.000000000000000 ) ;
#14348 = ORIENTED_EDGE ( 'NONE', *, *, #12460, .T. ) ;
#14349 = CARTESIAN_POINT ( 'NONE',  ( 21.09785597605719332, 15.56454579224779877, 47.04930799450051637 ) ) ;
#14350 = ORIENTED_EDGE ( 'NONE', *, *, #3799, .F. ) ;
#14351 = ADVANCED_FACE ( 'NONE', ( #11816 ), #18856, .F. ) ;
#14352 = EDGE_LOOP ( 'NONE', ( #19500, #32151, #29005 ) ) ;
#14353 = CIRCLE ( 'NONE', #19587, 55.00000000000000000 ) ;
#14354 = EDGE_CURVE ( 'NONE', #19168, #17364, #29045, .T. ) ;
#14355 = ADVANCED_FACE ( 'NONE', ( #11173 ), #23595, .F. ) ;
#14356 = ADVANCED_FACE ( 'NONE', ( #9346 ), #21156, .F. ) ;
#14357 = CIRCLE ( 'NONE', #20631, 22.00000000000000000 ) ;
#14358 = AXIS2_PLACEMENT_3D ( 'NONE', #17678, #27866, #5217 ) ;
#14359 = EDGE_CURVE ( 'NONE', #23536, #19744, #26260, .T. ) ;
#14360 = CARTESIAN_POINT ( 'NONE',  ( 21.09785597605719332, 30.56454579224779522, 79.54930799450052348 ) ) ;
#14361 = DIRECTION ( 'NONE',  ( -1.101824276508909887E-16, 1.000000000000000000, -0.000000000000000000 ) ) ;
#14362 = DIRECTION ( 'NONE',  ( 0.000000000000000000, -1.000000000000000000, 0.000000000000000000 ) ) ;
#14363 = DIRECTION ( 'NONE',  ( -1.101824276508909887E-16, 1.000000000000000000, -0.000000000000000000 ) ) ;
#14364 = EDGE_LOOP ( 'NONE', ( #10271, #2960, #28672, #29435, #15347, #16657, #6669, #10232, #2823, #13799, #310, #24391 ) ) ;
#14365 = CARTESIAN_POINT ( 'NONE',  ( -9.880269303432738681, -5.935454207752202116, -13.48461434800281289 ) ) ;
#14366 = ORIENTED_EDGE ( 'NONE', *, *, #28074, .T. ) ;
#14367 = DIRECTION ( 'NONE',  ( -1.000000000000000000, -1.101824276508909887E-16, 0.000000000000000000 ) ) ;
#14368 = DIRECTION ( 'NONE',  ( -0.000000000000000000, -1.000000000000000000, 0.000000000000000000 ) ) ;
#14369 = CARTESIAN_POINT ( 'NONE',  ( -40.64500813507293486, 6.819128862114092193, 39.51928662074344345 ) ) ;
#14370 = ORIENTED_EDGE ( 'NONE', *, *, #11216, .T. ) ;
#14371 = FACE_BOUND ( 'NONE', #15996, .T. ) ;
#14372 = CARTESIAN_POINT ( 'NONE',  ( 21.09992658989238734, 30.71664230456641675, 47.04930799450051637 ) ) ;
#14373 = FACE_OUTER_BOUND ( 'NONE', #16626, .T. ) ;
#14374 = CARTESIAN_POINT ( 'NONE',  ( -38.05567176388107242, 15.54312433976834740, 59.54930799450050927 ) ) ;
#14375 = CARTESIAN_POINT ( 'NONE',  ( 21.09785597605719332, -15.93545420775219945, 123.7593585008393831 ) ) ;
#14376 = DIRECTION ( 'NONE',  ( -1.224646799147353207E-16, -1.349345573449484691E-32, 1.000000000000000000 ) ) ;
#14377 = ORIENTED_EDGE ( 'NONE', *, *, #6229, .T. ) ;
#14378 = DIRECTION ( 'NONE',  ( -1.000000000000000000, 0.000000000000000000, 0.000000000000000000 ) ) ;
#14379 = DIRECTION ( 'NONE',  ( 1.000000000000000000, 0.000000000000000000, 0.000000000000000000 ) ) ;
#14380 = ORIENTED_EDGE ( 'NONE', *, *, #2358, .F. ) ;
#14382 = EDGE_CURVE ( 'NONE', #23429, #4508, #31518, .T. ) ;
#14381 = DIRECTION ( 'NONE',  ( -1.101824276508909887E-16, 1.000000000000000000, -0.000000000000000000 ) ) ;
#14383 = FACE_OUTER_BOUND ( 'NONE', #5558, .T. ) ;
#14384 = ORIENTED_EDGE ( 'NONE', *, *, #17453, .F. ) ;
#14385 = ORIENTED_EDGE ( 'NONE', *, *, #6410, .F. ) ;
#14386 = UNCERTAINTY_MEASURE_WITH_UNIT (LENGTH_MEASURE( 1.000000000000000082E-05 ), #27772, 'distance_accuracy_value', 'NONE');
#14387 = ORIENTED_EDGE ( 'NONE', *, *, #11861, .T. ) ;
#14388 = EDGE_CURVE ( 'NONE', #18298, #30931, #4720, .T. ) ;
#14389 = CIRCLE ( 'NONE', #10198, 1.003191532947550701 ) ;
#14390 = EDGE_CURVE ( 'NONE', #15932, #15162, #21496, .T. ) ;
#14391 = CIRCLE ( 'NONE', #18057, 24.99999999999999645 ) ;
#14392 = ADVANCED_FACE ( 'NONE', ( #26744 ), #16559, .T. ) ;
#14393 = TOROIDAL_SURFACE ( 'NONE', #753, 0.2000000000000000111, 0.1000000000000000056 ) ;
#14394 = CIRCLE ( 'NONE', #21729, 12.62506659569710266 ) ;
#14395 = DIRECTION ( 'NONE',  ( -1.101824276508909887E-16, 1.000000000000000000, -0.000000000000000000 ) ) ;
#14396 = B_SPLINE_CURVE_WITH_KNOTS ( 'NONE', 3,
 ( #5732, #10674, #12966, #13451, #28059, #25907, #20978, #12807, #23290, #23446, #803, #18186 ),
 .UNSPECIFIED., .F., .F.,
 ( 4, 2, 2, 2, 2, 4 ),
 ( 0.0003422370341462309374, 0.002080102550335785096, 0.003817968066525339200, 0.005555833582714892437, 0.006424766340809669705, 0.007293699098904446974 ),
 .UNSPECIFIED. ) ;
#14397 = ORIENTED_EDGE ( 'NONE', *, *, #28675, .F. ) ;
#14398 = VERTEX_POINT ( 'NONE', #11655 ) ;
#14399 = DIRECTION ( 'NONE',  ( -1.101824276508909887E-16, 1.000000000000000000, -0.000000000000000000 ) ) ;
#14400 = CARTESIAN_POINT ( 'NONE',  ( 47.40417757965286683, 23.10527845304106620, 46.57712699531703038 ) ) ;
#14401 = DIRECTION ( 'NONE',  ( -0.4544104193609807552, 0.000000000000000000, -0.8907924397839137587 ) ) ;
#14402 = CARTESIAN_POINT ( 'NONE',  ( 45.38854177497844944, 27.66952976649964668, 45.94041160078741370 ) ) ;
#14403 = ORIENTED_EDGE ( 'NONE', *, *, #21357, .F. ) ;
#14404 = DIRECTION ( 'NONE',  ( -1.000000000000000000, 0.000000000000000000, 0.000000000000000000 ) ) ;
#14405 = ORIENTED_EDGE ( 'NONE', *, *, #31431, .F. ) ;
#14406 = CARTESIAN_POINT ( 'NONE',  ( 48.14727188781972700, 22.86454579224779948, 49.10650501410609081 ) ) ;
#14407 = ORIENTED_EDGE ( 'NONE', *, *, #5496, .F. ) ;
#14409 = EDGE_CURVE ( 'NONE', #28894, #24681, #16259, .T. ) ;
#14408 = DIRECTION ( 'NONE',  ( -1.101824276508909887E-16, 1.000000000000000000, -0.000000000000000000 ) ) ;
#14410 = DIRECTION ( 'NONE',  ( -0.000000000000000000, 1.000000000000000000, -0.000000000000000000 ) ) ;
#14411 = LINE ( 'NONE', #24412, #27256 ) ;
#14412 = DIRECTION ( 'NONE',  ( -1.224646799147353207E-16, 0.000000000000000000, -1.000000000000000000 ) ) ;
#14413 = CARTESIAN_POINT ( 'NONE',  ( 47.23302798462060537, 26.48121246473837687, 44.44659793406428605 ) ) ;
#14414 = AXIS2_PLACEMENT_3D ( 'NONE', #19674, #9838, #5076 ) ;
#14415 = CARTESIAN_POINT ( 'NONE',  ( -40.02540636251514172, 2.839176264122877047, 57.04930799450051637 ) ) ;
#14416 = DIRECTION ( 'NONE',  ( -1.313185983435984691E-29, 1.000000000000000000, 3.761114140369702165E-15 ) ) ;
#14417 = CIRCLE ( 'NONE', #1300, 0.9999999999999731326 ) ;
#14418 = ORIENTED_EDGE ( 'NONE', *, *, #31143, .T. ) ;
#14419 = DIRECTION ( 'NONE',  ( -1.101824276508909887E-16, 1.000000000000000000, -0.000000000000000000 ) ) ;
#14421 = EDGE_CURVE ( 'NONE', #25267, #257, #11969, .T. ) ;
#14420 = FACE_OUTER_BOUND ( 'NONE', #11982, .T. ) ;
#14422 = AXIS2_PLACEMENT_3D ( 'NONE', #7510, #7671, #7997 ) ;
#14423 = CARTESIAN_POINT ( 'NONE',  ( -40.61178118339597631, 9.038025460530262123, 56.14611646155296398 ) ) ;
#14424 = EDGE_CURVE ( 'NONE', #7900, #10115, #542, .T. ) ;
#14425 = VECTOR ( 'NONE', #23144, 1000.000000000000000 ) ;
#14426 = CIRCLE ( 'NONE', #4988, 36.01080762834750715 ) ;
#14427 = CARTESIAN_POINT ( 'NONE',  ( 48.81767175631193112, 22.89977464660286444, 46.33034145269077442 ) ) ;
#14428 = CARTESIAN_POINT ( 'NONE',  ( 45.96182992765472619, 28.00087065737811898, 44.82232689504102296 ) ) ;
#14429 = ORIENTED_EDGE ( 'NONE', *, *, #2486, .T. ) ;
#14430 = ORIENTED_EDGE ( 'NONE', *, *, #18409, .T. ) ;
#14431 = DIRECTION ( 'NONE',  ( -1.101824276508909887E-16, 1.000000000000000000, -0.000000000000000000 ) ) ;
#14432 = CARTESIAN_POINT ( 'NONE',  ( 21.09992658989239089, 27.71664230456639899, 47.04930799450051637 ) ) ;
#14433 = B_SPLINE_CURVE_WITH_KNOTS ( 'NONE', 3,
 ( #6329, #16331, #13888, #23887, #1398, #11412 ),
 .UNSPECIFIED., .F., .F.,
 ( 4, 2, 4 ),
 ( 0.000000000000000000, 0.5000000000000000000, 1.000000000000000000 ),
 .UNSPECIFIED. ) ;
#14434 = EDGE_LOOP ( 'NONE', ( #14931, #24394, #16954, #22380 ) ) ;
#14435 = ADVANCED_FACE ( 'NONE', ( #7987 ), #28846, .F. ) ;
#14436 = VECTOR ( 'NONE', #12145, 999.9999999999998863 ) ;
#14437 = EDGE_LOOP ( 'NONE', ( #1952, #27079, #26574, #15664 ) ) ;
#14438 = AXIS2_PLACEMENT_3D ( 'NONE', #4588, #1964, #22144 ) ;
#14439 = CARTESIAN_POINT ( 'NONE',  ( -39.31817303416426768, 4.733858564475560193, 37.04930799450052348 ) ) ;
#14440 = CARTESIAN_POINT ( 'NONE',  ( 51.96080742951041742, -5.936631694656545832, -13.43417697512268916 ) ) ;
#14442 = DIRECTION ( 'NONE',  ( -0.000000000000000000, -0.000000000000000000, 1.000000000000000000 ) ) ;
#14441 = AXIS2_PLACEMENT_3D ( 'NONE', #26020, #15862, #25710 ) ;
#14443 = AXIS2_PLACEMENT_3D ( 'NONE', #14819, #13729, #2338 ) ;
#14444 = CIRCLE ( 'NONE', #30689, 66.44011198581388555 ) ;
#14445 = VERTEX_POINT ( 'NONE', #24599 ) ;
#14446 = DIRECTION ( 'NONE',  ( -1.000000000000000000, 0.000000000000000000, 0.000000000000000000 ) ) ;
#14447 = CARTESIAN_POINT ( 'NONE',  ( 21.09785597605718976, 7.094379510609982731, 66.36907787364950195 ) ) ;
#14448 = CARTESIAN_POINT ( 'NONE',  ( 76.70546203173246624, -3.171899563477270867, 13.33972164219158607 ) ) ;
#14449 = EDGE_CURVE ( 'NONE', #22635, #22128, #20607, .T. ) ;
#14450 = ORIENTED_EDGE ( 'NONE', *, *, #20038, .T. ) ;
#14451 = ORIENTED_EDGE ( 'NONE', *, *, #3108, .F. ) ;
#14452 = CYLINDRICAL_SURFACE ( 'NONE', #3908, 10.00000000000000533 ) ;
#14453 = ORIENTED_EDGE ( 'NONE', *, *, #13628, .T. ) ;
#14454 = EDGE_CURVE ( 'NONE', #22782, #4744, #12085, .T. ) ;
#14455 = CARTESIAN_POINT ( 'NONE',  ( -40.64160980462626327, 6.824069488939677797, 34.67994969264233163 ) ) ;
#14456 = DIRECTION ( 'NONE',  ( 0.000000000000000000, 1.000000000000000000, 0.000000000000000000 ) ) ;
#14457 = DIRECTION ( 'NONE',  ( 0.9612616959383207815, 0.2756373558169927240, 8.795445018804291370E-19 ) ) ;
#14458 = DIRECTION ( 'NONE',  ( 0.000000000000000000, 0.000000000000000000, 1.000000000000000000 ) ) ;
#14459 = ORIENTED_EDGE ( 'NONE', *, *, #21922, .F. ) ;
#14460 = VERTEX_POINT ( 'NONE', #5364 ) ;
#14461 = CARTESIAN_POINT ( 'NONE',  ( 49.06850489496601142, -13.30632128221581034, -1.386849490760364789 ) ) ;
#14462 = ADVANCED_FACE ( 'NONE', ( #27672 ), #2112, .T. ) ;
#14463 = DIRECTION ( 'NONE',  ( 0.2756373558170018279, -0.9612616959383181170, 0.000000000000000000 ) ) ;
#14464 = EDGE_CURVE ( 'NONE', #8721, #29191, #15522, .T. ) ;
#14465 = EDGE_CURVE ( 'NONE', #22386, #22091, #2882, .T. ) ;
#14466 = ORIENTED_EDGE ( 'NONE', *, *, #18227, .T. ) ;
#14467 = CARTESIAN_POINT ( 'NONE',  ( -8.414270849481495063, 6.668192824305379851, -4.699568316320720918 ) ) ;
#14468 = LINE ( 'NONE', #24792, #13 ) ;
#14469 = ORIENTED_EDGE ( 'NONE', *, *, #13580, .F. ) ;
#14470 = DIRECTION ( 'NONE',  ( -0.4848096202463673121, -0.8746197071393789768, 0.000000000000000000 ) ) ;
#14471 = FACE_OUTER_BOUND ( 'NONE', #28737, .T. ) ;
#14472 = AXIS2_PLACEMENT_3D ( 'NONE', #12852, #17921, #30406 ) ;
#14473 = STYLED_ITEM ( 'NONE', ( #28298 ), #26470 ) ;
#14474 = CARTESIAN_POINT ( 'NONE',  ( 21.09992658989238734, 38.56284415653841791, 47.04930799450051637 ) ) ;
#14475 = EDGE_CURVE ( 'NONE', #15078, #13441, #24651, .T. ) ;
#14476 = CIRCLE ( 'NONE', #22826, 12.62506659569710266 ) ;
#14477 = EDGE_LOOP ( 'NONE', ( #21349, #18113, #77, #9555, #26898, #615, #30788 ) ) ;
#14478 = FACE_OUTER_BOUND ( 'NONE', #10355, .T. ) ;
#14479 = FACE_OUTER_BOUND ( 'NONE', #1648, .T. ) ;
#14480 = DIRECTION ( 'NONE',  ( -0.1949050434465282311, 0.6797146636928673713, -0.7071067811865470176 ) ) ;
#14481 = CARTESIAN_POINT ( 'NONE',  ( 48.91284552371730143, 26.03619643316632448, 46.12344667017377020 ) ) ;
#14482 = ORIENTED_EDGE ( 'NONE', *, *, #8992, .F. ) ;
#14483 = CARTESIAN_POINT ( 'NONE',  ( -40.11286833322907341, 2.887657226147507306, 37.04930799450052348 ) ) ;
#14484 = CARTESIAN_POINT ( 'NONE',  ( -43.37834615508418068, 1.121909970995876193, 34.64930799450052490 ) ) ;
#14485 = ADVANCED_FACE ( 'NONE', ( #19508 ), #29540, .T. ) ;
#14486 = AXIS2_PLACEMENT_3D ( 'NONE', #30732, #1159, #28583 ) ;
#14487 = CARTESIAN_POINT ( 'NONE',  ( 48.14616182813506384, 9.421471677506305653, -3.404495637954462417 ) ) ;
#14488 = AXIS2_PLACEMENT_3D ( 'NONE', #13971, #24619, #31533 ) ;
#14489 = EDGE_CURVE ( 'NONE', #306, #9336, #30474, .T. ) ;
#14490 = CARTESIAN_POINT ( 'NONE',  ( 48.14727188781975542, 22.86454579224779948, 49.10650501410607660 ) ) ;
#14491 = DIRECTION ( 'NONE',  ( -0.000000000000000000, -1.000000000000000000, -0.000000000000000000 ) ) ;
#14492 = CARTESIAN_POINT ( 'NONE',  ( -6.402144023942787143, -5.098646251524523443, 47.04930799450052348 ) ) ;
#14493 = FACE_OUTER_BOUND ( 'NONE', #1897, .T. ) ;
#14494 = DIRECTION ( 'NONE',  ( -0.000000000000000000, -1.000000000000000000, -0.000000000000000000 ) ) ;
#14495 = EDGE_LOOP ( 'NONE', ( #5367, #27976, #20306, #31148 ) ) ;
#14496 = CARTESIAN_POINT ( 'NONE',  ( 45.95383497628772318, 23.03451764446790051, 46.65777585308548225 ) ) ;
#14497 = CARTESIAN_POINT ( 'NONE',  ( 48.51627339957213536, 25.02287913140503761, 44.86288096775929546 ) ) ;
#14498 = ADVANCED_FACE ( 'NONE', ( #7043 ), #17048, .T. ) ;
#14499 = CARTESIAN_POINT ( 'NONE',  ( -29.36860851563585584, 8.903991466124205445, 19.42204177740639892 ) ) ;
#14500 = VECTOR ( 'NONE', #1715, 1000.000000000000114 ) ;
#14501 = CARTESIAN_POINT ( 'NONE',  ( -41.02687597405218156, 7.220473278338834788, 53.64930799450051779 ) ) ;
#14502 = ORIENTED_EDGE ( 'NONE', *, *, #19556, .T. ) ;
#14503 = DIRECTION ( 'NONE',  ( -1.101824276508909887E-16, 1.000000000000000000, -0.000000000000000000 ) ) ;
#14504 = CARTESIAN_POINT ( 'NONE',  ( -40.11967773290336226, 9.763195579837789850, 38.54930799450052348 ) ) ;
#14505 = CARTESIAN_POINT ( 'NONE',  ( 21.09785597605720753, -5.098646251524523443, 47.04930799450052348 ) ) ;
#14506 = ORIENTED_EDGE ( 'NONE', *, *, #9794, .F. ) ;
#14507 = VERTEX_POINT ( 'NONE', #17653 ) ;
#14508 = FACE_OUTER_BOUND ( 'NONE', #21913, .T. ) ;
#14509 = DIRECTION ( 'NONE',  ( -1.224646799147353207E-16, -1.349345573449484691E-32, 1.000000000000000000 ) ) ;
#14510 = DIRECTION ( 'NONE',  ( -0.4848096202463429427, -0.8746197071393925215, 2.352477780477436787E-16 ) ) ;
#14511 = CARTESIAN_POINT ( 'NONE',  ( 40.59785597605721108, -5.098646251524523443, 47.04930799450052348 ) ) ;
#14512 = ORIENTED_EDGE ( 'NONE', *, *, #29495, .T. ) ;
#14513 = DIRECTION ( 'NONE',  ( 0.000000000000000000, -1.000000000000000000, 0.000000000000000000 ) ) ;
#14514 = ORIENTED_EDGE ( 'NONE', *, *, #19061, .F. ) ;
#14515 = AXIS2_PLACEMENT_3D ( 'NONE', #7560, #12818, #29559 ) ;
#14516 = EDGE_LOOP ( 'NONE', ( #23878, #17432, #9271, #17577 ) ) ;
#14517 = FACE_OUTER_BOUND ( 'NONE', #7810, .T. ) ;
#14518 = CIRCLE ( 'NONE', #20795, 12.36707279061065279 ) ;
#14519 = ORIENTED_EDGE ( 'NONE', *, *, #15526, .F. ) ;
#14520 = CARTESIAN_POINT ( 'NONE',  ( 33.72499318558949000, 38.56284415653841791, 47.04930799450051637 ) ) ;
#14521 = CARTESIAN_POINT ( 'NONE',  ( -29.47038852791792962, 8.010743491677633443, 75.51333467491832607 ) ) ;
#14522 = DIRECTION ( 'NONE',  ( -0.8746197071393790878, 0.4848096202463673676, 1.277302113040196197E-17 ) ) ;
#14523 = VERTEX_POINT ( 'NONE', #264 ) ;
#14524 = CARTESIAN_POINT ( 'NONE',  ( 51.92400919103563695, -5.935454207752202116, -13.65255231306078798 ) ) ;
#14525 = ORIENTED_EDGE ( 'NONE', *, *, #4346, .T. ) ;
#14526 = DIRECTION ( 'NONE',  ( -1.101824276508909887E-16, 1.000000000000000000, -0.000000000000000000 ) ) ;
#14527 = FACE_OUTER_BOUND ( 'NONE', #29861, .T. ) ;
#14528 = PLANE ( 'NONE',  #20718 ) ;
#14529 = ORIENTED_EDGE ( 'NONE', *, *, #27674, .F. ) ;
#14530 = CARTESIAN_POINT ( 'NONE',  ( -43.82034613516389498, -0.08801216882239806805, 62.04930799450052348 ) ) ;
#14531 = DIRECTION ( 'NONE',  ( 0.000000000000000000, 0.000000000000000000, -1.000000000000000000 ) ) ;
#14533 = DIRECTION ( 'NONE',  ( 1.188208965918165239E-16, 1.880121038077813132E-16, 1.000000000000000000 ) ) ;
#14532 = CIRCLE ( 'NONE', #7198, 54.30000000000000426 ) ;
#14534 = DIRECTION ( 'NONE',  ( 0.000000000000000000, -0.000000000000000000, -1.000000000000000000 ) ) ;
#14535 = EDGE_CURVE ( 'NONE', #1830, #25211, #101, .T. ) ;
#14536 = FACE_OUTER_BOUND ( 'NONE', #131, .T. ) ;
#14537 = CARTESIAN_POINT ( 'NONE',  ( 21.09785597605719332, 38.31023907818019580, 47.04930799450051637 ) ) ;
#14538 = CARTESIAN_POINT ( 'NONE',  ( -40.73091736380679606, 9.483895492497156354, 35.44930799450052206 ) ) ;
#14539 = ORIENTED_EDGE ( 'NONE', *, *, #7256, .T. ) ;
#14540 = CARTESIAN_POINT ( 'NONE',  ( -40.02327307428360115, 7.071123406434916880, 34.89423478111014276 ) ) ;
#14541 = CARTESIAN_POINT ( 'NONE',  ( 8.698509210239514289, 24.84164230456639544, 47.04930799450051637 ) ) ;
#14542 = ORIENTED_EDGE ( 'NONE', *, *, #3362, .T. ) ;
#14543 = DIRECTION ( 'NONE',  ( -1.101824276508909887E-16, 1.000000000000000000, -0.000000000000000000 ) ) ;
#14544 = CARTESIAN_POINT ( 'NONE',  ( 40.59785597605721108, 14.86454579224779948, 47.04930799450052348 ) ) ;
#14545 = ORIENTED_EDGE ( 'NONE', *, *, #23861, .T. ) ;
#14546 = PRODUCT ( 'Terminals', 'Terminals', '', ( #12486 ) ) ;
#14547 =( BOUNDED_CURVE ( )  B_SPLINE_CURVE ( 3, ( #9646, #14567, #24571, #4718 ),
 .UNSPECIFIED., .F., .F. ) 
 B_SPLINE_CURVE_WITH_KNOTS ( ( 4, 4 ),
 ( 5.497787143782102426, 6.283185307179586232 ),
 .UNSPECIFIED. ) 
 CURVE ( )  GEOMETRIC_REPRESENTATION_ITEM ( )  RATIONAL_B_SPLINE_CURVE ( ( 1.000000000000000000, 0.9492530216741865701, 0.9492530216741865701, 1.000000000000000000 ) ) 
 REPRESENTATION_ITEM ( '' )  );
#14548 = EDGE_LOOP ( 'NONE', ( #30499, #22704, #7629, #31981, #14103, #8647 ) ) ;
#14549 = AXIS2_PLACEMENT_3D ( 'NONE', #15451, #20361, #10368 ) ;
#14550 = ORIENTED_EDGE ( 'NONE', *, *, #15279, .F. ) ;
#14551 = CONICAL_SURFACE ( 'NONE', #394, 19.45967690998103805, 0.7960495370845414032 ) ;
#14552 = AXIS2_PLACEMENT_3D ( 'NONE', #24833, #21701, #1852 ) ;
#14553 = DIRECTION ( 'NONE',  ( -0.4848096202463431648, -0.8746197071393924105, 0.000000000000000000 ) ) ;
#14554 = ORIENTED_EDGE ( 'NONE', *, *, #31790, .F. ) ;
#14555 = AXIS2_PLACEMENT_3D ( 'NONE', #18296, #23550, #20922 ) ;
#14556 = VERTEX_POINT ( 'NONE', #27841 ) ;
#14557 = CYLINDRICAL_SURFACE ( 'NONE', #15075, 54.30000000000000426 ) ;
#14558 = DIRECTION ( 'NONE',  ( 0.000000000000000000, -1.000000000000000000, 0.000000000000000000 ) ) ;
#14559 = CARTESIAN_POINT ( 'NONE',  ( 21.09785597605720753, 13.61454579224779771, 47.04930799450052348 ) ) ;
#14560 = DIRECTION ( 'NONE',  ( 0.4848096202463489934, 0.8746197071393893019, 9.920727850367968435E-18 ) ) ;
#14561 = DIRECTION ( 'NONE',  ( -1.000000000000000000, 0.000000000000000000, 0.000000000000000000 ) ) ;
#14562 = ORIENTED_EDGE ( 'NONE', *, *, #4038, .T. ) ;
#14563 = CARTESIAN_POINT ( 'NONE',  ( -8.565981920724627940, 6.453333540778367627, 97.92432209181883707 ) ) ;
#14564 = VERTEX_POINT ( 'NONE', #2886 ) ;
#14565 = CARTESIAN_POINT ( 'NONE',  ( -12.42032014790552807, -3.872051342217444070, -8.192007789466410728 ) ) ;
#14566 = EDGE_LOOP ( 'NONE', ( #17831, #3370 ) ) ;
#14567 = CARTESIAN_POINT ( 'NONE',  ( -40.67837904183829068, 9.488261090400161635, 34.65356819842892833 ) ) ;
#14568 = CARTESIAN_POINT ( 'NONE',  ( -40.11286833322908052, 2.887657226147511302, 57.04930799450051637 ) ) ;
#14569 = CARTESIAN_POINT ( 'NONE',  ( 21.09992658989239089, 26.97145308207318948, 47.04930799450051637 ) ) ;
#14570 = DIRECTION ( 'NONE',  ( -0.5932111027100930301, 0.7071067811865471286, -0.3848383915638822761 ) ) ;
#14571 = DIRECTION ( 'NONE',  ( -1.000000000000000000, 0.000000000000000000, 0.000000000000000000 ) ) ;
#14572 = EDGE_CURVE ( 'NONE', #12078, #15900, #2518, .T. ) ;
#14573 = ADVANCED_FACE ( 'NONE', ( #3524 ), #5999, .T. ) ;
#14574 = CARTESIAN_POINT ( 'NONE',  ( 50.10320668408830613, 26.30621246473837616, 47.20539118556276037 ) ) ;
#14575 = EDGE_CURVE ( 'NONE', #14642, #24034, #13872, .T. ) ;
#14576 = CARTESIAN_POINT ( 'NONE',  ( 47.35361591473682097, 23.10527845304106265, 47.55068078453451363 ) ) ;
#14577 = CARTESIAN_POINT ( 'NONE',  ( 21.09785597605720753, -5.098646251524523443, 47.04930799450052348 ) ) ;
#14578 = ADVANCED_FACE ( 'NONE', ( #13549 ), #28640, .T. ) ;
#14579 = EDGE_LOOP ( 'NONE', ( #14067, #13973, #28082 ) ) ;
#14580 = CARTESIAN_POINT ( 'NONE',  ( 47.13083292863866802, 29.59604743734263010, 44.98107144923852019 ) ) ;
#14581 = CARTESIAN_POINT ( 'NONE',  ( -40.12405407910454613, 7.699914440225940737, 60.22001867261916885 ) ) ;
#14582 = CARTESIAN_POINT ( 'NONE',  ( 47.09785597605719687, 15.77906836436399374, 47.04930799450078638 ) ) ;
#14583 = VECTOR ( 'NONE', #32446, 1000.000000000000000 ) ;
#14584 = FACE_OUTER_BOUND ( 'NONE', #20323, .T. ) ;
#14585 = CARTESIAN_POINT ( 'NONE',  ( -29.27337757263006424, -0.7885452029232787874, 13.38511290719907798 ) ) ;
#14586 = VERTEX_POINT ( 'NONE', #26010 ) ;
#14587 = AXIS2_PLACEMENT_3D ( 'NONE', #21136, #11632, #16540 ) ;
#14588 = ORIENTED_EDGE ( 'NONE', *, *, #10771, .T. ) ;
#14589 = CARTESIAN_POINT ( 'NONE',  ( 8.474859994195286461, 25.34184655352419213, 47.04930799450051637 ) ) ;
#14590 = CIRCLE ( 'NONE', #13538, 0.1250000000000001110 ) ;
#14591 = VERTEX_POINT ( 'NONE', #6153 ) ;
#14592 = ORIENTED_EDGE ( 'NONE', *, *, #18687, .T. ) ;
#14593 = DIRECTION ( 'NONE',  ( -1.000000000000000000, 0.000000000000000000, 0.000000000000000000 ) ) ;
#14594 = ADVANCED_FACE ( 'NONE', ( #31435 ), #19252, .T. ) ;
#14595 = CIRCLE ( 'NONE', #16664, 56.65825807113184709 ) ;
#14596 = LINE ( 'NONE', #22451, #16541 ) ;
#14597 = CARTESIAN_POINT ( 'NONE',  ( 21.09785597605719332, 25.13358275951983956, 47.04930799450051637 ) ) ;
#14598 = EDGE_CURVE ( 'NONE', #3624, #649, #19274, .T. ) ;
#14599 = AXIS2_PLACEMENT_3D ( 'NONE', #31355, #18215, #8861 ) ;
#14600 = AXIS2_PLACEMENT_3D ( 'NONE', #31341, #8531, #16070 ) ;
#14601 = ORIENTED_EDGE ( 'NONE', *, *, #25394, .T. ) ;
#14602 = VECTOR ( 'NONE', #6582, 1000.000000000000000 ) ;
#14603 = DIRECTION ( 'NONE',  ( -1.000000000000000000, 0.000000000000000000, 0.000000000000000000 ) ) ;
#14604 = AXIS2_PLACEMENT_3D ( 'NONE', #17145, #12249, #6989 ) ;
#14605 = DIRECTION ( 'NONE',  ( 0.2756373558169954441, -0.9612616959383198934, 1.479773560108263204E-16 ) ) ;
#14606 = DIRECTION ( 'NONE',  ( -1.101824276508909887E-16, 1.000000000000000000, -0.000000000000000000 ) ) ;
#14607 = ORIENTED_EDGE ( 'NONE', *, *, #1815, .T. ) ;
#14608 = VERTEX_POINT ( 'NONE', #749 ) ;
#14609 = LINE ( 'NONE', #4431, #16992 ) ;
#14610 = EDGE_LOOP ( 'NONE', ( #15893, #12217, #32246, #25062 ) ) ;
#14611 = CIRCLE ( 'NONE', #18272, 12.36707279061065101 ) ;
#14612 = DIRECTION ( 'NONE',  ( -1.224646799147353207E-16, -1.349345573449484691E-32, 1.000000000000000000 ) ) ;
#14613 = DIRECTION ( 'NONE',  ( 0.000000000000000000, -0.000000000000000000, -1.000000000000000000 ) ) ;
#14614 = DIRECTION ( 'NONE',  ( -1.224646799147353207E-16, -1.349345573449484691E-32, 1.000000000000000000 ) ) ;
#14615 = CARTESIAN_POINT ( 'NONE',  ( -45.73387052288833132, -5.935454207752206557, 40.15016479612525302 ) ) ;
#14616 = CARTESIAN_POINT ( 'NONE',  ( 44.70507715278255034, 28.36291119454914877, 46.92503878583765697 ) ) ;
#14617 = EDGE_CURVE ( 'NONE', #6215, #6567, #28711, .T. ) ;
#14618 = ORIENTED_EDGE ( 'NONE', *, *, #25398, .F. ) ;
#14619 = ORIENTED_EDGE ( 'NONE', *, *, #28988, .T. ) ;
#14620 = CARTESIAN_POINT ( 'NONE',  ( 67.63274615763145903, 14.86454579224779948, 47.04930799450051637 ) ) ;
#14621 = LINE ( 'NONE', #21986, #1521 ) ;
#14622 = ORIENTED_EDGE ( 'NONE', *, *, #7011, .T. ) ;
#14623 = CARTESIAN_POINT ( 'NONE',  ( -7.668010133714219023, 7.652955895019252885, -4.493996600949651032 ) ) ;
#14624 = CARTESIAN_POINT ( 'NONE',  ( 8.474859994195282908, 38.56284415653841791, 47.04930799450051637 ) ) ;
#14625 = ORIENTED_EDGE ( 'NONE', *, *, #30850, .F. ) ;
#14626 = CARTESIAN_POINT ( 'NONE',  ( 21.09785597605719332, -5.935454207752198563, 47.04930799450051637 ) ) ;
#14627 = DIRECTION ( 'NONE',  ( -1.101824276508909887E-16, 1.000000000000000000, -0.000000000000000000 ) ) ;
#14628 = AXIS2_PLACEMENT_3D ( 'NONE', #30675, #13756, #23281 ) ;
#14629 = AXIS2_PLACEMENT_3D ( 'NONE', #14349, #14513, #9752 ) ;
#14630 = DIRECTION ( 'NONE',  ( -1.101824276508909887E-16, 1.000000000000000000, -0.000000000000000000 ) ) ;
#14631 = AXIS2_PLACEMENT_3D ( 'NONE', #30050, #7561, #25116 ) ;
#14632 = EDGE_CURVE ( 'NONE', #22873, #7835, #7232, .T. ) ;
#14633 = EDGE_CURVE ( 'NONE', #12345, #29925, #12492, .T. ) ;
#14634 = CIRCLE ( 'NONE', #29865, 0.1000000000000006301 ) ;
#14635 = EDGE_LOOP ( 'NONE', ( #22033, #1818, #10510, #5529 ) ) ;
#14636 = ORIENTED_EDGE ( 'NONE', *, *, #2006, .F. ) ;
#14637 = DIRECTION ( 'NONE',  ( 0.8746197071393925215, -0.4848096202463429982, -8.676864087101708112E-18 ) ) ;
#14638 = ADVANCED_FACE ( 'NONE', ( #3365 ), #20312, .F. ) ;
#14639 = DIRECTION ( 'NONE',  ( 1.000000000000000000, 0.000000000000000000, 0.000000000000000000 ) ) ;
#14640 = CARTESIAN_POINT ( 'NONE',  ( 44.70507715278255745, 25.64951373492759856, 46.92503878583764987 ) ) ;
#14641 = ADVANCED_FACE ( 'NONE', ( #15681 ), #6171, .T. ) ;
#14642 = VERTEX_POINT ( 'NONE', #18771 ) ;
#14643 = EDGE_CURVE ( 'NONE', #11793, #17109, #23273, .T. ) ;
#14644 = DIRECTION ( 'NONE',  ( -0.000000000000000000, 1.000000000000000000, -0.000000000000000000 ) ) ;
#14645 = CARTESIAN_POINT ( 'NONE',  ( -40.58856461370174884, 7.499380836222963254, 60.14930799450051779 ) ) ;
#14646 = CARTESIAN_POINT ( 'NONE',  ( -40.09211399732166115, 9.667069410243957606, 35.44930799450052206 ) ) ;
#14647 = AXIS2_PLACEMENT_3D ( 'NONE', #2244, #12267, #20280 ) ;
#14648 = CIRCLE ( 'NONE', #32482, 0.2000000000000057288 ) ;
#14649 = DIRECTION ( 'NONE',  ( 1.234978253042719660E-16, -1.000000000000000000, -1.109335647967047851E-31 ) ) ;
#14650 = CARTESIAN_POINT ( 'NONE',  ( 33.72499318558949710, 23.84184655352419213, 47.04930799450051637 ) ) ;
#14651 = CYLINDRICAL_SURFACE ( 'NONE', #18456, 2.000000000000001776 ) ;
#14652 = CARTESIAN_POINT ( 'NONE',  ( 6.001413532006936613, -13.74047052604243646, -9.312396943078789846 ) ) ;
#14653 = CARTESIAN_POINT ( 'NONE',  ( 8.823509210239544487, 27.84164230456639544, 47.04930799450051637 ) ) ;
#14654 = CARTESIAN_POINT ( 'NONE',  ( 21.09785597605719332, 11.92558985988973497, 47.04930799450051637 ) ) ;
#14655 = DIRECTION ( 'NONE',  ( 0.4848096202463429982, 0.8746197071393925215, 9.920727850371698576E-18 ) ) ;
#14656 = ADVANCED_FACE ( 'NONE', ( #4666 ), #4344, .T. ) ;
#14657 = ORIENTED_EDGE ( 'NONE', *, *, #17036, .T. ) ;
#14658 = CARTESIAN_POINT ( 'NONE',  ( -40.59783130604490253, 7.538194345349025660, 53.99315859930123906 ) ) ;
#14659 = CARTESIAN_POINT ( 'NONE',  ( 47.26255010802070444, 24.99819976284614853, 43.87815533714887550 ) ) ;
#14660 = CARTESIAN_POINT ( 'NONE',  ( -29.83711070102105012, 6.212614032769436356, 17.22340695172378844 ) ) ;
#14661 = VECTOR ( 'NONE', #13499, 1000.000000000000000 ) ;
#14662 = TOROIDAL_SURFACE ( 'NONE', #21966, 20.49999999999999645, 1.499999999999997780 ) ;
#14663 = CARTESIAN_POINT ( 'NONE',  ( 71.48501281440437083, 8.310461108307681144, 75.47198155259907537 ) ) ;
#14664 = VERTEX_POINT ( 'NONE', #12226 ) ;
#14665 = DIRECTION ( 'NONE',  ( -0.8389271868029088974, 0.000000000000000000, -0.5442436726714948714 ) ) ;
#14666 = AXIS2_PLACEMENT_3D ( 'NONE', #31983, #11805, #21800 ) ;
#14667 = DIRECTION ( 'NONE',  ( -1.101824276508909887E-16, 1.000000000000000000, -0.000000000000000000 ) ) ;
#14668 = CARTESIAN_POINT ( 'NONE',  ( 21.09992658989239089, 27.09164230456639899, 47.04930799450051637 ) ) ;
#14669 = ORIENTED_EDGE ( 'NONE', *, *, #20480, .F. ) ;
#14670 = ORIENTED_EDGE ( 'NONE', *, *, #2110, .F. ) ;
#14671 = DIRECTION ( 'NONE',  ( -0.000000000000000000, -1.000000000000000000, 0.000000000000000000 ) ) ;
#14672 = CARTESIAN_POINT ( 'NONE',  ( 21.09785597605719332, 30.56454579224779522, 73.04930799450052348 ) ) ;
#14673 = LINE ( 'NONE', #12211, #30410 ) ;
#14674 = CARTESIAN_POINT ( 'NONE',  ( 21.09992658989239089, 23.72145308207319658, 47.04930799450051637 ) ) ;
#14675 = CARTESIAN_POINT ( 'NONE',  ( 44.81325834503692107, 29.29399940044038786, 46.39891453572019486 ) ) ;
#14676 = VERTEX_POINT ( 'NONE', #29619 ) ;
#14677 = ADVANCED_FACE ( 'NONE', ( #18934 ), #22216, .F. ) ;
#14678 = VECTOR ( 'NONE', #23202, 1000.000000000000000 ) ;
#14679 = EDGE_CURVE ( 'NONE', #12963, #13273, #4081, .T. ) ;
#14680 = ORIENTED_EDGE ( 'NONE', *, *, #29239, .T. ) ;
#14681 = DIRECTION ( 'NONE',  ( -0.000000000000000000, -1.000000000000000000, -0.000000000000000000 ) ) ;
#14682 = EDGE_CURVE ( 'NONE', #27386, #27774, #10370, .T. ) ;
#14683 = AXIS2_PLACEMENT_3D ( 'NONE', #16860, #14739, #9488 ) ;
#14684 = AXIS2_PLACEMENT_3D ( 'NONE', #24280, #11327, #16241 ) ;
#14685 = ORIENTED_EDGE ( 'NONE', *, *, #2230, .F. ) ;
#14686 = ADVANCED_FACE ( 'NONE', ( #21725 ), #1543, .T. ) ;
#14687 = AXIS2_PLACEMENT_3D ( 'NONE', #27606, #12692, #10374 ) ;
#14688 = DIRECTION ( 'NONE',  ( -0.2756373558169973870, 0.9612616959383193382, 1.315048337272770280E-17 ) ) ;
#14689 = CARTESIAN_POINT ( 'NONE',  ( -29.54697681637456697, 7.561619403635258863, 75.88267709390528637 ) ) ;
#14690 = AXIS2_PLACEMENT_3D ( 'NONE', #27370, #9976, #5535 ) ;
#14691 = ORIENTED_EDGE ( 'NONE', *, *, #8418, .T. ) ;
#14692 = CARTESIAN_POINT ( 'NONE',  ( -40.75223430975736960, 8.437483520745759691, 34.54930799450052348 ) ) ;
#14693 = ORIENTED_EDGE ( 'NONE', *, *, #19747, .F. ) ;
#14694 = CARTESIAN_POINT ( 'NONE',  ( -41.01929587258828747, 9.401204285752060130, 35.44930799450052206 ) ) ;
#14695 = DIRECTION ( 'NONE',  ( -1.101824276508909887E-16, 1.000000000000000000, -0.000000000000000000 ) ) ;
#14696 = CARTESIAN_POINT ( 'NONE',  ( 71.77671131497349677, 10.95964320463250807, 71.78996344180542621 ) ) ;
#14697 = ORIENTED_EDGE ( 'NONE', *, *, #17652, .T. ) ;
#14698 = DIRECTION ( 'NONE',  ( 0.2756373558169828430, -0.9612616959383236681, 1.479773560108285391E-16 ) ) ;
#14699 = DIRECTION ( 'NONE',  ( 0.4544104193609903586, 0.000000000000000000, 0.8907924397839087627 ) ) ;
#14700 = CARTESIAN_POINT ( 'NONE',  ( 46.04844006429464542, 19.96454579224779380, 44.99211097489548905 ) ) ;
#14701 = FACE_OUTER_BOUND ( 'NONE', #5928, .T. ) ;
#14702 = CARTESIAN_POINT ( 'NONE',  ( -40.15599670534037102, 7.478908884098768084, 39.44930799450052206 ) ) ;
#14703 = CARTESIAN_POINT ( 'NONE',  ( 21.09785597605720042, -14.24176827912842391, -11.80059343253840609 ) ) ;
#14704 = ORIENTED_EDGE ( 'NONE', *, *, #11365, .T. ) ;
#14705 = CARTESIAN_POINT ( 'NONE',  ( -40.62123369608615775, 7.650200974017423938, 39.54930799450052348 ) ) ;
#14706 = ORIENTED_EDGE ( 'NONE', *, *, #18728, .F. ) ;
#14707 = DIRECTION ( 'NONE',  ( -1.101824276508909887E-16, 1.000000000000000000, -0.000000000000000000 ) ) ;
#14708 = AXIS2_PLACEMENT_3D ( 'NONE', #10946, #11585, #8955 ) ;
#14709 = VECTOR ( 'NONE', #14442, 1000.000000000000000 ) ;
#14710 = DIRECTION ( 'NONE',  ( 0.000000000000000000, -0.6560590289905074979, -0.7547095802227717920 ) ) ;
#14711 = ORIENTED_EDGE ( 'NONE', *, *, #28441, .T. ) ;
#14712 = AXIS2_PLACEMENT_3D ( 'NONE', #8713, #23651, #11493 ) ;
#14713 = ORIENTED_EDGE ( 'NONE', *, *, #2586, .T. ) ;
#14714 = TOROIDAL_SURFACE ( 'NONE', #24660, 12.40141737965280555, 0.1250000000000006939 ) ;
#14715 = CIRCLE ( 'NONE', #5735, 0.1000000000000018235 ) ;
#14716 = AXIS2_PLACEMENT_3D ( 'NONE', #12693, #27607, #13335 ) ;
#14717 = ORIENTED_EDGE ( 'NONE', *, *, #5589, .T. ) ;
#14718 = TOROIDAL_SURFACE ( 'NONE', #20478, 39.69941114636694834, 1.000000000000000000 ) ;
#14719 = EDGE_CURVE ( 'NONE', #26434, #22710, #9301, .T. ) ;
#14720 = EDGE_CURVE ( 'NONE', #22190, #13364, #29241, .T. ) ;
#14721 = CIRCLE ( 'NONE', #19943, 0.1250000000000001110 ) ;
#14722 = VERTEX_POINT ( 'NONE', #21887 ) ;
#14723 = EDGE_LOOP ( 'NONE', ( #17657, #20517, #4815, #19791 ) ) ;
#14724 = FACE_OUTER_BOUND ( 'NONE', #26311, .T. ) ;
#14725 = CARTESIAN_POINT ( 'NONE',  ( 21.09785597605719332, 13.74476430820393347, 47.04930799450051637 ) ) ;
#14726 = TOROIDAL_SURFACE ( 'NONE', #19959, 83.95481021798164534, 94.94530576803616384 ) ;
#14727 = FACE_OUTER_BOUND ( 'NONE', #12941, .T. ) ;
#14728 = CARTESIAN_POINT ( 'NONE',  ( 8.474859994195286461, 25.34143805560860940, 47.04930799450051637 ) ) ;
#14729 = AXIS2_PLACEMENT_3D ( 'NONE', #14646, #31717, #7257 ) ;
#14730 = DIRECTION ( 'NONE',  ( -1.000000000000000000, 0.000000000000000000, 0.000000000000000000 ) ) ;
#14731 = AXIS2_PLACEMENT_3D ( 'NONE', #4351, #6811, #16813 ) ;
#14732 = ORIENTED_EDGE ( 'NONE', *, *, #10087, .T. ) ;
#14733 = CARTESIAN_POINT ( 'NONE',  ( -7.783295380925389750, 7.511668073839847359, 97.69862240222212790 ) ) ;
#14734 = ORIENTED_EDGE ( 'NONE', *, *, #12985, .T. ) ;
#14735 = FACE_OUTER_BOUND ( 'NONE', #6045, .T. ) ;
#14736 = ORIENTED_EDGE ( 'NONE', *, *, #26081, .F. ) ;
#14737 = DIRECTION ( 'NONE',  ( 0.2756373558170128191, -0.9612616959383148973, 0.000000000000000000 ) ) ;
#14738 = DIRECTION ( 'NONE',  ( 0.4848096202463430537, 0.8746197071393926326, 9.920727850371700117E-18 ) ) ;
#14739 = DIRECTION ( 'NONE',  ( -1.101824276508909887E-16, 1.000000000000000000, -0.000000000000000000 ) ) ;
#14740 = FACE_OUTER_BOUND ( 'NONE', #20078, .T. ) ;
#14741 = CARTESIAN_POINT ( 'NONE',  ( -41.74593813222361405, 15.43463958587387808, 38.54930799450052348 ) ) ;
#14742 = CARTESIAN_POINT ( 'NONE',  ( 45.35708200440645044, 26.20457786121582444, 45.92000246470679770 ) ) ;
#14743 = SHAPE_REPRESENTATION ( 'Coil', ( #8172 ), #331 ) ;
#14744 = CARTESIAN_POINT ( 'NONE',  ( 33.72499318558949000, 38.56284415653841791, 47.04930799450051637 ) ) ;
#14745 = DIRECTION ( 'NONE',  ( -1.000000000000000000, -0.000000000000000000, -3.491481338843133355E-15 ) ) ;
#14746 = EDGE_LOOP ( 'NONE', ( #23171, #29752, #31997, #14278 ) ) ;
#14747 = B_SPLINE_CURVE_WITH_KNOTS ( 'NONE', 3,
 ( #18739, #26144, #21361, #31245 ),
 .UNSPECIFIED., .F., .F.,
 ( 4, 4 ),
 ( 0.000000000000000000, 0.0001556073905087536054 ),
 .UNSPECIFIED. ) ;
#14748 = CARTESIAN_POINT ( 'NONE',  ( 21.09785597605719332, 14.58544108513610027, 47.04930799450051637 ) ) ;
#14749 = DIRECTION ( 'NONE',  ( -1.101824276508909887E-16, 1.000000000000000000, -0.000000000000000000 ) ) ;
#14750 = ORIENTED_EDGE ( 'NONE', *, *, #1207, .T. ) ;
#14751 = CARTESIAN_POINT ( 'NONE',  ( 21.09785597605719332, 40.56454579224779877, 64.04930799450050927 ) ) ;
#14752 = CARTESIAN_POINT ( 'NONE',  ( -40.50726676055796105, 7.559560307024983494, 53.54930799450051637 ) ) ;
#14753 = VERTEX_POINT ( 'NONE', #29458 ) ;
#14754 = VERTEX_POINT ( 'NONE', #9433 ) ;
#14755 = CARTESIAN_POINT ( 'NONE',  ( 8.732853799281718565, 31.22145308207317171, 47.04930799450051637 ) ) ;
#14756 = ORIENTED_EDGE ( 'NONE', *, *, #28648, .F. ) ;
#14757 = TOROIDAL_SURFACE ( 'NONE', #22076, 12.40141737965286239, 0.1250000000000005551 ) ;
#14758 = AXIS2_PLACEMENT_3D ( 'NONE', #18945, #28816, #4355 ) ;
#14759 = EDGE_CURVE ( 'NONE', #22795, #20651, #15106, .T. ) ;
#14760 = ADVANCED_FACE ( 'NONE', ( #10406 ), #4834, .T. ) ;
#14761 = EDGE_CURVE ( 'NONE', #28974, #11047, #27661, .T. ) ;
#14762 = ORIENTED_EDGE ( 'NONE', *, *, #28637, .F. ) ;
#14763 = EDGE_CURVE ( 'NONE', #22939, #5375, #18725, .T. ) ;
#14764 = EDGE_CURVE ( 'NONE', #15368, #16515, #22938, .T. ) ;
#14765 = DIRECTION ( 'NONE',  ( 0.8746197071393858602, -0.4848096202463547666, 0.000000000000000000 ) ) ;
#14766 = DIRECTION ( 'NONE',  ( 0.000000000000000000, 0.000000000000000000, 1.000000000000000000 ) ) ;
#14767 = AXIS2_PLACEMENT_3D ( 'NONE', #12771, #17998, #608 ) ;
#14768 = ORIENTED_EDGE ( 'NONE', *, *, #13066, .F. ) ;
#14769 = DIRECTION ( 'NONE',  ( 0.000000000000000000, -1.000000000000000000, 0.000000000000000000 ) ) ;
#14770 = CARTESIAN_POINT ( 'NONE',  ( -42.21195563036362586, 4.051200314738734320, 57.04930799450051637 ) ) ;
#14771 = CARTESIAN_POINT ( 'NONE',  ( 33.71785032049100295, 29.96664230456641675, 47.04930799450051637 ) ) ;
#14772 = CARTESIAN_POINT ( 'NONE',  ( 48.83862994770794330, 25.15457786121582373, 48.17861352429476796 ) ) ;
#14773 = ORIENTED_EDGE ( 'NONE', *, *, #22337, .F. ) ;
#14774 = ORIENTED_EDGE ( 'NONE', *, *, #23515, .T. ) ;
#14775 = SURFACE_SIDE_STYLE ('',( #16897 ) ) ;
#14776 = EDGE_LOOP ( 'NONE', ( #4498, #18876, #9023, #29202 ) ) ;
#14777 = DIRECTION ( 'NONE',  ( 0.000000000000000000, 0.000000000000000000, -1.000000000000000000 ) ) ;
#14778 = AXIS2_PLACEMENT_3D ( 'NONE', #23563, #8480, #3052 ) ;
#14779 = DIRECTION ( 'NONE',  ( -1.101824276508909887E-16, 1.000000000000000000, -0.000000000000000000 ) ) ;
#14780 = CARTESIAN_POINT ( 'NONE',  ( -40.69503817910143084, 6.787791837620303248, 34.66137507890927338 ) ) ;
#14781 = AXIS2_PLACEMENT_3D ( 'NONE', #24174, #28781, #6782 ) ;
#14782 = CYLINDRICAL_SURFACE ( 'NONE', #3159, 0.1000000000000006301 ) ;
#14783 = CARTESIAN_POINT ( 'NONE',  ( 45.79384627280941089, 28.47957786121581591, 49.05938063676249072 ) ) ;
#14784 = SHAPE_DEFINITION_REPRESENTATION ( #2233, #21423 ) ;
#14785 = ORIENTED_EDGE ( 'NONE', *, *, #894, .F. ) ;
#14786 = EDGE_LOOP ( 'NONE', ( #20954, #8324, #24460, #24185 ) ) ;
#14787 = CARTESIAN_POINT ( 'NONE',  ( -36.59542768321662720, 12.56771722797891400, 37.04930799450052348 ) ) ;
#14788 = CARTESIAN_POINT ( 'NONE',  ( 21.09785597605720042, -16.63545420775220407, 47.04930799450051637 ) ) ;
#14789 = DIRECTION ( 'NONE',  ( -1.000000000000000000, 0.000000000000000000, 0.000000000000000000 ) ) ;
#14790 = VERTEX_POINT ( 'NONE', #7296 ) ;
#14791 = DIRECTION ( 'NONE',  ( -6.722685822323786766E-17, 1.000000000000000000, -0.000000000000000000 ) ) ;
#14792 = DIRECTION ( 'NONE',  ( 1.000000000000000000, 0.000000000000000000, 0.000000000000000000 ) ) ;
#14793 = VERTEX_POINT ( 'NONE', #27635 ) ;
#14794 = DIRECTION ( 'NONE',  ( 0.000000000000000000, 0.000000000000000000, -1.000000000000000000 ) ) ;
#14795 = FACE_OUTER_BOUND ( 'NONE', #11356, .T. ) ;
#14796 = EDGE_CURVE ( 'NONE', #14341, #22032, #17464, .T. ) ;
#14797 = CIRCLE ( 'NONE', #1160, 13.00178401536290806 ) ;
#14798 = FACE_OUTER_BOUND ( 'NONE', #17926, .T. ) ;
#14799 = VECTOR ( 'NONE', #12021, 1000.000000000000000 ) ;
#14800 = VECTOR ( 'NONE', #6574, 1000.000000000000000 ) ;
#14801 = ORIENTED_EDGE ( 'NONE', *, *, #10774, .F. ) ;
#14802 = EDGE_CURVE ( 'NONE', #16982, #7700, #4998, .T. ) ;
#14803 = AXIS2_PLACEMENT_3D ( 'NONE', #12128, #19496, #24586 ) ;
#14804 = VERTEX_POINT ( 'NONE', #12723 ) ;
#14805 = ADVANCED_FACE ( 'NONE', ( #25179 ), #27664, .F. ) ;
#14806 = DIRECTION ( 'NONE',  ( 0.000000000000000000, 1.000000000000000000, 0.000000000000000000 ) ) ;
#14807 = CARTESIAN_POINT ( 'NONE',  ( 73.74052036900765472, 11.92558985988972964, 68.00755811609985813 ) ) ;
#14808 = DIRECTION ( 'NONE',  ( -1.000000000000000000, -1.101824276508909887E-16, 0.000000000000000000 ) ) ;
#14809 = EDGE_LOOP ( 'NONE', ( #18785, #7416, #18139, #20035 ) ) ;
#14810 = DIRECTION ( 'NONE',  ( 0.000000000000000000, -0.000000000000000000, -1.000000000000000000 ) ) ;
#14811 = CARTESIAN_POINT ( 'NONE',  ( 21.09992658989239089, 27.84164230456639544, 47.04930799450051637 ) ) ;
#14812 = DIRECTION ( 'NONE',  ( 0.000000000000000000, 0.000000000000000000, 1.000000000000000000 ) ) ;
#14813 = DIRECTION ( 'NONE',  ( -0.8907924397839087627, -1.100109291107994187E-16, 0.4544104193609907472 ) ) ;
#14814 = CARTESIAN_POINT ( 'NONE',  ( 21.09785597605720753, 13.86454579224779948, 47.04930799450052348 ) ) ;
#14815 = CARTESIAN_POINT ( 'NONE',  ( -14.41812891119676188, -13.74047052604243646, 0.7550407962218198543 ) ) ;
#14816 = FACE_BOUND ( 'NONE', #27753, .T. ) ;
#14817 = CIRCLE ( 'NONE', #4859, 12.62506659569710266 ) ;
#14818 = PRODUCT_DEFINITION_SHAPE ( 'NONE', 'NONE',  #27968 ) ;
#14819 = CARTESIAN_POINT ( 'NONE',  ( 21.09992658989238734, 38.56284415653841791, 47.04930799450051637 ) ) ;
#14820 = AXIS2_PLACEMENT_3D ( 'NONE', #2330, #12347, #22340 ) ;
#14821 = DIRECTION ( 'NONE',  ( -1.000000000000000000, 0.000000000000000000, 0.000000000000000000 ) ) ;
#14822 = ORIENTED_EDGE ( 'NONE', *, *, #19135, .F. ) ;
#14823 = VERTEX_POINT ( 'NONE', #12552 ) ;
#14824 = LINE ( 'NONE', #204, #28601 ) ;
#14825 = CARTESIAN_POINT ( 'NONE',  ( 45.84097905237065618, 22.86454579224779948, 48.98672734302541443 ) ) ;
#14827 = EDGE_CURVE ( 'NONE', #12384, #29330, #3543, .T. ) ;
#14826 = TOROIDAL_SURFACE ( 'NONE', #9570, 12.61792373059891403, 0.1250000000000023315 ) ;
#14828 = CARTESIAN_POINT ( 'NONE',  ( -40.17244512953781310, 6.931285263614340053, 34.54930799450052348 ) ) ;
#14829 = CARTESIAN_POINT ( 'NONE',  ( 49.32483701613094240, 27.12587066347689557, 45.91328182968236860 ) ) ;
#14830 = ORIENTED_EDGE ( 'NONE', *, *, #17656, .T. ) ;
#14831 = CIRCLE ( 'NONE', #12755, 12.27641737965282154 ) ;
#14832 = CARTESIAN_POINT ( 'NONE',  ( 50.59785597605720397, 14.86454579224779948, 47.04930799450051637 ) ) ;
#14833 = DIRECTION ( 'NONE',  ( -2.779292025043186357E-18, 1.288349127009862211E-17, -1.000000000000000000 ) ) ;
#14834 = DIRECTION ( 'NONE',  ( -1.000000000000000000, 0.000000000000000000, 0.000000000000000000 ) ) ;
#14835 = ORIENTED_EDGE ( 'NONE', *, *, #10656, .F. ) ;
#14836 = VERTEX_POINT ( 'NONE', #22541 ) ;
#14837 = DIRECTION ( 'NONE',  ( 0.000000000000000000, 0.000000000000000000, -1.000000000000000000 ) ) ;
#14838 = CARTESIAN_POINT ( 'NONE',  ( -42.37913764077812573, 15.23192269303853053, 35.64930799450052490 ) ) ;
#14839 = EDGE_CURVE ( 'NONE', #27529, #7227, #9858, .T. ) ;
#14840 = ADVANCED_FACE ( 'NONE', ( #9763 ), #5327, .T. ) ;
#14841 = DIRECTION ( 'NONE',  ( -0.9999997877697283100, 0.0006515063303658816165, -1.224646539240230088E-16 ) ) ;
#14842 = DIRECTION ( 'NONE',  ( -1.101824276508909887E-16, 1.000000000000000000, -0.000000000000000000 ) ) ;
#14843 = CARTESIAN_POINT ( 'NONE',  ( 45.99457799031791438, 29.23661293962803143, 44.88652376508412090 ) ) ;
#14844 = ORIENTED_EDGE ( 'NONE', *, *, #20222, .F. ) ;
#14845 = VERTEX_POINT ( 'NONE', #25502 ) ;
#14846 = VECTOR ( 'NONE', #20294, 1000.000000000000114 ) ;
#14847 = EDGE_CURVE ( 'NONE', #3864, #26992, #1456, .T. ) ;
#14848 = FACE_OUTER_BOUND ( 'NONE', #12601, .T. ) ;
#14849 = ORIENTED_EDGE ( 'NONE', *, *, #3204, .T. ) ;
#14850 = VECTOR ( 'NONE', #19581, 1000.000000000000000 ) ;
#14851 = DIRECTION ( 'NONE',  ( -1.000000000000000000, 0.000000000000000000, 0.000000000000000000 ) ) ;
#14852 = ORIENTED_EDGE ( 'NONE', *, *, #29084, .T. ) ;
#14853 = DIRECTION ( 'NONE',  ( -0.8746197071393925215, 0.4848096202463429982, 8.676864087101708112E-18 ) ) ;
#14854 = ORIENTED_EDGE ( 'NONE', *, *, #17331, .F. ) ;
#14855 = CARTESIAN_POINT ( 'NONE',  ( 35.09963999142011204, 16.03967147762300982, 47.04930799450052348 ) ) ;
#14856 = EDGE_CURVE ( 'NONE', #17323, #104, #381, .T. ) ;
#14857 = CARTESIAN_POINT ( 'NONE',  ( 33.46699938050302592, 31.72145308207317882, 47.04930799450050927 ) ) ;
#14858 = DIRECTION ( 'NONE',  ( -0.000000000000000000, -1.000000000000000000, -0.000000000000000000 ) ) ;
#14859 = EDGE_LOOP ( 'NONE', ( #5880, #3238, #32383, #32333, #14229, #25412 ) ) ;
#14860 = DIRECTION ( 'NONE',  ( -0.000000000000000000, -1.000000000000000000, -0.000000000000000000 ) ) ;
#14861 = CARTESIAN_POINT ( 'NONE',  ( 21.09992658989239089, 24.84164230456639544, 47.04930799450051637 ) ) ;
#14862 = CARTESIAN_POINT ( 'NONE',  ( -42.22510282758591416, 14.66434666503944051, 60.54930799450051637 ) ) ;
#14863 = DIRECTION ( 'NONE',  ( 0.000000000000000000, 0.000000000000000000, -1.000000000000000000 ) ) ;
#14864 = EDGE_CURVE ( 'NONE', #28859, #32358, #20401, .T. ) ;
#14865 = DIRECTION ( 'NONE',  ( 0.9612616959383221138, 0.2756373558169876170, 0.000000000000000000 ) ) ;
#14866 = AXIS2_PLACEMENT_3D ( 'NONE', #26676, #8791, #6499 ) ;
#14867 = VERTEX_POINT ( 'NONE', #13036 ) ;
#14868 = DIRECTION ( 'NONE',  ( -1.101824276508909887E-16, 1.000000000000000000, -0.000000000000000000 ) ) ;
#14869 = DIRECTION ( 'NONE',  ( -0.000000000000000000, 1.000000000000000000, -0.000000000000000000 ) ) ;
#14870 = CIRCLE ( 'NONE', #19030, 2.499999999999999112 ) ;
#14871 = ORIENTED_EDGE ( 'NONE', *, *, #3221, .T. ) ;
#14872 = FACE_OUTER_BOUND ( 'NONE', #23304, .T. ) ;
#14873 = ADVANCED_FACE ( 'NONE', ( #17946 ), #19790, .T. ) ;
#14874 = DIRECTION ( 'NONE',  ( 1.000000000000000000, 0.000000000000000000, 0.000000000000000000 ) ) ;
#14875 = EDGE_CURVE ( 'NONE', #3250, #16822, #28198, .T. ) ;
#14876 = AXIS2_PLACEMENT_3D ( 'NONE', #28152, #15987, #30617 ) ;
#14877 = VERTEX_POINT ( 'NONE', #21196 ) ;
#14878 = VECTOR ( 'NONE', #4290, 1000.000000000000114 ) ;
#14879 = CIRCLE ( 'NONE', #14358, 12.52247886585643677 ) ;
#14880 = ORIENTED_EDGE ( 'NONE', *, *, #7310, .F. ) ;
#14881 = ORIENTED_EDGE ( 'NONE', *, *, #16376, .F. ) ;
#14882 = AXIS2_PLACEMENT_3D ( 'NONE', #23893, #1404, #1179 ) ;
#14883 = CARTESIAN_POINT ( 'NONE',  ( 48.28214861297873028, 24.78954579807170333, 49.37090702980594870 ) ) ;
#14884 = VERTEX_POINT ( 'NONE', #18420 ) ;
#14885 = EDGE_LOOP ( 'NONE', ( #23888, #11907, #16811 ) ) ;
#14886 = CARTESIAN_POINT ( 'NONE',  ( 75.17570804623589709, -2.284241381456150410, 13.31978822362705195 ) ) ;
#14887 = AXIS2_PLACEMENT_3D ( 'NONE', #13897, #11421, #21415 ) ;
#14888 = CARTESIAN_POINT ( 'NONE',  ( 42.60151274628839246, 11.88152873911358753, -5.399210173220353681 ) ) ;
#14889 = DIRECTION ( 'NONE',  ( -1.000000000000000000, 0.000000000000000000, 0.000000000000000000 ) ) ;
#14890 = FACE_OUTER_BOUND ( 'NONE', #1137, .T. ) ;
#14891 = EDGE_CURVE ( 'NONE', #17834, #4178, #30265, .T. ) ;
#14892 = DIRECTION ( 'NONE',  ( -1.101824276508909887E-16, 1.000000000000000000, -0.000000000000000000 ) ) ;
#14893 = EDGE_LOOP ( 'NONE', ( #3453, #21649, #27667, #3028 ) ) ;
#14894 = CARTESIAN_POINT ( 'NONE',  ( -10.80606256024020873, 2.793366809690227992, 98.94773045085101160 ) ) ;
#14895 = ORIENTED_EDGE ( 'NONE', *, *, #18040, .T. ) ;
#14896 = DIRECTION ( 'NONE',  ( 0.000000000000000000, 0.000000000000000000, -1.000000000000000000 ) ) ;
#14897 = CARTESIAN_POINT ( 'NONE',  ( 80.24225075505094651, -5.881344816830196720, 15.57390435040008114 ) ) ;
#14898 = ORIENTED_EDGE ( 'NONE', *, *, #6214, .F. ) ;
#14899 = CARTESIAN_POINT ( 'NONE',  ( 81.79971628361815306, -5.935454207752202116, 77.87546120947918382 ) ) ;
#14900 = CARTESIAN_POINT ( 'NONE',  ( 21.09992658989239089, 29.34164230456639899, 47.04930799450051637 ) ) ;
#14901 = EDGE_CURVE ( 'NONE', #5070, #313, #18102, .T. ) ;
#14902 = CARTESIAN_POINT ( 'NONE',  ( -41.55884944519204538, 7.292100401678685451, 39.54930799450052348 ) ) ;
#14903 = CARTESIAN_POINT ( 'NONE',  ( -40.58856461370174884, 7.499380836222963254, 60.14930799450051779 ) ) ;
#14904 = CARTESIAN_POINT ( 'NONE',  ( 21.09785597605720753, 13.86454579224779948, 47.04930799450052348 ) ) ;
#14905 = CARTESIAN_POINT ( 'NONE',  ( 45.35708200440645044, 27.60457786121581947, 45.92000246470679770 ) ) ;
#14906 = CARTESIAN_POINT ( 'NONE',  ( -40.11729073372970333, 6.802967823440400075, 34.64930799450051779 ) ) ;
#14907 = CYLINDRICAL_SURFACE ( 'NONE', #6477, 12.36707279061065101 ) ;
#14908 = ORIENTED_EDGE ( 'NONE', *, *, #22117, .T. ) ;
#14909 = CARTESIAN_POINT ( 'NONE',  ( 47.13159012232203082, 29.60361862379404840, 44.98865247363699638 ) ) ;
#14910 = DIRECTION ( 'NONE',  ( -1.101824276508909887E-16, 1.000000000000000000, -0.000000000000000000 ) ) ;
#14911 = ORIENTED_EDGE ( 'NONE', *, *, #16556, .F. ) ;
#14912 = EDGE_CURVE ( 'NONE', #16822, #5228, #22446, .T. ) ;
#14913 = CARTESIAN_POINT ( 'NONE',  ( -4.902144023942810236, 25.56454579224779877, 47.04930799450078638 ) ) ;
#14914 = EDGE_LOOP ( 'NONE', ( #3776, #5033, #575, #1325 ) ) ;
#14915 = CIRCLE ( 'NONE', #23292, 18.86195243859455672 ) ;
#14916 = ORIENTED_EDGE ( 'NONE', *, *, #5190, .F. ) ;
#14917 = DIRECTION ( 'NONE',  ( -1.000000000000000000, -1.101824276508909887E-16, 0.000000000000000000 ) ) ;
#14918 = TOROIDAL_SURFACE ( 'NONE', #6513, 12.40141737965281621, 0.1249999999999985428 ) ;
#14919 = AXIS2_PLACEMENT_3D ( 'NONE', #15294, #14649, #14973 ) ;
#14920 = TOROIDAL_SURFACE ( 'NONE', #11254, 12.40141737965284996, 0.1250000000000002776 ) ;
#14921 = ORIENTED_EDGE ( 'NONE', *, *, #21556, .F. ) ;
#14922 = ORIENTED_EDGE ( 'NONE', *, *, #7352, .T. ) ;
#14923 = DIRECTION ( 'NONE',  ( -1.000000000000000000, -1.101824276508909887E-16, 0.000000000000000000 ) ) ;
#14924 = EDGE_LOOP ( 'NONE', ( #32012, #5784, #19688, #29061 ) ) ;
#14925 = CARTESIAN_POINT ( 'NONE',  ( 21.09785597605720753, -5.098646251524523443, 47.04930799450052348 ) ) ;
#14926 =( BOUNDED_SURFACE ( )  B_SPLINE_SURFACE ( 3, 2, ( 
 ( #23227, #15841, #20761 ),
 ( #5839, #25844, #21383 ),
 ( #31746, #26648, #23542 ),
 ( #3512, #4004, #6791 ) ),
 .UNSPECIFIED., .F., .F., .F. ) 
 B_SPLINE_SURFACE_WITH_KNOTS ( ( 4, 4 ),
 ( 3, 3 ),
 ( 1.570796326794896558, 1.630650672327996542 ),
 ( 0.000000000000000000, 1.000000000000000000 ),
 .UNSPECIFIED. ) 
 GEOMETRIC_REPRESENTATION_ITEM ( )  RATIONAL_B_SPLINE_SURFACE ( (
 ( 1.000000000000000000, 0.7071067811865515695, 1.000000000000000000),
 ( 1.000000000000000000, 0.7120946502353932006, 1.000000000000000000),
 ( 1.000000000000000000, 0.7170297040967722468, 1.000000000000000000),
 ( 1.000000000000000000, 0.7219065546282052992, 1.000000000000000000) ) ) 
 REPRESENTATION_ITEM ( '' )  SURFACE ( )  );
#14927 = CARTESIAN_POINT ( 'NONE',  ( 21.09992658989239089, 28.21183152705961206, 47.04930799450051637 ) ) ;
#14928 = DIRECTION ( 'NONE',  ( -0.000000000000000000, -1.000000000000000000, -0.000000000000000000 ) ) ;
#14929 = CARTESIAN_POINT ( 'NONE',  ( 48.94625023931840957, 26.67124452788248945, 46.10640627770150246 ) ) ;
#14930 = VERTEX_POINT ( 'NONE', #16283 ) ;
#14931 = ORIENTED_EDGE ( 'NONE', *, *, #27468, .F. ) ;
#14933 = DIRECTION ( 'NONE',  ( 0.2756373558169974980, -0.9612616959383193382, -1.315048337272770589E-17 ) ) ;
#14932 = CIRCLE ( 'NONE', #8657, 0.1250000000000001110 ) ;
#14934 = AXIS2_PLACEMENT_3D ( 'NONE', #7570, #20192, #32026 ) ;
#14935 = ORIENTED_EDGE ( 'NONE', *, *, #17037, .F. ) ;
#14936 = DIRECTION ( 'NONE',  ( 0.4848096202463429427, 0.8746197071393925215, -2.352477780477436787E-16 ) ) ;
#14937 = AXIS2_PLACEMENT_3D ( 'NONE', #12955, #18021, #13283 ) ;
#14938 = DIRECTION ( 'NONE',  ( -1.000000000000000000, -1.101824276508910010E-16, 0.000000000000000000 ) ) ;
#14939 = DIRECTION ( 'NONE',  ( 0.7848668881104262640, 0.2250569586005336520, -0.5773502691896258421 ) ) ;
#14940 = DIRECTION ( 'NONE',  ( -1.101824276508909887E-16, 1.000000000000000000, -0.000000000000000000 ) ) ;
#14941 = DIRECTION ( 'NONE',  ( -0.000000000000000000, -1.000000000000000000, -0.000000000000000000 ) ) ;
#14942 = APPLICATION_PROTOCOL_DEFINITION ( 'draft international standard', 'automotive_design', 1998, #29222 ) ;
#14943 = EDGE_LOOP ( 'NONE', ( #14317, #21754, #7901, #29595 ) ) ;
#14944 = VERTEX_POINT ( 'NONE', #3813 ) ;
#14945 = DIRECTION ( 'NONE',  ( 0.000000000000000000, -1.000000000000000000, 0.000000000000000000 ) ) ;
#14946 = FACE_OUTER_BOUND ( 'NONE', #25065, .T. ) ;
#14947 = EDGE_CURVE ( 'NONE', #26256, #32220, #18246, .T. ) ;
#14948 = EDGE_CURVE ( 'NONE', #1830, #12799, #22487, .T. ) ;
#14949 = DIRECTION ( 'NONE',  ( -1.101824276508909887E-16, 1.000000000000000000, -0.000000000000000000 ) ) ;
#14950 = EDGE_CURVE ( 'NONE', #26169, #13889, #31362, .T. ) ;
#14951 = ADVANCED_FACE ( 'NONE', ( #8735 ), #30754, .T. ) ;
#14952 = EDGE_LOOP ( 'NONE', ( #23379, #21174, #16722, #3309 ) ) ;
#14953 = CARTESIAN_POINT ( 'NONE',  ( 48.83862994770794330, 27.34118040159426499, 48.17861352429476796 ) ) ;
#14954 = ORIENTED_EDGE ( 'NONE', *, *, #4854, .F. ) ;
#14955 = FACE_OUTER_BOUND ( 'NONE', #17119, .T. ) ;
#14956 = FACE_OUTER_BOUND ( 'NONE', #15567, .T. ) ;
#14957 = CYLINDRICAL_SURFACE ( 'NONE', #22777, 34.00000000000000000 ) ;
#14958 = CIRCLE ( 'NONE', #7095, 2.500000000000003553 ) ;
#14959 = AXIS2_PLACEMENT_3D ( 'NONE', #15571, #20660, #30529 ) ;
#14960 = AXIS2_PLACEMENT_3D ( 'NONE', #2049, #20253, #25025 ) ;
#14961 = CIRCLE ( 'NONE', #6565, 3.699999999999994849 ) ;
#14962 = VECTOR ( 'NONE', #14853, 1000.000000000000114 ) ;
#14963 = VERTEX_POINT ( 'NONE', #10577 ) ;
#14964 = ORIENTED_EDGE ( 'NONE', *, *, #18733, .F. ) ;
#14965 = CARTESIAN_POINT ( 'NONE',  ( -38.44253683272001609, -5.930168697284449841, 15.95990681549819534 ) ) ;
#14966 = DIRECTION ( 'NONE',  ( -1.101824276508909887E-16, 1.000000000000000000, -0.000000000000000000 ) ) ;
#14967 = CARTESIAN_POINT ( 'NONE',  ( 49.49063479933183629, 25.99951373492759643, 47.17357720316391578 ) ) ;
#14968 = ORIENTED_EDGE ( 'NONE', *, *, #20030, .F. ) ;
#14969 = DIRECTION ( 'NONE',  ( 0.000000000000000000, 0.000000000000000000, 1.000000000000000000 ) ) ;
#14970 = CARTESIAN_POINT ( 'NONE',  ( 21.09785597605719332, 24.74924423484549507, 47.04930799450051637 ) ) ;
#14971 = ADVANCED_FACE ( 'NONE', ( #23681 ), #24535, .T. ) ;
#14972 = LINE ( 'NONE', #24974, #384 ) ;
#14973 = DIRECTION ( 'NONE',  ( 0.4544104193609900810, 5.611869858668441979E-17, 0.8907924397839090958 ) ) ;
#14974 = DIRECTION ( 'NONE',  ( -1.101824276508909887E-16, 1.000000000000000000, -0.000000000000000000 ) ) ;
#14975 = DIRECTION ( 'NONE',  ( -0.2756373558169961102, 0.9612616959383197823, 0.000000000000000000 ) ) ;
#14976 = CARTESIAN_POINT ( 'NONE',  ( 21.09785597605720042, -14.04221034894631615, -11.61388374861560635 ) ) ;
#14977 = DIRECTION ( 'NONE',  ( -0.8746197071393925215, 0.4848096202463429982, 8.676864087101709653E-18 ) ) ;
#14978 = AXIS2_PLACEMENT_3D ( 'NONE', #4709, #7505, #27521 ) ;
#14979 = DIRECTION ( 'NONE',  ( 0.4441739386571981751, -0.2110602665713104398, 0.8707256032141232893 ) ) ;
#14980 = LINE ( 'NONE', #12024, #13725 ) ;
#14981 = ORIENTED_EDGE ( 'NONE', *, *, #1582, .T. ) ;
#14982 = VERTEX_POINT ( 'NONE', #28600 ) ;
#14983 = CARTESIAN_POINT ( 'NONE',  ( 21.09992658989238734, 30.84184655352422411, 47.04930799450051637 ) ) ;
#14984 = VECTOR ( 'NONE', #18908, 1000.000000000000000 ) ;
#14985 = CARTESIAN_POINT ( 'NONE',  ( 21.09992658989239089, 30.09164230456639544, 47.04930799450051637 ) ) ;
#14986 = CIRCLE ( 'NONE', #3368, 0.1000000000000018235 ) ;
#14987 = EDGE_CURVE ( 'NONE', #2302, #10357, #31066, .T. ) ;
#14988 = DIRECTION ( 'NONE',  ( -1.101824276508909887E-16, 1.000000000000000000, -0.000000000000000000 ) ) ;
#14989 = ADVANCED_FACE ( 'NONE', ( #18254 ), #3330, .F. ) ;
#14990 = ADVANCED_FACE ( 'NONE', ( #867 ), #10891, .T. ) ;
#14991 = ORIENTED_EDGE ( 'NONE', *, *, #31836, .F. ) ;
#14992 = DIRECTION ( 'NONE',  ( -1.101824276508909887E-16, 1.000000000000000000, -0.000000000000000000 ) ) ;
#14993 = DIRECTION ( 'NONE',  ( 1.000000000000000000, 0.000000000000000000, 0.000000000000000000 ) ) ;
#14994 = CARTESIAN_POINT ( 'NONE',  ( 45.31840898497604542, 11.19016079752309167, -3.739202734180806953 ) ) ;
#14995 = ORIENTED_EDGE ( 'NONE', *, *, #26483, .F. ) ;
#14996 = ORIENTED_EDGE ( 'NONE', *, *, #10967, .F. ) ;
#14997 = CARTESIAN_POINT ( 'NONE',  ( -40.13633318854532916, 6.906174383240057502, 39.54018667097405171 ) ) ;
#14998 = EDGE_CURVE ( 'NONE', #4372, #11143, #7252, .T. ) ;
#14999 = CARTESIAN_POINT ( 'NONE',  ( 21.09785597605720753, -16.03545420775220265, 117.0483275080932941 ) ) ;
#15000 = LINE ( 'NONE', #25004, #22011 ) ;
#15001 = AXIS2_PLACEMENT_3D ( 'NONE', #1219, #13713, #10776 ) ;
#15002 = CARTESIAN_POINT ( 'NONE',  ( 21.09992658989239089, 28.34164230456639544, 47.04930799450051637 ) ) ;
#15003 = CARTESIAN_POINT ( 'NONE',  ( 44.74186670439651436, 29.31291848938220568, 47.00181081234863001 ) ) ;
#15004 = ORIENTED_EDGE ( 'NONE', *, *, #9122, .F. ) ;
#15005 = ORIENTED_EDGE ( 'NONE', *, *, #13987, .F. ) ;
#15006 = DIRECTION ( 'NONE',  ( -1.000000000000000000, -1.101824276508909887E-16, 0.000000000000000000 ) ) ;
#15007 = AXIS2_PLACEMENT_3D ( 'NONE', #27242, #7065, #27080 ) ;
#15008 = PRODUCT_DEFINITION_FORMATION_WITH_SPECIFIED_SOURCE ( 'ANY', '', #9564, .NOT_KNOWN. ) ;
#15009 = ORIENTED_EDGE ( 'NONE', *, *, #9341, .T. ) ;
#15010 = CYLINDRICAL_SURFACE ( 'NONE', #17622, 12.62506659569710266 ) ;
#15011 = DIRECTION ( 'NONE',  ( -1.000000000000000000, 0.000000000000000000, 0.000000000000000000 ) ) ;
#15012 = EDGE_CURVE ( 'NONE', #10259, #1803, #17196, .T. ) ;
#15013 = ADVANCED_FACE ( 'NONE', ( #11210 ), #28761, .F. ) ;
#15014 = AXIS2_PLACEMENT_3D ( 'NONE', #22377, #19919, #17463 ) ;
#15015 = ORIENTED_EDGE ( 'NONE', *, *, #17375, .F. ) ;
#15016 = CARTESIAN_POINT ( 'NONE',  ( 21.09992658989238734, 32.59164230456639899, 47.04930799450051637 ) ) ;
#15017 = ORIENTED_EDGE ( 'NONE', *, *, #25090, .F. ) ;
#15018 = FACE_OUTER_BOUND ( 'NONE', #19515, .T. ) ;
#15019 = CARTESIAN_POINT ( 'NONE',  ( 21.09785597605719332, 25.56454579224779877, 44.12577010967610391 ) ) ;
#15020 = DIRECTION ( 'NONE',  ( -1.000000000000000000, -1.101824276508909887E-16, 0.000000000000000000 ) ) ;
#15021 = LINE ( 'NONE', #25509, #8698 ) ;
#15022 = VERTEX_POINT ( 'NONE', #3976 ) ;
#15023 = CARTESIAN_POINT ( 'NONE',  ( 78.16097076962940093, -5.523138741469189483, 79.26738665229451897 ) ) ;
#15024 = SPHERICAL_SURFACE ( 'NONE', #7423, 0.1000000000000000056 ) ;
#15025 = DIRECTION ( 'NONE',  ( -0.000000000000000000, 1.000000000000000000, -0.000000000000000000 ) ) ;
#15026 = CARTESIAN_POINT ( 'NONE',  ( 8.732853799281729223, 27.97145308207318237, 47.04930799450051637 ) ) ;
#15027 = CARTESIAN_POINT ( 'NONE',  ( 21.09785597605720753, 13.86454579224779948, 47.04930799450052348 ) ) ;
#15028 = ORIENTED_EDGE ( 'NONE', *, *, #13270, .F. ) ;
#15029 = DIRECTION ( 'NONE',  ( -1.000000000000000000, 0.000000000000000000, 0.000000000000000000 ) ) ;
#15030 = CARTESIAN_POINT ( 'NONE',  ( -48.25869185997735400, 10.94158050198885590, 54.56265170360538264 ) ) ;
#15031 = ORIENTED_EDGE ( 'NONE', *, *, #5362, .F. ) ;
#15032 = EDGE_CURVE ( 'NONE', #14523, #4901, #16928, .T. ) ;
#15033 = DIRECTION ( 'NONE',  ( -1.101824276508909887E-16, 1.000000000000000000, -0.000000000000000000 ) ) ;
#15034 = CIRCLE ( 'NONE', #29719, 0.1250000000000001110 ) ;
#15035 = FACE_OUTER_BOUND ( 'NONE', #6950, .T. ) ;
#15036 = ORIENTED_EDGE ( 'NONE', *, *, #17149, .T. ) ;
#15037 = CARTESIAN_POINT ( 'NONE',  ( -40.73728033978215990, 8.177846351970792682, 54.53299432381886191 ) ) ;
#15038 = ORIENTED_EDGE ( 'NONE', *, *, #26856, .F. ) ;
#15039 = VECTOR ( 'NONE', #14480, 1000.000000000000000 ) ;
#15040 = EDGE_LOOP ( 'NONE', ( #10286, #31423, #30832, #7808 ) ) ;
#15041 = EDGE_CURVE ( 'NONE', #10620, #25220, #8302, .T. ) ;
#15042 = EDGE_CURVE ( 'NONE', #18493, #21006, #30854, .T. ) ;
#15043 = DIRECTION ( 'NONE',  ( 0.8746197071393926326, -0.4848096202463430537, -8.676864087101709653E-18 ) ) ;
#15044 = EDGE_CURVE ( 'NONE', #12276, #27773, #1994, .T. ) ;
#15045 = EDGE_CURVE ( 'NONE', #29138, #11711, #9359, .T. ) ;
#15046 = ORIENTED_EDGE ( 'NONE', *, *, #26449, .F. ) ;
#15047 = EDGE_LOOP ( 'NONE', ( #1433, #30132, #1762, #29658 ) ) ;
#15048 = CARTESIAN_POINT ( 'NONE',  ( 74.25710670715862705, -0.5585041340025438394, 13.65520570039996429 ) ) ;
#15049 = DIRECTION ( 'NONE',  ( -0.8746197071393858602, 0.4848096202463547666, 0.000000000000000000 ) ) ;
#15050 = DIRECTION ( 'NONE',  ( -1.000000000000000000, -1.101824276508909887E-16, 0.000000000000000000 ) ) ;
#15051 = CARTESIAN_POINT ( 'NONE',  ( 21.09785597605720753, 13.86454579224779948, 47.04930799450052348 ) ) ;
#15052 = DIRECTION ( 'NONE',  ( -0.000000000000000000, -1.000000000000000000, 0.000000000000000000 ) ) ;
#15053 = ORIENTED_EDGE ( 'NONE', *, *, #6487, .T. ) ;
#15054 = CARTESIAN_POINT ( 'NONE',  ( -12.63929815817735758, -2.946992577399104807, 101.5552643058159248 ) ) ;
#15055 = EDGE_LOOP ( 'NONE', ( #13355, #28167, #2691, #30308 ) ) ;
#15056 = CARTESIAN_POINT ( 'NONE',  ( -35.95057207277420019, -4.776692292720859712, 14.02650114813283366 ) ) ;
#15057 = DIRECTION ( 'NONE',  ( -0.3428121700606640565, -0.6184495258776567805, 0.7071067811865474617 ) ) ;
#15058 = VERTEX_POINT ( 'NONE', #18899 ) ;
#15059 = CARTESIAN_POINT ( 'NONE',  ( 81.54161849434414933, -5.935345006353228925, 78.03023866733708758 ) ) ;
#15060 = CARTESIAN_POINT ( 'NONE',  ( -40.50146157965988891, 7.595301493077381672, 35.43807061034478778 ) ) ;
#15061 = AXIS2_PLACEMENT_3D ( 'NONE', #13886, #31927, #9445 ) ;
#15062 = CARTESIAN_POINT ( 'NONE',  ( 21.09785597605719332, -16.43545420775217281, 47.04930799450051637 ) ) ;
#15063 = DIRECTION ( 'NONE',  ( -1.101824276508909887E-16, 1.000000000000000000, -0.000000000000000000 ) ) ;
#15064 = CARTESIAN_POINT ( 'NONE',  ( 21.09785597605720042, -13.40182760052194588, -8.733904799977112887 ) ) ;
#15065 = CARTESIAN_POINT ( 'NONE',  ( 48.94625023931840246, 28.77124452788248732, 46.10640627770150246 ) ) ;
#15066 = CARTESIAN_POINT ( 'NONE',  ( -42.22138300640814634, 14.68176690255378425, 38.09144330556765112 ) ) ;
#15067 = DIRECTION ( 'NONE',  ( 0.000000000000000000, -0.000000000000000000, -1.000000000000000000 ) ) ;
#15068 = ORIENTED_EDGE ( 'NONE', *, *, #12738, .T. ) ;
#15069 = EDGE_CURVE ( 'NONE', #21033, #1586, #14321, .T. ) ;
#15070 = DIRECTION ( 'NONE',  ( -1.000000000000000000, -0.000000000000000000, -3.491481338843133355E-15 ) ) ;
#15071 = CARTESIAN_POINT ( 'NONE',  ( 21.09785597605719332, 15.43591091851533115, 47.04930799450051637 ) ) ;
#15072 = ORIENTED_EDGE ( 'NONE', *, *, #27431, .F. ) ;
#15073 = DIRECTION ( 'NONE',  ( -0.000000000000000000, -1.000000000000000000, -0.000000000000000000 ) ) ;
#15074 = ORIENTED_EDGE ( 'NONE', *, *, #22662, .T. ) ;
#15075 = AXIS2_PLACEMENT_3D ( 'NONE', #29324, #26540, #21926 ) ;
#15076 = ORIENTED_EDGE ( 'NONE', *, *, #16960, .T. ) ;
#15077 = CONICAL_SURFACE ( 'NONE', #1444, 2.923537884824412014, 0.6981317007977324574 ) ;
#15078 = VERTEX_POINT ( 'NONE', #31558 ) ;
#15079 = AXIS2_PLACEMENT_3D ( 'NONE', #25195, #7966, #3015 ) ;
#15080 = EDGE_CURVE ( 'NONE', #19002, #25278, #1673, .T. ) ;
#15081 = ADVANCED_FACE ( 'NONE', ( #28932 ), #6604, .T. ) ;
#15082 = ORIENTED_EDGE ( 'NONE', *, *, #6150, .F. ) ;
#15083 = CARTESIAN_POINT ( 'NONE',  ( 45.90820269358763994, 22.93328494799376571, 48.28896993515231628 ) ) ;
#15084 = EDGE_CURVE ( 'NONE', #16834, #14804, #16598, .T. ) ;
#15085 = ORIENTED_EDGE ( 'NONE', *, *, #11095, .F. ) ;
#15086 = DIRECTION ( 'NONE',  ( -1.101824276508909887E-16, 1.000000000000000000, -0.000000000000000000 ) ) ;
#15087 = CARTESIAN_POINT ( 'NONE',  ( 100.3079064823960493, -15.93545420775219945, 47.04930799450134771 ) ) ;
#15088 = CARTESIAN_POINT ( 'NONE',  ( -10.01019957330261256, -5.935668773294352718, -13.36321184671484552 ) ) ;
#15089 = CARTESIAN_POINT ( 'NONE',  ( 48.40186567930498285, 27.42957786121582231, 45.03923535223908203 ) ) ;
#15090 = ORIENTED_EDGE ( 'NONE', *, *, #262, .F. ) ;
#15091 = CONICAL_SURFACE ( 'NONE', #28717, 13.20000000000000995, 0.7853981633974612686 ) ;
#15092 = ORIENTED_EDGE ( 'NONE', *, *, #14464, .F. ) ;
#15093 = CARTESIAN_POINT ( 'NONE',  ( 0.6836613156275053171, 11.92558985988973497, 99.90211174246701376 ) ) ;
#15094 = TOROIDAL_SURFACE ( 'NONE', #3035, 48.63405236513555963, 2.000000000000000000 ) ;
#15095 = ORIENTED_EDGE ( 'NONE', *, *, #28088, .F. ) ;
#15096 = CARTESIAN_POINT ( 'NONE',  ( -40.47579404106498657, 7.230063580211345986, 35.21320777407684233 ) ) ;
#15097 = CARTESIAN_POINT ( 'NONE',  ( 52.99971320245913375, -5.721341737285090545, 105.3293216028873616 ) ) ;
#15098 = DIRECTION ( 'NONE',  ( -1.000000000000000000, 0.000000000000000000, 0.000000000000000000 ) ) ;
#15099 = DIRECTION ( 'NONE',  ( 0.000000000000000000, 0.8987940462991685919, 0.4383711467890740732 ) ) ;
#15100 = CARTESIAN_POINT ( 'NONE',  ( -40.80097511801616150, 8.246641009394465982, 54.64930799450051779 ) ) ;
#15101 = CONTEXT_DEPENDENT_SHAPE_REPRESENTATION ( #15808, #8761 ) ;
#15102 = ORIENTED_EDGE ( 'NONE', *, *, #10321, .F. ) ;
#15103 = ORIENTED_EDGE ( 'NONE', *, *, #5121, .T. ) ;
#15104 = CARTESIAN_POINT ( 'NONE',  ( 21.09992658989239089, 26.59184655352419568, 47.04930799450051637 ) ) ;
#15105 = CARTESIAN_POINT ( 'NONE',  ( -40.67837904183828357, 9.488261090400158082, 38.64504779057212147 ) ) ;
#15106 = CIRCLE ( 'NONE', #26616, 12.62506659569710266 ) ;
#15107 = CARTESIAN_POINT ( 'NONE',  ( -9.875810886335083083, -5.935708903123432911, 107.5270801035856039 ) ) ;
#15108 = ORIENTED_EDGE ( 'NONE', *, *, #18204, .F. ) ;
#15109 = CARTESIAN_POINT ( 'NONE',  ( 48.40186567930497574, 28.91618040159426073, 45.03923535223908203 ) ) ;
#15110 = ORIENTED_EDGE ( 'NONE', *, *, #19378, .F. ) ;
#15111 = DIRECTION ( 'NONE',  ( 0.000000000000000000, 0.000000000000000000, -1.000000000000000000 ) ) ;
#15112 = CARTESIAN_POINT ( 'NONE',  ( 21.09785597605719332, 28.56454579224779877, 47.45554698579308450 ) ) ;
#15113 = CARTESIAN_POINT ( 'NONE',  ( 21.09785597605719332, 6.574714862014670480, 47.04930799450051637 ) ) ;
#15114 = CIRCLE ( 'NONE', #32409, 12.27641737965283397 ) ;
#15115 = AXIS2_PLACEMENT_3D ( 'NONE', #13478, #1308, #13325 ) ;
#15116 = CIRCLE ( 'NONE', #25605, 0.7928932188134565351 ) ;
#15117 = ORIENTED_EDGE ( 'NONE', *, *, #12657, .F. ) ;
#15118 = CIRCLE ( 'NONE', #26092, 0.1250000000000001110 ) ;
#15119 =( BOUNDED_CURVE ( )  B_SPLINE_CURVE ( 3, ( #23414, #23090, #13417, #2748 ),
 .UNSPECIFIED., .F., .F. ) 
 B_SPLINE_CURVE_WITH_KNOTS ( ( 4, 4 ),
 ( 1.510941981261797462, 1.570796326794904774 ),
 .UNSPECIFIED. ) 
 CURVE ( )  GEOMETRIC_REPRESENTATION_ITEM ( )  RATIONAL_B_SPLINE_CURVE ( ( 1.000000000000000000, 0.9997014770583808607, 0.9997014770583808607, 1.000000000000000000 ) ) 
 REPRESENTATION_ITEM ( '' )  );
#15120 = AXIS2_PLACEMENT_3D ( 'NONE', #92, #16829, #32429 ) ;
#15121 = ORIENTED_EDGE ( 'NONE', *, *, #19747, .T. ) ;
#15122 = DIRECTION ( 'NONE',  ( 0.2756373558169974980, -0.9612616959383193382, -1.315048337272770589E-17 ) ) ;
#15123 = DIRECTION ( 'NONE',  ( -1.101824276508909887E-16, 1.000000000000000000, -0.000000000000000000 ) ) ;
#15124 = CARTESIAN_POINT ( 'NONE',  ( 48.94625023931840957, 26.05784706826093355, 46.10640627770150246 ) ) ;
#15125 = ADVANCED_FACE ( 'NONE', ( #31394 ), #30309, .T. ) ;
#15126 = AXIS2_PLACEMENT_3D ( 'NONE', #13361, #23358, #1029 ) ;
#15127 = ORIENTED_EDGE ( 'NONE', *, *, #26931, .F. ) ;
#15128 = EDGE_CURVE ( 'NONE', #18493, #22536, #16670, .T. ) ;
#15129 = CARTESIAN_POINT ( 'NONE',  ( 21.09785597605719332, 15.24673779880127356, 47.04930799450051637 ) ) ;
#15130 = DIRECTION ( 'NONE',  ( 1.000000000000000000, 0.000000000000000000, 0.000000000000000000 ) ) ;
#15131 = CARTESIAN_POINT ( 'NONE',  ( -42.48853158357926674, 14.65761848575743898, 55.12990477204974837 ) ) ;
#15132 = LINE ( 'NONE', #20046, #7731 ) ;
#15133 = CARTESIAN_POINT ( 'NONE',  ( 52.09785597605720397, 14.86454579224779948, 47.04930799450051637 ) ) ;
#15134 = DIRECTION ( 'NONE',  ( -1.101824276508909887E-16, 1.000000000000000000, -0.000000000000000000 ) ) ;
#15135 = DIRECTION ( 'NONE',  ( 1.188208965918164993E-16, 1.880121038077812639E-16, 1.000000000000000000 ) ) ;
#15136 = CARTESIAN_POINT ( 'NONE',  ( -43.95628906790246759, -0.1269931775117038586, 32.14930799450051779 ) ) ;
#15137 = FACE_OUTER_BOUND ( 'NONE', #12741, .T. ) ;
#15138 = DIRECTION ( 'NONE',  ( -0.000000000000000000, -1.000000000000000000, 0.000000000000000000 ) ) ;
#15139 = DIRECTION ( 'NONE',  ( 0.000000000000000000, 0.000000000000000000, 1.000000000000000000 ) ) ;
#15140 = ORIENTED_EDGE ( 'NONE', *, *, #29493, .T. ) ;
#15141 = ORIENTED_EDGE ( 'NONE', *, *, #1074, .F. ) ;
#15142 = CYLINDRICAL_SURFACE ( 'NONE', #10301, 2.000000000000001776 ) ;
#15143 = CIRCLE ( 'NONE', #28762, 0.1250000000000001110 ) ;
#15144 = CARTESIAN_POINT ( 'NONE',  ( 48.67890918804130251, 25.06197292877712002, 45.08320410557258384 ) ) ;
#15145 = DIRECTION ( 'NONE',  ( -1.000000000000000000, -1.101824276508909887E-16, 0.000000000000000000 ) ) ;
#15146 = AXIS2_PLACEMENT_3D ( 'NONE', #18202, #8695, #11471 ) ;
#15147 = CARTESIAN_POINT ( 'NONE',  ( 54.61603210001991471, -3.872051342217452508, 102.2906237784674204 ) ) ;
#15148 = ORIENTED_EDGE ( 'NONE', *, *, #9852, .T. ) ;
#15149 = DIRECTION ( 'NONE',  ( -1.000000000000000000, 0.000000000000000000, 0.000000000000000000 ) ) ;
#15150 = DIRECTION ( 'NONE',  ( -1.000000000000000000, 0.000000000000000000, 0.000000000000000000 ) ) ;
#15151 = CARTESIAN_POINT ( 'NONE',  ( 47.34055844982418648, 10.07270486929681752, -3.422361949332906939 ) ) ;
#15152 = EDGE_LOOP ( 'NONE', ( #30000, #23019, #28234, #10389 ) ) ;
#15153 = VERTEX_POINT ( 'NONE', #9063 ) ;
#15154 = FACE_OUTER_BOUND ( 'NONE', #30944, .T. ) ;
#15155 = CARTESIAN_POINT ( 'NONE',  ( 48.83862994770794330, 25.94118040159426641, 48.17861352429476796 ) ) ;
#15156 = CARTESIAN_POINT ( 'NONE',  ( 21.09785597605719332, 25.56454579224779877, 47.04930799450051637 ) ) ;
#15157 = VECTOR ( 'NONE', #31853, 1000.000000000000114 ) ;
#15158 = DIRECTION ( 'NONE',  ( -1.000000000000000000, 0.000000000000000000, 0.000000000000000000 ) ) ;
#15159 = DIRECTION ( 'NONE',  ( 0.000000000000000000, 0.000000000000000000, 1.000000000000000000 ) ) ;
#15160 = ORIENTED_EDGE ( 'NONE', *, *, #14489, .T. ) ;
#15161 = DIRECTION ( 'NONE',  ( 1.234978253042719660E-16, -1.000000000000000000, -1.109335647967047851E-31 ) ) ;
#15162 = VERTEX_POINT ( 'NONE', #6761 ) ;
#15163 = ADVANCED_FACE ( 'NONE', ( #17089 ), #29244, .T. ) ;
#15164 = EDGE_CURVE ( 'NONE', #6754, #20995, #9335, .T. ) ;
#15165 = EDGE_CURVE ( 'NONE', #12276, #32106, #9875, .T. ) ;
#15166 = DIRECTION ( 'NONE',  ( 0.4544104193609807552, 0.000000000000000000, 0.8907924397839137587 ) ) ;
#15167 = CARTESIAN_POINT ( 'NONE',  ( -9.728297238921257417, -5.935454207752202116, 107.4930705127871420 ) ) ;
#15168 = EDGE_CURVE ( 'NONE', #32483, #22659, #2542, .T. ) ;
#15169 = ORIENTED_EDGE ( 'NONE', *, *, #2311, .T. ) ;
#15170 = CIRCLE ( 'NONE', #3609, 37.50000000000000711 ) ;
#15171 = CARTESIAN_POINT ( 'NONE',  ( 44.79156314060809763, 22.86454579224779948, 46.92953032342011710 ) ) ;
#15172 = ORIENTED_EDGE ( 'NONE', *, *, #31027, .F. ) ;
#15173 = CARTESIAN_POINT ( 'NONE',  ( -48.34557642001920641, 3.861744873591483440, 60.54930799450051637 ) ) ;
#15174 = CARTESIAN_POINT ( 'NONE',  ( 21.09785597605720042, 11.78014697381582643, -8.546216316978195948 ) ) ;
#15175 = CIRCLE ( 'NONE', #30922, 12.62506659569710266 ) ;
#15176 = LINE ( 'NONE', #6973, #5860 ) ;
#15177 = CARTESIAN_POINT ( 'NONE',  ( 21.09785597605720753, 13.86454579224779948, 47.04930799450052348 ) ) ;
#15178 = EDGE_LOOP ( 'NONE', ( #18122, #12462, #22930, #22560 ) ) ;
#15179 = CARTESIAN_POINT ( 'NONE',  ( 73.80326597356666696, 0.5083845707908861700, 80.05401455079878303 ) ) ;
#15180 = DIRECTION ( 'NONE',  ( 0.000000000000000000, -0.000000000000000000, -1.000000000000000000 ) ) ;
#15181 = DIRECTION ( 'NONE',  ( -0.9612616959383206705, -0.2756373558169934457, 1.660411357259282938E-16 ) ) ;
#15182 = CARTESIAN_POINT ( 'NONE',  ( -40.60333149162104860, 7.557375771971046596, 59.44930799450051495 ) ) ;
#15183 = DIRECTION ( 'NONE',  ( -1.000000000000000000, 0.000000000000000000, 0.000000000000000000 ) ) ;
#15184 = EDGE_LOOP ( 'NONE', ( #13513, #14995, #10388, #20521 ) ) ;
#15185 = CARTESIAN_POINT ( 'NONE',  ( 33.46699938050304723, 25.97145308207318593, 47.04930799450050927 ) ) ;
#15186 = DIRECTION ( 'NONE',  ( 0.2756373558169942228, -0.9612616959383203374, 0.000000000000000000 ) ) ;
#15187 = VERTEX_POINT ( 'NONE', #22008 ) ;
#15188 = CYLINDRICAL_SURFACE ( 'NONE', #18330, 0.9999999999999998890 ) ;
#15189 = DIRECTION ( 'NONE',  ( 0.000000000000000000, 0.000000000000000000, 1.000000000000000000 ) ) ;
#15190 = CIRCLE ( 'NONE', #23022, 12.62506659569710266 ) ;
#15191 = VECTOR ( 'NONE', #26486, 1000.000000000000114 ) ;
#15192 = DIRECTION ( 'NONE',  ( -0.8746197071393926326, 0.4848096202463430537, 8.676864087101709653E-18 ) ) ;
#15193 = ORIENTED_EDGE ( 'NONE', *, *, #32403, .F. ) ;
#15194 = FACE_OUTER_BOUND ( 'NONE', #16908, .T. ) ;
#15195 = ORIENTED_EDGE ( 'NONE', *, *, #9078, .F. ) ;
#15196 = EDGE_CURVE ( 'NONE', #15022, #19672, #29274, .T. ) ;
#15197 = AXIS2_PLACEMENT_3D ( 'NONE', #20551, #28588, #30580 ) ;
#15198 = CIRCLE ( 'NONE', #29338, 16.00569570871410008 ) ;
#15199 = VERTEX_POINT ( 'NONE', #6444 ) ;
#15200 = AXIS2_PLACEMENT_3D ( 'NONE', #31667, #26731, #22290 ) ;
#15201 = VECTOR ( 'NONE', #18279, 1000.000000000000000 ) ;
#15202 = DIRECTION ( 'NONE',  ( -1.101824276508909887E-16, 1.000000000000000000, -0.000000000000000000 ) ) ;
#15203 = CARTESIAN_POINT ( 'NONE',  ( 21.09992658989238734, 31.96183152705962272, 47.04930799450051637 ) ) ;
#15204 = EDGE_CURVE ( 'NONE', #24463, #21157, #12254, .T. ) ;
#15205 = AXIS2_PLACEMENT_3D ( 'NONE', #13212, #17951, #2852 ) ;
#15206 = EDGE_LOOP ( 'NONE', ( #29707, #18926, #26484, #25951 ) ) ;
#15207 = ORIENTED_EDGE ( 'NONE', *, *, #17116, .F. ) ;
#15208 = CARTESIAN_POINT ( 'NONE',  ( -43.86699113690139740, -4.883519073094417351, 52.28371130614638673 ) ) ;
#15209 = CARTESIAN_POINT ( 'NONE',  ( -40.59758774925371938, 7.567737757495683226, 38.66054537865625917 ) ) ;
#15210 = CARTESIAN_POINT ( 'NONE',  ( -32.65337990276172775, 0.2376265079274789416, 80.17160938599175779 ) ) ;
#15211 = DIRECTION ( 'NONE',  ( -1.000000000000000000, 0.000000000000000000, 0.000000000000000000 ) ) ;
#15212 = EDGE_LOOP ( 'NONE', ( #28305, #5358, #23321, #9400 ) ) ;
#15213 = CARTESIAN_POINT ( 'NONE',  ( -10.48395140503805756, -5.832427868686518302, 104.6627029599396792 ) ) ;
#15214 = VERTEX_POINT ( 'NONE', #22498 ) ;
#15215 = CARTESIAN_POINT ( 'NONE',  ( -30.33993856030302894, 8.336148451382289437, 18.87414756954700934 ) ) ;
#15216 = CARTESIAN_POINT ( 'NONE',  ( 80.56633024382773556, -5.928581419070738434, 15.83468436991982919 ) ) ;
#15217 = VERTEX_POINT ( 'NONE', #7911 ) ;
#15218 = FACE_OUTER_BOUND ( 'NONE', #415, .T. ) ;
#15219 = AXIS2_PLACEMENT_3D ( 'NONE', #959, #18351, #28381 ) ;
#15220 = AXIS2_PLACEMENT_3D ( 'NONE', #19016, #28892, #1462 ) ;
#15221 = DIRECTION ( 'NONE',  ( 0.000000000000000000, -0.000000000000000000, -1.000000000000000000 ) ) ;
#15222 = LINE ( 'NONE', #19975, #14347 ) ;
#15223 = CARTESIAN_POINT ( 'NONE',  ( 46.99023568444673060, 27.83791119454915375, 49.12151524109405898 ) ) ;
#15224 = VECTOR ( 'NONE', #26141, 1000.000000000000000 ) ;
#15225 = CARTESIAN_POINT ( 'NONE',  ( -41.77464577679392477, 3.808795504615562155, 47.04930799450051637 ) ) ;
#15226 = DIRECTION ( 'NONE',  ( -0.9612616959383204485, -0.2756373558169933347, 1.660411357259282692E-16 ) ) ;
#15227 = EDGE_CURVE ( 'NONE', #1884, #286, #3562, .T. ) ;
#15228 = VERTEX_POINT ( 'NONE', #22830 ) ;
#15229 = CIRCLE ( 'NONE', #17320, 94.44530576803552435 ) ;
#15230 = AXIS2_PLACEMENT_3D ( 'NONE', #28473, #21065, #4489 ) ;
#15231 = DIRECTION ( 'NONE',  ( -0.000000000000000000, -1.000000000000000000, 0.000000000000000000 ) ) ;
#15232 = ORIENTED_EDGE ( 'NONE', *, *, #30507, .T. ) ;
#15233 = COLOUR_RGB ( '',0.7921568627450980005, 0.8196078431372548767, 0.9333333333333333481 ) ;
#15234 = EDGE_CURVE ( 'NONE', #15887, #26305, #25088, .T. ) ;
#15235 = DIRECTION ( 'NONE',  ( 0.000000000000000000, 0.000000000000000000, 1.000000000000000000 ) ) ;
#15236 = ORIENTED_EDGE ( 'NONE', *, *, #16443, .T. ) ;
#15237 = VERTEX_POINT ( 'NONE', #14645 ) ;
#15238 = CARTESIAN_POINT ( 'NONE',  ( 8.474859994195281132, 31.09184655352422411, 47.04930799450051637 ) ) ;
#15239 = EDGE_CURVE ( 'NONE', #16515, #4901, #27160, .T. ) ;
#15240 = EDGE_CURVE ( 'NONE', #24311, #9505, #23508, .T. ) ;
#15241 = EDGE_LOOP ( 'NONE', ( #23444, #26994 ) ) ;
#15242 = AXIS2_PLACEMENT_3D ( 'NONE', #21096, #3542, #13567 ) ;
#15243 = CIRCLE ( 'NONE', #23598, 12.62506659569710266 ) ;
#15244 = ORIENTED_EDGE ( 'NONE', *, *, #20256, .F. ) ;
#15245 = CIRCLE ( 'NONE', #2153, 1.142135311067127512 ) ;
#15246 = CARTESIAN_POINT ( 'NONE',  ( 46.04064016343871657, 22.98879437201065912, 48.06859758049203180 ) ) ;
#15247 = EDGE_CURVE ( 'NONE', #17931, #23918, #10367, .T. ) ;
#15248 = CIRCLE ( 'NONE', #581, 13.00178401536290806 ) ;
#15249 = VERTEX_POINT ( 'NONE', #2810 ) ;
#15250 = CARTESIAN_POINT ( 'NONE',  ( 49.25382518103883456, 29.29907168554532149, 46.06391241801129866 ) ) ;
#15251 = CARTESIAN_POINT ( 'NONE',  ( -9.880269303432736905, -5.935454207752200340, -13.45870566634170018 ) ) ;
#15252 = CARTESIAN_POINT ( 'NONE',  ( 49.49063479933183629, 27.31291119454915517, 47.17357720316391578 ) ) ;
#15253 = ORIENTED_EDGE ( 'NONE', *, *, #22624, .T. ) ;
#15254 = ORIENTED_EDGE ( 'NONE', *, *, #5274, .T. ) ;
#15255 = DIRECTION ( 'NONE',  ( -1.000000000000000000, 0.000000000000000000, 0.000000000000000000 ) ) ;
#15256 = TOROIDAL_SURFACE ( 'NONE', #5313, 12.40141737965288904, 0.1249999999999998612 ) ;
#15257 = ORIENTED_EDGE ( 'NONE', *, *, #12349, .T. ) ;
#15258 = CARTESIAN_POINT ( 'NONE',  ( 8.823575513742486720, 34.59164230456639899, 47.37072134000479906 ) ) ;
#15259 = FACE_OUTER_BOUND ( 'NONE', #3277, .T. ) ;
#15260 = CARTESIAN_POINT ( 'NONE',  ( 21.09992658989238734, 30.84143805560860585, 47.04930799450051637 ) ) ;
#15261 = DIRECTION ( 'NONE',  ( -0.000000000000000000, -1.000000000000000000, 0.000000000000000000 ) ) ;
#15262 = CARTESIAN_POINT ( 'NONE',  ( 49.49063479933183629, 25.21291119454915730, 47.17357720316391578 ) ) ;
#15263 = EDGE_CURVE ( 'NONE', #22659, #7408, #28228, .T. ) ;
#15264 = ORIENTED_EDGE ( 'NONE', *, *, #7123, .T. ) ;
#15265 = ORIENTED_EDGE ( 'NONE', *, *, #4625, .F. ) ;
#15266 = CYLINDRICAL_SURFACE ( 'NONE', #27587, 1.042135311067126979 ) ;
#15267 = CYLINDRICAL_SURFACE ( 'NONE', #16636, 12.36707279061065101 ) ;
#15268 = EDGE_CURVE ( 'NONE', #26, #6039, #24019, .T. ) ;
#15269 = DIRECTION ( 'NONE',  ( 0.000000000000000000, 0.000000000000000000, 1.000000000000000000 ) ) ;
#15270 = ORIENTED_EDGE ( 'NONE', *, *, #17488, .F. ) ;
#15271 = CARTESIAN_POINT ( 'NONE',  ( 45.24946171279598417, 29.20784706826092503, 47.99220971130007030 ) ) ;
#15272 = TOROIDAL_SURFACE ( 'NONE', #1101, 1.299999999999999822, 0.1000000000000000056 ) ;
#15273 = ORIENTED_EDGE ( 'NONE', *, *, #11386, .T. ) ;
#15274 = DIRECTION ( 'NONE',  ( -0.8746197071393926326, 0.4848096202463430537, 8.676864087101709653E-18 ) ) ;
#15275 = CIRCLE ( 'NONE', #26276, 0.1999999999999987899 ) ;
#15276 = DIRECTION ( 'NONE',  ( -1.000000000000000000, 0.000000000000000000, 0.000000000000000000 ) ) ;
#15277 = CLOSED_SHELL ( 'NONE', ( #16789, #5447, #9821, #2926, #18650, #27720, #15753, #8538, #1356, #16591, #5629, #21206, #26853, #1593, #12739, #12879, #25120, #25306, #3339, #15760, #13074, #32097, #16922, #5955, #18244, #3710, #2523, #3438, #6193, #31506, #16014, #16631, #18160, #2036, #6485, #10652, #18984, #24344, #18291, #1515, #5233, #2445, #1656, #17975, #13559, #22082, #19182, #25450, #30392, #23201, #24341, #20439, #2638, #18768, #16808, #29310, #30098, #9630, #26044, #23495, #12312, #14073, #6250 ) ) ;
#15278 = AXIS2_PLACEMENT_3D ( 'NONE', #9812, #22271, #19974 ) ;
#15279 = EDGE_CURVE ( 'NONE', #10069, #22139, #14590, .T. ) ;
#15280 = LINE ( 'NONE', #8061, #29606 ) ;
#15281 = EDGE_CURVE ( 'NONE', #8039, #25543, #22693, .T. ) ;
#15282 = AXIS2_PLACEMENT_3D ( 'NONE', #21777, #31484, #26230 ) ;
#15283 = ORIENTED_EDGE ( 'NONE', *, *, #18, .F. ) ;
#15284 = ORIENTED_EDGE ( 'NONE', *, *, #23936, .T. ) ;
#15285 = CARTESIAN_POINT ( 'NONE',  ( 21.09785597605719332, 25.56454579224779877, 47.04930799450051637 ) ) ;
#15286 = ORIENTED_EDGE ( 'NONE', *, *, #28012, .T. ) ;
#15287 = VECTOR ( 'NONE', #6167, 1000.000000000000000 ) ;
#15288 = CARTESIAN_POINT ( 'NONE',  ( -38.65545646816406133, -0.7885532610349046401, 80.71350123316483405 ) ) ;
#15289 = CIRCLE ( 'NONE', #22619, 1.500000000000001332 ) ;
#15290 = DIRECTION ( 'NONE',  ( -0.000000000000000000, -1.000000000000000000, 0.000000000000000000 ) ) ;
#15291 = DIRECTION ( 'NONE',  ( 0.8746197071393926326, -0.4848096202463430537, -8.676864087101709653E-18 ) ) ;
#15292 = TOROIDAL_SURFACE ( 'NONE', #23673, 54.10000000000000142, 0.1999999999999994282 ) ;
#15293 = CARTESIAN_POINT ( 'NONE',  ( 44.87087493598345134, 26.07587066347689486, 48.18533415931919706 ) ) ;
#15294 = CARTESIAN_POINT ( 'NONE',  ( 47.09785597605719687, 24.76454579224779806, 47.04930799450078638 ) ) ;
#15295 = FACE_OUTER_BOUND ( 'NONE', #26872, .T. ) ;
#15296 = PLANE ( 'NONE',  #7465 ) ;
#15297 = CARTESIAN_POINT ( 'NONE',  ( 45.40326095744675428, 22.93807716476589675, 47.12319401418537268 ) ) ;
#15298 = DIRECTION ( 'NONE',  ( 0.000000000000000000, 0.000000000000000000, 1.000000000000000000 ) ) ;
#15299 = LINE ( 'NONE', #17590, #28835 ) ;
#15300 = ADVANCED_FACE ( 'NONE', ( #17419 ), #5285, .T. ) ;
#15301 = CARTESIAN_POINT ( 'NONE',  ( 21.09785597605719332, 30.36454579224779238, 34.04930799450050927 ) ) ;
#15302 = SHAPE_REPRESENTATION_RELATIONSHIP ( 'NONE' , 'NONE' ,  #21423, #8462 ) ;
#15303 = ORIENTED_EDGE ( 'NONE', *, *, #15080, .T. ) ;
#15304 = EDGE_LOOP ( 'NONE', ( #16226, #5532, #164, #21882 ) ) ;
#15305 = CYLINDRICAL_SURFACE ( 'NONE', #26497, 12.36707279061065279 ) ;
#15306 = AXIS2_PLACEMENT_3D ( 'NONE', #3054, #15868, #17835 ) ;
#15307 = CARTESIAN_POINT ( 'NONE',  ( 33.71785032049132980, 29.21664230456640254, 47.04930799450051637 ) ) ;
#15308 = CARTESIAN_POINT ( 'NONE',  ( -35.68407394989286985, -5.326758346624735019, 14.55639542095637751 ) ) ;
#15309 = DIRECTION ( 'NONE',  ( 1.000000000000000000, 0.000000000000000000, -1.224646799147353207E-16 ) ) ;
#15310 = ORIENTED_EDGE ( 'NONE', *, *, #848, .T. ) ;
#15311 = CARTESIAN_POINT ( 'NONE',  ( -39.48078212898874995, -5.935481998376881840, 77.98349214134881890 ) ) ;
#15312 = DIRECTION ( 'NONE',  ( -1.000000000000000000, -1.101824276508910010E-16, 0.000000000000000000 ) ) ;
#15313 = CARTESIAN_POINT ( 'NONE',  ( 21.09992658989238734, 38.56284415653841791, 47.04930799450051637 ) ) ;
#15314 = ORIENTED_EDGE ( 'NONE', *, *, #26002, .T. ) ;
#15315 = ORIENTED_EDGE ( 'NONE', *, *, #21512, .F. ) ;
#15316 = CARTESIAN_POINT ( 'NONE',  ( 48.94625023931840957, 26.05784706826093355, 46.10640627770150246 ) ) ;
#15317 = CARTESIAN_POINT ( 'NONE',  ( -9.472371843582571671, 5.388785998227650254, -3.351769630585352377 ) ) ;
#15318 = EDGE_CURVE ( 'NONE', #27142, #30184, #14070, .T. ) ;
#15319 = DIRECTION ( 'NONE',  ( -1.000000000000000000, 0.000000000000000000, 0.000000000000000000 ) ) ;
#15320 = AXIS2_PLACEMENT_3D ( 'NONE', #877, #8438, #18431 ) ;
#15321 = CARTESIAN_POINT ( 'NONE',  ( 21.09992658989238734, 31.97145308207317171, 47.04930799450051637 ) ) ;
#15322 = AXIS2_PLACEMENT_3D ( 'NONE', #3503, #5984, #3350 ) ;
#15323 = ORIENTED_EDGE ( 'NONE', *, *, #28209, .F. ) ;
#15324 = CIRCLE ( 'NONE', #30516, 1.003191532947550701 ) ;
#15325 = ORIENTED_EDGE ( 'NONE', *, *, #1174, .T. ) ;
#15326 = CIRCLE ( 'NONE', #18974, 12.62506659569710266 ) ;
#15327 = CARTESIAN_POINT ( 'NONE',  ( 21.09785597605720753, 13.61454579224779771, 47.04930799450052348 ) ) ;
#15328 = PRODUCT_RELATED_PRODUCT_CATEGORY ( 'part', '', ( #3299 ) ) ;
#15329 = DIRECTION ( 'NONE',  ( 0.2756373558170082672, -0.9612616959383162296, 6.938893903907184201E-14 ) ) ;
#15330 = B_SPLINE_CURVE_WITH_KNOTS ( 'NONE', 3,
 ( #31722, #9235, #19063, #19223, #29248, #19395, #29586, #31563, #7093, #6931, #4797, #26951, #24322, #29747, #6767, #22015, #27113, #27277, #9396, #16768, #29092, #31879, #7262, #6610, #21527, #19720, #14815, #32047, #9562, #19557, #14652, #16602, #26623, #1842 ),
 .UNSPECIFIED., .F., .F.,
 ( 4, 2, 2, 2, 2, 2, 2, 2, 2, 2, 2, 2, 2, 2, 2, 2, 4 ),
 ( 0.5000000000000000000, 0.5312500000000000000, 0.5625000000000000000, 0.5937500000000000000, 0.6250000000000000000, 0.6562500000000000000, 0.6875000000000000000, 0.7187500000000000000, 0.7500000000000000000, 0.7812500000000000000, 0.8125000000000000000, 0.8437500000000000000, 0.8750000000000000000, 0.9062500000000000000, 0.9375000000000000000, 0.9687500000000000000, 1.000000000000000000 ),
 .UNSPECIFIED. ) ;
#15331 = CIRCLE ( 'NONE', #25293, 0.1250000000000001110 ) ;
#15332 = VERTEX_POINT ( 'NONE', #32205 ) ;
#15333 = EDGE_LOOP ( 'NONE', ( #4421, #17829, #13183, #29276 ) ) ;
#15334 = DIRECTION ( 'NONE',  ( -1.000000000000000000, 0.000000000000000000, 0.000000000000000000 ) ) ;
#15335 = DIRECTION ( 'NONE',  ( -1.224646799147353207E-16, 0.000000000000000000, -1.000000000000000000 ) ) ;
#15336 = CIRCLE ( 'NONE', #30531, 1.000000000000000888 ) ;
#15337 = CARTESIAN_POINT ( 'NONE',  ( 33.72499318558949000, 38.56284415653841791, 47.04930799450051637 ) ) ;
#15338 = CARTESIAN_POINT ( 'NONE',  ( 45.29931651390019454, 22.86454579224779948, 47.92489232862990889 ) ) ;
#15339 = VERTEX_POINT ( 'NONE', #9721 ) ;
#15340 = CARTESIAN_POINT ( 'NONE',  ( 45.96182992765471909, 27.87822092656774586, 44.82232689504102296 ) ) ;
#15341 = CARTESIAN_POINT ( 'NONE',  ( -9.943725601011752957, -5.936969727347462644, -13.57595196341301858 ) ) ;
#15342 = DIRECTION ( 'NONE',  ( 0.9612616959383200044, 0.2756373558169954996, -1.660411357259285896E-16 ) ) ;
#15343 = LINE ( 'NONE', #23213, #18894 ) ;
#15344 = CARTESIAN_POINT ( 'NONE',  ( 21.09785597605719332, 17.56454579224779877, -1.926157182631158093 ) ) ;
#15345 = EDGE_LOOP ( 'NONE', ( #28180, #13911, #1835, #27166 ) ) ;
#15346 = CARTESIAN_POINT ( 'NONE',  ( 21.09992658989239089, 24.46183152705960140, 47.04930799450051637 ) ) ;
#15347 = ORIENTED_EDGE ( 'NONE', *, *, #24297, .T. ) ;
#15348 = CARTESIAN_POINT ( 'NONE',  ( -43.38408989745150990, 1.111547985471240674, 53.54930799450051637 ) ) ;
#15349 = DIRECTION ( 'NONE',  ( 0.000000000000000000, -0.000000000000000000, -1.000000000000000000 ) ) ;
#15350 = CARTESIAN_POINT ( 'NONE',  ( -29.27337757263006424, -5.906256089375805374, 15.45647446568822225 ) ) ;
#15351 = ADVANCED_FACE ( 'NONE', ( #7255 ), #22683, .T. ) ;
#15352 = DIRECTION ( 'NONE',  ( 0.000000000000000000, -0.000000000000000000, -1.000000000000000000 ) ) ;
#15353 = ADVANCED_FACE ( 'NONE', ( #27271 ), #19876, .T. ) ;
#15354 = EDGE_CURVE ( 'NONE', #9336, #18648, #26749, .T. ) ;
#15355 = AXIS2_PLACEMENT_3D ( 'NONE', #17708, #27733, #806 ) ;
#15356 = ORIENTED_EDGE ( 'NONE', *, *, #9260, .T. ) ;
#15357 = B_SPLINE_SURFACE_WITH_KNOTS ( 'NONE', 3, 1, ( 
 ( #24342, #28787 ),
 ( #6954, #6469 ),
 ( #1372, #11389 ),
 ( #29275, #24505 ),
 ( #24180, #6789 ),
 ( #16949, #26973 ) ),
 .UNSPECIFIED., .F., .F., .F.,
 ( 4, 1, 1, 4 ),
 ( 2, 2 ),
 ( 0.1800733115436725096, 0.4989925988945991819, 0.7849997004460342875, 1.000000000000000000 ),
 ( 0.000000000000000000, 1.000000000000000000 ),
 .UNSPECIFIED. ) ;
#15358 = EDGE_CURVE ( 'NONE', #10259, #11316, #9878, .T. ) ;
#15359 = DIRECTION ( 'NONE',  ( -0.1949050434465282311, 0.6797146636928673713, -0.7071067811865470176 ) ) ;
#15360 = ORIENTED_EDGE ( 'NONE', *, *, #30020, .F. ) ;
#15361 = EDGE_CURVE ( 'NONE', #10568, #23541, #14303, .T. ) ;
#15362 = VECTOR ( 'NONE', #22628, 1000.000000000000000 ) ;
#15363 = ORIENTED_EDGE ( 'NONE', *, *, #28402, .F. ) ;
#15364 = AXIS2_PLACEMENT_3D ( 'NONE', #2717, #15352, #30461 ) ;
#15365 = CARTESIAN_POINT ( 'NONE',  ( -9.875059786958400920, -5.935668157269682332, 107.6366642019984567 ) ) ;
#15366 = FACE_OUTER_BOUND ( 'NONE', #1702, .T. ) ;
#15367 = ORIENTED_EDGE ( 'NONE', *, *, #15849, .F. ) ;
#15368 = VERTEX_POINT ( 'NONE', #21161 ) ;
#15369 = AXIS2_PLACEMENT_3D ( 'NONE', #16653, #1238, #9119 ) ;
#15370 = FACE_OUTER_BOUND ( 'NONE', #8210, .T. ) ;
#15371 = LINE ( 'NONE', #25379, #18565 ) ;
#15372 = CARTESIAN_POINT ( 'NONE',  ( 21.09992658989238734, 31.59164230456639544, 47.04930799450051637 ) ) ;
#15373 = AXIS2_PLACEMENT_3D ( 'NONE', #16523, #21768, #16362 ) ;
#15374 = DIRECTION ( 'NONE',  ( 0.03087013654144268177, -0.1076569600579695002, -0.9937087166876366062 ) ) ;
#15375 = EDGE_CURVE ( 'NONE', #14267, #4827, #5916, .T. ) ;
#15376 = ORIENTED_EDGE ( 'NONE', *, *, #31944, .F. ) ;
#15377 = CARTESIAN_POINT ( 'NONE',  ( -11.87686653301373241, -4.853532562205602474, 103.2493967191210373 ) ) ;
#15378 = ORIENTED_EDGE ( 'NONE', *, *, #1359, .F. ) ;
#15379 = CARTESIAN_POINT ( 'NONE',  ( -32.97970629999527858, -0.5268592320365600434, 13.64887994798114512 ) ) ;
#15380 = CARTESIAN_POINT ( 'NONE',  ( -6.282007179091762872, 9.127627432390735152, -3.410470909561460928 ) ) ;
#15381 = ORIENTED_EDGE ( 'NONE', *, *, #15814, .T. ) ;
#15382 = CARTESIAN_POINT ( 'NONE',  ( 47.13599827484107863, 23.09557481883486929, 46.31488638136413272 ) ) ;
#15383 = CARTESIAN_POINT ( 'NONE',  ( 21.09785597605718621, 77.37241625295546044, 47.04930799450051637 ) ) ;
#15384 = DIRECTION ( 'NONE',  ( -0.8746197071393926326, 0.4848096202463430537, 8.676864087101709653E-18 ) ) ;
#15385 = DIRECTION ( 'NONE',  ( 0.000000000000000000, -0.000000000000000000, -1.000000000000000000 ) ) ;
#15386 = CARTESIAN_POINT ( 'NONE',  ( 44.70507715278255745, 29.06291119454914806, 46.92503878583764987 ) ) ;
#15387 = AXIS2_PLACEMENT_3D ( 'NONE', #7117, #61, #30105 ) ;
#15388 = AXIS2_PLACEMENT_3D ( 'NONE', #2266, #7185, #2096 ) ;
#15389 = DIRECTION ( 'NONE',  ( 7.588956326749211550E-18, -4.206627182996911684E-18, 1.000000000000000000 ) ) ;
#15390 = CARTESIAN_POINT ( 'NONE',  ( 21.09785597605720753, 13.86454579224779948, 47.04930799450052348 ) ) ;
#15391 = ORIENTED_EDGE ( 'NONE', *, *, #18490, .F. ) ;
#15392 = CARTESIAN_POINT ( 'NONE',  ( 21.09992658989239089, 29.47145308207317882, 47.04930799450051637 ) ) ;
#15393 = ORIENTED_EDGE ( 'NONE', *, *, #28684, .F. ) ;
#15394 = CARTESIAN_POINT ( 'NONE',  ( -43.69495677161796010, 1.169528900831203311, 60.54930799450051637 ) ) ;
#15395 = ADVANCED_FACE ( 'NONE', ( #20849 ), #5444, .T. ) ;
#15396 = VERTEX_POINT ( 'NONE', #12998 ) ;
#15397 = EDGE_CURVE ( 'NONE', #27983, #16490, #20570, .T. ) ;
#15398 = EDGE_LOOP ( 'NONE', ( #4735, #11940, #15381, #2519 ) ) ;
#15399 = DIRECTION ( 'NONE',  ( 0.000000000000000000, 0.000000000000000000, -1.000000000000000000 ) ) ;
#15400 = EDGE_CURVE ( 'NONE', #7489, #15932, #13160, .T. ) ;
#15401 = ORIENTED_EDGE ( 'NONE', *, *, #5389, .F. ) ;
#15402 = AXIS2_PLACEMENT_3D ( 'NONE', #18789, #21098, #3708 ) ;
#15403 = AXIS2_PLACEMENT_3D ( 'NONE', #20260, #17963, #30288 ) ;
#15404 = AXIS2_PLACEMENT_3D ( 'NONE', #28749, #21679, #19207 ) ;
#15405 = ORIENTED_EDGE ( 'NONE', *, *, #11937, .F. ) ;
#15406 = DIRECTION ( 'NONE',  ( 2.779292025043186357E-18, -1.288349127009862211E-17, 1.000000000000000000 ) ) ;
#15407 = ORIENTED_EDGE ( 'NONE', *, *, #20700, .T. ) ;
#15408 = DIRECTION ( 'NONE',  ( 0.1949050434465268156, -0.6797146636928678154, -0.7071067811865469066 ) ) ;
#15409 = DIRECTION ( 'NONE',  ( 0.2756373558169973870, -0.9612616959383193382, -1.315048337272770435E-17 ) ) ;
#15410 = CARTESIAN_POINT ( 'NONE',  ( 47.20547626766766314, 26.78791119454915659, 44.97710074790751378 ) ) ;
#15411 = ADVANCED_FACE ( 'NONE', ( #11016, #30718 ), #25463, .T. ) ;
#15412 = EDGE_LOOP ( 'NONE', ( #7716, #28635, #6098, #17558 ) ) ;
#15413 = EDGE_LOOP ( 'NONE', ( #1033, #21416, #5825, #8587 ) ) ;
#15414 = DIRECTION ( 'NONE',  ( 1.234978253042719660E-16, -1.000000000000000000, -1.109335647967047851E-31 ) ) ;
#15415 = EDGE_CURVE ( 'NONE', #1311, #13866, #18696, .T. ) ;
#15416 = VERTEX_POINT ( 'NONE', #21004 ) ;
#15417 = DIRECTION ( 'NONE',  ( 0.000000000000000000, -1.000000000000000000, 0.000000000000000000 ) ) ;
#15418 = DIRECTION ( 'NONE',  ( -1.000000000000000000, 0.000000000000000000, 0.000000000000000000 ) ) ;
#15419 = CARTESIAN_POINT ( 'NONE',  ( -40.68879370032182408, 6.799057175545497600, 34.73625888416037810 ) ) ;
#15420 = CIRCLE ( 'NONE', #5997, 2.499999999999998668 ) ;
#15421 = CARTESIAN_POINT ( 'NONE',  ( 8.474859994195281132, 38.56284415653841791, 47.04930799450051637 ) ) ;
#15422 = CARTESIAN_POINT ( 'NONE',  ( 48.53603344299159517, 25.12750526699945297, 48.64505250420380378 ) ) ;
#15423 = SHAPE_DEFINITION_REPRESENTATION ( #27115, #5723 ) ;
#15424 = ORIENTED_EDGE ( 'NONE', *, *, #30522, .T. ) ;
#15425 = DIRECTION ( 'NONE',  ( -1.000000000000000000, 0.000000000000000000, 0.000000000000000000 ) ) ;
#15426 = CARTESIAN_POINT ( 'NONE',  ( 21.09785597605719332, -6.704410789454799513, 47.04930799450051637 ) ) ;
#15427 = CARTESIAN_POINT ( 'NONE',  ( 48.83862994770794330, 28.74118040159426002, 48.17861352429476796 ) ) ;
#15428 = ORIENTED_EDGE ( 'NONE', *, *, #25972, .T. ) ;
#15429 = CYLINDRICAL_SURFACE ( 'NONE', #9926, 12.62506659569710266 ) ;
#15430 = CARTESIAN_POINT ( 'NONE',  ( -0.9021440239427910290, 13.86454579224779948, 47.04930799450052348 ) ) ;
#15431 = EDGE_CURVE ( 'NONE', #110, #32358, #10535, .T. ) ;
#15432 = DIRECTION ( 'NONE',  ( 0.2756373558169973870, -0.9612616959383193382, -1.315048337272770280E-17 ) ) ;
#15433 = VERTEX_POINT ( 'NONE', #8548 ) ;
#15434 = AXIS2_PLACEMENT_3D ( 'NONE', #23194, #28286, #5806 ) ;
#15435 = CIRCLE ( 'NONE', #21184, 12.36707279061065101 ) ;
#15436 = ORIENTED_EDGE ( 'NONE', *, *, #13239, .F. ) ;
#15437 = EDGE_CURVE ( 'NONE', #13254, #31739, #16911, .T. ) ;
#15438 = AXIS2_PLACEMENT_3D ( 'NONE', #17825, #5198, #12597 ) ;
#15439 = DIRECTION ( 'NONE',  ( 0.4848096202463430537, 0.8746197071393926326, -1.125439520643636483E-16 ) ) ;
#15440 = CARTESIAN_POINT ( 'NONE',  ( -40.65487266620045403, 9.475231293617264683, 35.46144002885649371 ) ) ;
#15442 = CARTESIAN_POINT ( 'NONE',  ( -58.11219453028166981, 25.56454579224780232, 47.04930799450023926 ) ) ;
#15441 = CIRCLE ( 'NONE', #14422, 54.10000000000000142 ) ;
#15443 = AXIS2_PLACEMENT_3D ( 'NONE', #25445, #2798, #12824 ) ;
#15444 = EDGE_CURVE ( 'NONE', #14982, #21567, #21104, .T. ) ;
#15445 = AXIS2_PLACEMENT_3D ( 'NONE', #30553, #15439, #17733 ) ;
#15446 = ORIENTED_EDGE ( 'NONE', *, *, #6155, .T. ) ;
#15447 = CARTESIAN_POINT ( 'NONE',  ( -38.65545646816406133, -5.952175616702188421, 78.54874598263256757 ) ) ;
#15448 = DIRECTION ( 'NONE',  ( 3.551608010268815105E-15, 0.000000000000000000, 1.000000000000000000 ) ) ;
#15449 = DIRECTION ( 'NONE',  ( 0.000000000000000000, -0.000000000000000000, -1.000000000000000000 ) ) ;
#15450 = EDGE_CURVE ( 'NONE', #11333, #20809, #24239, .T. ) ;
#15451 = CARTESIAN_POINT ( 'NONE',  ( 21.09992658989238734, 38.56284415653841791, 47.04930799450051637 ) ) ;
#15452 = ADVANCED_FACE ( 'NONE', ( #10856 ), #10118, .F. ) ;
#15453 = EDGE_CURVE ( 'NONE', #18652, #28622, #22163, .T. ) ;
#15454 = LINE ( 'NONE', #17258, #9094 ) ;
#15455 = DIRECTION ( 'NONE',  ( 0.4848096202463424431, 0.8746197071393927436, -2.220446049250312588E-16 ) ) ;
#15456 = CARTESIAN_POINT ( 'NONE',  ( 52.07598125554711999, -5.935454207752202116, 132.0493079945005377 ) ) ;
#15457 = CYLINDRICAL_SURFACE ( 'NONE', #1573, 39.49999999999999289 ) ;
#15458 = CARTESIAN_POINT ( 'NONE',  ( 44.91142894931555674, 28.69787913140503832, 45.63089057098605394 ) ) ;
#15459 = PRESENTATION_STYLE_ASSIGNMENT (( #29923 ) ) ;
#15460 = ORIENTED_EDGE ( 'NONE', *, *, #29829, .F. ) ;
#15461 = ORIENTED_EDGE ( 'NONE', *, *, #13826, .F. ) ;
#15462 = DIRECTION ( 'NONE',  ( 0.2756373558169961102, -0.9612616959383197823, 0.000000000000000000 ) ) ;
#15463 = FACE_OUTER_BOUND ( 'NONE', #27676, .T. ) ;
#15464 = DIRECTION ( 'NONE',  ( -1.101824276508909887E-16, 1.000000000000000000, -0.000000000000000000 ) ) ;
#15465 = CIRCLE ( 'NONE', #19618, 0.1250000000000001110 ) ;
#15466 = EDGE_LOOP ( 'NONE', ( #16493, #2617, #18514, #14466 ) ) ;
#15467 = CARTESIAN_POINT ( 'NONE',  ( -39.52346957204299827, -5.935776016422421364, 77.96988935039777857 ) ) ;
#15468 = CARTESIAN_POINT ( 'NONE',  ( -40.22853490217745076, 6.951940700334886536, 39.38237851325574468 ) ) ;
#15469 = VERTEX_POINT ( 'NONE', #8074 ) ;
#15470 = ORIENTED_EDGE ( 'NONE', *, *, #15444, .T. ) ;
#15472 = AXIS2_PLACEMENT_3D ( 'NONE', #25942, #13164, #10540 ) ;
#15471 = CARTESIAN_POINT ( 'NONE',  ( 21.09785597605719332, -5.986312001188950127, -20.31486511684154550 ) ) ;
#15473 = CARTESIAN_POINT ( 'NONE',  ( 46.99023568444673060, 27.92451373492759714, 49.12151524109405898 ) ) ;
#15474 = EDGE_CURVE ( 'NONE', #15199, #20144, #18978, .T. ) ;
#15475 = AXIS2_PLACEMENT_3D ( 'NONE', #16816, #26838, #4354 ) ;
#15476 = AXIS2_PLACEMENT_3D ( 'NONE', #2701, #23036, #724 ) ;
#15477 = CARTESIAN_POINT ( 'NONE',  ( 48.18662509608405031, 28.59624452788247950, 49.18364984542562013 ) ) ;
#15478 = DIRECTION ( 'NONE',  ( -0.000000000000000000, -0.000000000000000000, 1.000000000000000000 ) ) ;
#15479 = CIRCLE ( 'NONE', #13880, 19.50000000000000000 ) ;
#15480 = VERTEX_POINT ( 'NONE', #25621 ) ;
#15481 = EDGE_CURVE ( 'NONE', #29530, #20511, #6425, .T. ) ;
#15482 = CARTESIAN_POINT ( 'NONE',  ( 21.09992658989239089, 26.34164230456639899, 47.04930799450051637 ) ) ;
#15483 = EDGE_CURVE ( 'NONE', #32242, #27103, #29492, .T. ) ;
#15484 = ORIENTED_EDGE ( 'NONE', *, *, #3031, .F. ) ;
#15485 = AXIS2_PLACEMENT_3D ( 'NONE', #635, #20492, #20318 ) ;
#15486 = LINE ( 'NONE', #28448, #20147 ) ;
#15487 = DIRECTION ( 'NONE',  ( 0.9612616959383194493, 0.2756373558169974980, 8.795445018804946186E-19 ) ) ;
#15488 = VECTOR ( 'NONE', #24949, 1000.000000000000000 ) ;
#15489 = AXIS2_PLACEMENT_3D ( 'NONE', #21698, #24325, #4475 ) ;
#15490 = AXIS2_PLACEMENT_3D ( 'NONE', #15177, #12731, #27817 ) ;
#15491 = ADVANCED_FACE ( 'NONE', ( #9354 ), #11979, .T. ) ;
#15492 = ORIENTED_EDGE ( 'NONE', *, *, #22968, .T. ) ;
#15493 = CYLINDRICAL_SURFACE ( 'NONE', #19081, 0.1000000000000006301 ) ;
#15494 = CIRCLE ( 'NONE', #23871, 12.27641737965280200 ) ;
#15495 = EDGE_CURVE ( 'NONE', #28351, #16288, #16158, .T. ) ;
#15496 = DIRECTION ( 'NONE',  ( -0.2756373558169973870, 0.9612616959383193382, 1.315048337272770280E-17 ) ) ;
#15497 = LINE ( 'NONE', #25824, #20958 ) ;
#15498 = CARTESIAN_POINT ( 'NONE',  ( 0.6836613156275053171, 11.92558985988973497, -4.944603100128008855 ) ) ;
#15499 = CARTESIAN_POINT ( 'NONE',  ( -40.69234404896523216, 6.790679892791737338, 39.46310372540604305 ) ) ;
#15500 = ORIENTED_EDGE ( 'NONE', *, *, #3631, .F. ) ;
#15501 = CARTESIAN_POINT ( 'NONE',  ( 74.68627032013220912, -1.428409478025942425, 80.66670155429770261 ) ) ;
#15502 = CARTESIAN_POINT ( 'NONE',  ( 33.50134396954528171, 23.59164230456639544, 47.04930799450051637 ) ) ;
#15503 = DIRECTION ( 'NONE',  ( -1.101824276508909887E-16, 1.000000000000000000, -0.000000000000000000 ) ) ;
#15504 = DIRECTION ( 'NONE',  ( -1.000000000000000000, 0.000000000000000000, 0.000000000000000000 ) ) ;
#15505 = VECTOR ( 'NONE', #23636, 1000.000000000000000 ) ;
#15506 = DIRECTION ( 'NONE',  ( 1.000000000000000000, 0.000000000000000000, 0.000000000000000000 ) ) ;
#15507 = ORIENTED_EDGE ( 'NONE', *, *, #9440, .F. ) ;
#15508 = DIRECTION ( 'NONE',  ( -1.000000000000000000, 0.000000000000000000, 0.000000000000000000 ) ) ;
#15509 = DIRECTION ( 'NONE',  ( 0.000000000000000000, 0.000000000000000000, -1.000000000000000000 ) ) ;
#15510 = VERTEX_POINT ( 'NONE', #16719 ) ;
#15511 = DIRECTION ( 'NONE',  ( 1.234978253042719660E-16, -1.000000000000000000, -1.109335647967047851E-31 ) ) ;
#15512 = CARTESIAN_POINT ( 'NONE',  ( -38.41701585771487260, 6.978388747684010518, 62.04930799450052348 ) ) ;
#15513 = CARTESIAN_POINT ( 'NONE',  ( 48.40423897560355471, 29.16454579224780019, 44.91779129072006072 ) ) ;
#15514 = CARTESIAN_POINT ( 'NONE',  ( 54.18094237054272355, -4.708525186292121134, -9.920763639972056680 ) ) ;
#15515 = ORIENTED_EDGE ( 'NONE', *, *, #16960, .F. ) ;
#15516 = CARTESIAN_POINT ( 'NONE',  ( 48.74539165043771760, 22.91413368675619111, 47.78185833695556539 ) ) ;
#15517 = ORIENTED_EDGE ( 'NONE', *, *, #27838, .T. ) ;
#15518 = CIRCLE ( 'NONE', #3465, 2.500000000000002220 ) ;
#15519 = VERTEX_POINT ( 'NONE', #18860 ) ;
#15520 = AXIS2_PLACEMENT_3D ( 'NONE', #11395, #18933, #26500 ) ;
#15521 = CARTESIAN_POINT ( 'NONE',  ( -41.02113223168485234, 7.230835263863471418, 34.64930799450051779 ) ) ;
#15522 = LINE ( 'NONE', #12756, #14709 ) ;
#15523 = EDGE_CURVE ( 'NONE', #30456, #1224, #27394, .T. ) ;
#15524 = ORIENTED_EDGE ( 'NONE', *, *, #13751, .T. ) ;
#15525 = EDGE_LOOP ( 'NONE', ( #15031, #4703, #30731, #13522 ) ) ;
#15526 = EDGE_CURVE ( 'NONE', #8522, #5457, #21608, .T. ) ;
#15527 = CARTESIAN_POINT ( 'NONE',  ( 46.81682104422132085, 23.12036939723557083, 47.03471240234085116 ) ) ;
#15528 = CARTESIAN_POINT ( 'NONE',  ( 33.50134396954527460, 24.34164230456639544, 47.04930799450051637 ) ) ;
#15529 = DIRECTION ( 'NONE',  ( -1.101824276508909887E-16, 1.000000000000000000, -0.000000000000000000 ) ) ;
#15530 = CARTESIAN_POINT ( 'NONE',  ( 21.09785597605719332, 47.56454579224779877, 65.91126043309506599 ) ) ;
#15531 = ORIENTED_EDGE ( 'NONE', *, *, #29086, .T. ) ;
#15532 = CARTESIAN_POINT ( 'NONE',  ( -12.19700416223893313, -0.2653311271195798460, 100.0789975867371169 ) ) ;
#15533 = ORIENTED_EDGE ( 'NONE', *, *, #9626, .F. ) ;
#15534 = DIRECTION ( 'NONE',  ( 0.000000000000000000, 1.000000000000000000, -0.000000000000000000 ) ) ;
#15536 = DIRECTION ( 'NONE',  ( -0.000000000000000000, -1.000000000000000000, -0.000000000000000000 ) ) ;
#15535 = AXIS2_PLACEMENT_3D ( 'NONE', #1775, #11794, #17184 ) ;
#15537 = ORIENTED_EDGE ( 'NONE', *, *, #8224, .T. ) ;
#15538 = LINE ( 'NONE', #28181, #12142 ) ;
#15539 = CARTESIAN_POINT ( 'NONE',  ( 8.732853799281738105, 26.46183152705960140, 47.04930799450051637 ) ) ;
#15540 = FACE_OUTER_BOUND ( 'NONE', #11273, .T. ) ;
#15541 = CYLINDRICAL_SURFACE ( 'NONE', #9090, 84.30000000000001137 ) ;
#15542 = LINE ( 'NONE', #25553, #18370 ) ;
#15543 = CARTESIAN_POINT ( 'NONE',  ( 45.36511207810799107, 28.60948166895303402, 45.12672418911606087 ) ) ;
#15544 = CARTESIAN_POINT ( 'NONE',  ( -41.77464577679392477, 3.808795504615560379, 47.04930799450051637 ) ) ;
#15545 = EDGE_LOOP ( 'NONE', ( #9380, #12514, #14706, #23313 ) ) ;
#15546 = FACE_OUTER_BOUND ( 'NONE', #957, .T. ) ;
#15547 = AXIS2_PLACEMENT_3D ( 'NONE', #15321, #10397, #20394 ) ;
#15548 = DIRECTION ( 'NONE',  ( 1.000000000000000000, -0.000000000000000000, -0.000000000000000000 ) ) ;
#15549 = VERTEX_POINT ( 'NONE', #26748 ) ;
#15550 = VERTEX_POINT ( 'NONE', #19349 ) ;
#15551 = CYLINDRICAL_SURFACE ( 'NONE', #25158, 12.36707279061065101 ) ;
#15552 = EDGE_LOOP ( 'NONE', ( #11108, #18799, #20869, #22986 ) ) ;
#15553 = AXIS2_PLACEMENT_3D ( 'NONE', #2268, #15070, #28150 ) ;
#15554 = ORIENTED_EDGE ( 'NONE', *, *, #24678, .T. ) ;
#15555 = CARTESIAN_POINT ( 'NONE',  ( 21.09992658989238734, 32.09164230456639899, 47.04930799450051637 ) ) ;
#15556 = TOROIDAL_SURFACE ( 'NONE', #31299, 13.30178401536290878, 0.2000000000000002609 ) ;
#15557 = VERTEX_POINT ( 'NONE', #29375 ) ;
#15558 = EDGE_CURVE ( 'NONE', #17658, #1940, #6893, .T. ) ;
#15559 = EDGE_CURVE ( 'NONE', #11505, #17692, #25312, .T. ) ;
#15560 = DIRECTION ( 'NONE',  ( -1.000000000000000000, 0.000000000000000000, 0.000000000000000000 ) ) ;
#15561 = EDGE_CURVE ( 'NONE', #29641, #29156, #15972, .T. ) ;
#15562 = DIRECTION ( 'NONE',  ( 1.000000000000000000, 0.000000000000000000, 0.000000000000000000 ) ) ;
#15563 = CARTESIAN_POINT ( 'NONE',  ( 47.09785597605719687, 15.77906836436399374, 47.04930799450078638 ) ) ;
#15564 = EDGE_CURVE ( 'NONE', #17073, #5065, #11164, .T. ) ;
#15565 = CARTESIAN_POINT ( 'NONE',  ( 45.38854177497844944, 26.92622849631043991, 45.94041160078741370 ) ) ;
#15566 = ORIENTED_EDGE ( 'NONE', *, *, #20202, .F. ) ;
#15567 = EDGE_LOOP ( 'NONE', ( #10257, #3698, #3222, #24351 ) ) ;
#15568 = FACE_OUTER_BOUND ( 'NONE', #27087, .T. ) ;
#15569 = EDGE_LOOP ( 'NONE', ( #18185, #13390, #31367, #32172 ) ) ;
#15570 = FACE_OUTER_BOUND ( 'NONE', #17794, .T. ) ;
#15571 = CARTESIAN_POINT ( 'NONE',  ( -41.63422246745999189, 11.51531537899137447, 57.04930799450051637 ) ) ;
#15572 = DIRECTION ( 'NONE',  ( -1.101824276508909887E-16, 1.000000000000000000, -0.000000000000000000 ) ) ;
#15573 = DIRECTION ( 'NONE',  ( 0.000000000000000000, 0.000000000000000000, -1.000000000000000000 ) ) ;
#15574 = CARTESIAN_POINT ( 'NONE',  ( 48.83862994770795041, 25.15457786121582373, 48.17861352429476085 ) ) ;
#15575 = EDGE_LOOP ( 'NONE', ( #14211, #10299, #21457, #30476 ) ) ;
#15576 = DIRECTION ( 'NONE',  ( -1.000000000000000000, 0.000000000000000000, 0.000000000000000000 ) ) ;
#15577 = AXIS2_PLACEMENT_3D ( 'NONE', #25675, #31094, #18915 ) ;
#15578 = CARTESIAN_POINT ( 'NONE',  ( 21.09992658989239089, 23.96664230456639899, 47.04930799450051637 ) ) ;
#15579 = DIRECTION ( 'NONE',  ( -1.000000000000000000, 0.000000000000000000, 0.000000000000000000 ) ) ;
#15580 = CARTESIAN_POINT ( 'NONE',  ( 46.00908685603032922, 26.23284706826093071, 44.91496614357595263 ) ) ;
#15581 = ORIENTED_EDGE ( 'NONE', *, *, #7357, .F. ) ;
#15582 = CARTESIAN_POINT ( 'NONE',  ( 21.09992658989238734, 31.72145308207317171, 47.04930799450051637 ) ) ;
#15583 = DIRECTION ( 'NONE',  ( -0.000000000000000000, -1.000000000000000000, 0.000000000000000000 ) ) ;
#15584 = CARTESIAN_POINT ( 'NONE',  ( 21.09785597605719332, 47.56454579224779877, 47.04930799450051637 ) ) ;
#15585 = VERTEX_POINT ( 'NONE', #32491 ) ;
#15586 =( BOUNDED_CURVE ( )  B_SPLINE_CURVE ( 2, ( #18637, #15543, #13738, #28024, #30812, #23418, #28186, #1091, #25554 ),
 .UNSPECIFIED., .F., .F. ) 
 B_SPLINE_CURVE_WITH_KNOTS ( ( 3, 2, 2, 2, 3 ),
 ( 0.6785714274101559695, 0.6904761904761904656, 0.7142857142857143016, 0.7380952380952381375, 0.7499999988387272554 ),
 .UNSPECIFIED. ) 
 CURVE ( )  GEOMETRIC_REPRESENTATION_ITEM ( )  RATIONAL_B_SPLINE_CURVE ( ( 0.9330127018922199644, 0.9330126953578159466, 1.000000000000000000, 0.8660254037844387076, 1.000000000000000000, 0.8660254037844387076, 1.000000000000000000, 0.9330127084266233162, 0.9330127018922199644 ) ) 
 REPRESENTATION_ITEM ( '' )  );
#15587 = EDGE_CURVE ( 'NONE', #1567, #9952, #31592, .T. ) ;
#15588 = EDGE_CURVE ( 'NONE', #19042, #12544, #23546, .T. ) ;
#15589 = ORIENTED_EDGE ( 'NONE', *, *, #26204, .F. ) ;
#15590 = ORIENTED_EDGE ( 'NONE', *, *, #31273, .F. ) ;
#15591 = DIRECTION ( 'NONE',  ( 0.000000000000000000, 0.000000000000000000, 1.000000000000000000 ) ) ;
#15592 = AXIS2_PLACEMENT_3D ( 'NONE', #851, #10876, #20867 ) ;
#15593 = CARTESIAN_POINT ( 'NONE',  ( -44.78404486970123344, -5.108345900017423169, 52.41914759286123626 ) ) ;
#15594 = CARTESIAN_POINT ( 'NONE',  ( -40.57832940339291383, 7.446916344587776848, 60.54930799450051637 ) ) ;
#15595 = VECTOR ( 'NONE', #24420, 1000.000000000000114 ) ;
#15596 = ORIENTED_EDGE ( 'NONE', *, *, #15558, .F. ) ;
#15597 = CARTESIAN_POINT ( 'NONE',  ( -29.27613032885505007, -5.952175616702188421, 78.54874598263256757 ) ) ;
#15598 = CIRCLE ( 'NONE', #27671, 0.1250000000000001110 ) ;
#15599 = DIRECTION ( 'NONE',  ( 0.000000000000000000, -1.000000000000000000, 0.000000000000000000 ) ) ;
#15600 = DIRECTION ( 'NONE',  ( 0.000000000000000000, 1.000000000000000000, 0.000000000000000000 ) ) ;
#15601 = EDGE_CURVE ( 'NONE', #10149, #10609, #32331, .T. ) ;
#15602 = DIRECTION ( 'NONE',  ( 0.000000000000000000, 0.000000000000000000, -1.000000000000000000 ) ) ;
#15603 = CARTESIAN_POINT ( 'NONE',  ( -37.47960991055109758, -5.772969811237893545, 78.78223253563916728 ) ) ;
#15604 = AXIS2_PLACEMENT_3D ( 'NONE', #25342, #12391, #20087 ) ;
#15605 = DIRECTION ( 'NONE',  ( 0.5442436726714898754, 1.289618226626749973E-16, -0.8389271868029121171 ) ) ;
#15606 = DIRECTION ( 'NONE',  ( 1.234978253042719660E-16, -1.000000000000000000, -1.109335647967047851E-31 ) ) ;
#15607 = CARTESIAN_POINT ( 'NONE',  ( 48.24519908733286400, 29.46405251693653682, 48.93429100061246118 ) ) ;
#15608 = CARTESIAN_POINT ( 'NONE',  ( 21.09992658989238734, 32.54735957529758394, 47.04930799450051637 ) ) ;
#15609 = B_SPLINE_SURFACE_WITH_KNOTS ( 'NONE', 3, 1, ( 
 ( #24598, #24934 ),
 ( #21808, #27061 ),
 ( #7205, #9513 ),
 ( #4913, #19507 ),
 ( #31826, #421 ),
 ( #31994, #29539 ) ),
 .UNSPECIFIED., .F., .F., .F.,
 ( 4, 1, 1, 4 ),
 ( 2, 2 ),
 ( 0.1800733115436725096, 0.3950736110976382220, 0.6810807126490734387, 1.000000000000000000 ),
 ( 0.000000000000000000, 1.000000000000000000 ),
 .UNSPECIFIED. ) ;
#15610 = CARTESIAN_POINT ( 'NONE',  ( 47.27395380374088774, 22.74928388133296764, 49.52406241924104791 ) ) ;
#15611 = CARTESIAN_POINT ( 'NONE',  ( -41.10400476907452116, 9.333823787025618657, 34.66646528202590360 ) ) ;
#15612 = ORIENTED_EDGE ( 'NONE', *, *, #7768, .T. ) ;
#15613 = ORIENTED_EDGE ( 'NONE', *, *, #2846, .T. ) ;
#15614 = DIRECTION ( 'NONE',  ( -0.9612616959383194493, -0.2756373558169974980, -8.795445018804946186E-19 ) ) ;
#15615 = DIRECTION ( 'NONE',  ( -1.101824276508909887E-16, 1.000000000000000000, -0.000000000000000000 ) ) ;
#15616 = DIRECTION ( 'NONE',  ( 0.000000000000000000, -0.8290375725550389596, -0.5591929034707507906 ) ) ;
#15617 = ORIENTED_EDGE ( 'NONE', *, *, #2994, .T. ) ;
#15618 = DIRECTION ( 'NONE',  ( -1.101824276508909887E-16, 1.000000000000000000, -0.000000000000000000 ) ) ;
#15619 = FACE_OUTER_BOUND ( 'NONE', #25504, .T. ) ;
#15620 = EDGE_CURVE ( 'NONE', #12130, #17686, #16101, .T. ) ;
#15621 = ORIENTED_EDGE ( 'NONE', *, *, #24805, .T. ) ;
#15622 = ORIENTED_EDGE ( 'NONE', *, *, #10686, .T. ) ;
#15623 = DIRECTION ( 'NONE',  ( -1.000000000000000000, -1.101824276508909887E-16, 0.000000000000000000 ) ) ;
#15624 = CARTESIAN_POINT ( 'NONE',  ( 45.79384627280941089, 26.46618040159426144, 49.05938063676249072 ) ) ;
#15625 = AXIS2_PLACEMENT_3D ( 'NONE', #6006, #18621, #28332 ) ;
#15626 = CARTESIAN_POINT ( 'NONE',  ( 49.49063479933183629, 28.01291119454915091, 47.17357720316391578 ) ) ;
#15627 = VECTOR ( 'NONE', #6001, 1000.000000000000000 ) ;
#15628 = EDGE_CURVE ( 'NONE', #25082, #9462, #13268, .T. ) ;
#15629 = CARTESIAN_POINT ( 'NONE',  ( -43.90780810587784089, -0.03953120679776617880, 61.94930799450052206 ) ) ;
#15630 = VECTOR ( 'NONE', #12853, 1000.000000000000114 ) ;
#15631 = EDGE_CURVE ( 'NONE', #27949, #29666, #22129, .T. ) ;
#15632 = EDGE_CURVE ( 'NONE', #17901, #7171, #9591, .T. ) ;
#15633 = AXIS2_PLACEMENT_3D ( 'NONE', #546, #8109, #5967 ) ;
#15634 = ORIENTED_EDGE ( 'NONE', *, *, #31643, .T. ) ;
#15635 = EDGE_CURVE ( 'NONE', #27727, #24189, #7493, .T. ) ;
#15636 = CYLINDRICAL_SURFACE ( 'NONE', #10407, 2.499999999999997335 ) ;
#15637 = DIRECTION ( 'NONE',  ( 0.000000000000000000, 0.000000000000000000, 1.000000000000000000 ) ) ;
#15638 = ORIENTED_EDGE ( 'NONE', *, *, #2716, .T. ) ;
#15639 = DIRECTION ( 'NONE',  ( 0.000000000000000000, 0.000000000000000000, 1.000000000000000000 ) ) ;
#15640 = DIRECTION ( 'NONE',  ( -1.000000000000000000, 0.000000000000000000, 0.000000000000000000 ) ) ;
#15641 = ADVANCED_FACE ( 'NONE', ( #25261 ), #19675, .F. ) ;
#15642 = CARTESIAN_POINT ( 'NONE',  ( 76.33917176002422877, -3.872051342217440517, 13.53113187053797972 ) ) ;
#15643 = VECTOR ( 'NONE', #16891, 1000.000000000000114 ) ;
#15644 = CIRCLE ( 'NONE', #29283, 0.1249999999999983763 ) ;
#15645 = ORIENTED_EDGE ( 'NONE', *, *, #10847, .F. ) ;
#15646 = LINE ( 'NONE', #20734, #10260 ) ;
#15647 = AXIS2_PLACEMENT_3D ( 'NONE', #21019, #16256, #1482 ) ;
#15648 = DIRECTION ( 'NONE',  ( -1.000000000000000000, 0.000000000000000000, 0.000000000000000000 ) ) ;
#15649 = DIRECTION ( 'NONE',  ( 0.2756373558169973870, -0.9612616959383193382, -1.315048337272770280E-17 ) ) ;
#15650 = CARTESIAN_POINT ( 'NONE',  ( 21.09785597605720753, -5.098646251524523443, 47.04930799450052348 ) ) ;
#15651 = CARTESIAN_POINT ( 'NONE',  ( -40.69549116917064424, 6.786800228906571419, 39.45362111768539393 ) ) ;
#15652 = ORIENTED_EDGE ( 'NONE', *, *, #9627, .F. ) ;
#15653 = CARTESIAN_POINT ( 'NONE',  ( -42.11634311166133671, 14.67824478428857660, 37.04930799450052348 ) ) ;
#15654 = DIRECTION ( 'NONE',  ( -1.000000000000000000, 0.000000000000000000, 0.000000000000000000 ) ) ;
#15655 = DIRECTION ( 'NONE',  ( 1.000000000000000000, 0.000000000000000000, 0.000000000000000000 ) ) ;
#15656 = DIRECTION ( 'NONE',  ( -1.101824276508909887E-16, 1.000000000000000000, -0.000000000000000000 ) ) ;
#15657 = VECTOR ( 'NONE', #30411, 1000.000000000000227 ) ;
#15658 = CARTESIAN_POINT ( 'NONE',  ( -40.62017490690358557, 6.854514378931026997, 39.32186498431286026 ) ) ;
#15659 = ORIENTED_EDGE ( 'NONE', *, *, #23712, .F. ) ;
#15660 = DIRECTION ( 'NONE',  ( -0.000000000000000000, -1.000000000000000000, 0.000000000000000000 ) ) ;
#15661 = CARTESIAN_POINT ( 'NONE',  ( 49.64105649875294546, 24.93604219378083187, 46.47965702198763438 ) ) ;
#15662 = CARTESIAN_POINT ( 'NONE',  ( 8.474859994195286461, 28.84143805560861296, 47.04930799450051637 ) ) ;
#15663 = EDGE_CURVE ( 'NONE', #17323, #31343, #30024, .T. ) ;
#15664 = ORIENTED_EDGE ( 'NONE', *, *, #15718, .F. ) ;
#15665 = CARTESIAN_POINT ( 'NONE',  ( -10.16620058928556780, -5.922252862938464091, -12.36825037132245697 ) ) ;
#15666 = DIRECTION ( 'NONE',  ( 0.000000000000000000, 0.000000000000000000, 1.000000000000000000 ) ) ;
#15667 = DIRECTION ( 'NONE',  ( -1.000000000000000000, 0.000000000000000000, 0.000000000000000000 ) ) ;
#15668 = EDGE_CURVE ( 'NONE', #14556, #9452, #15878, .T. ) ;
#15669 = CARTESIAN_POINT ( 'NONE',  ( 54.63929679171693721, -1.094061166256825812, -7.310699946633206103 ) ) ;
#15670 = EDGE_LOOP ( 'NONE', ( #20837, #12376, #7121, #18030 ) ) ;
#15671 = DIRECTION ( 'NONE',  ( -1.000000000000000000, 0.000000000000000000, 0.000000000000000000 ) ) ;
#15672 = ORIENTED_EDGE ( 'NONE', *, *, #16033, .T. ) ;
#15673 = CONICAL_SURFACE ( 'NONE', #1506, 19.45967690998103805, 0.7960495370845414032 ) ;
#15674 = ADVANCED_FACE ( 'NONE', ( #8510 ), #20055, .T. ) ;
#15675 = ORIENTED_EDGE ( 'NONE', *, *, #6595, .F. ) ;
#15677 = EDGE_CURVE ( 'NONE', #16051, #30056, #3198, .T. ) ;
#15676 = B_SPLINE_CURVE_WITH_KNOTS ( 'NONE', 3,
 ( #6956, #16952, #26976, #27303, #4822, #24507, #2028, #12045, #32072, #9587, #9912, #7455 ),
 .UNSPECIFIED., .F., .F.,
 ( 4, 2, 2, 2, 2, 4 ),
 ( 0.0003422200191418649728, 0.002082436906217386297, 0.003822653793292908001, 0.005562870680368429271, 0.006432979123906190123, 0.007303087567443950975 ),
 .UNSPECIFIED. ) ;
#15678 = VECTOR ( 'NONE', #12661, 1000.000000000000114 ) ;
#15679 = AXIS2_PLACEMENT_3D ( 'NONE', #5584, #30702, #10192 ) ;
#15680 = DIRECTION ( 'NONE',  ( -2.779292025043186357E-18, 1.288349127009862057E-17, -1.000000000000000000 ) ) ;
#15681 = FACE_OUTER_BOUND ( 'NONE', #9219, .T. ) ;
#15682 = LINE ( 'NONE', #3203, #18744 ) ;
#15683 = ORIENTED_EDGE ( 'NONE', *, *, #22671, .T. ) ;
#15684 = CARTESIAN_POINT ( 'NONE',  ( 21.09785597605720753, 14.46497581658974063, 47.04930799450052348 ) ) ;
#15685 = VERTEX_POINT ( 'NONE', #7870 ) ;
#15686 = CARTESIAN_POINT ( 'NONE',  ( -10.97410526921440521, -5.983766253076979069, 97.43646483284780402 ) ) ;
#15687 = DIRECTION ( 'NONE',  ( -1.000000000000000000, 0.000000000000000000, 0.000000000000000000 ) ) ;
#15688 = CARTESIAN_POINT ( 'NONE',  ( 21.09992658989239089, 27.34164230456639544, 47.04930799450051637 ) ) ;
#15689 = DIRECTION ( 'NONE',  ( 0.000000000000000000, -0.000000000000000000, -1.000000000000000000 ) ) ;
#15690 = ORIENTED_EDGE ( 'NONE', *, *, #24466, .F. ) ;
#15691 = LINE ( 'NONE', #31445, #18060 ) ;
#15692 = EDGE_LOOP ( 'NONE', ( #21541, #24629, #2781, #1978 ) ) ;
#15693 = DIRECTION ( 'NONE',  ( -0.9862637841664554372, -0.1651779284337450415, 0.000000000000000000 ) ) ;
#15694 = CARTESIAN_POINT ( 'NONE',  ( -40.68535844407768565, 8.206233278606879011, 59.57859731638185963 ) ) ;
#15695 = CIRCLE ( 'NONE', #31938, 12.62506659569710266 ) ;
#15696 = VERTEX_POINT ( 'NONE', #13291 ) ;
#15697 = CARTESIAN_POINT ( 'NONE',  ( 49.65101332465108186, 24.93501648625822398, 46.52608845888364186 ) ) ;
#15698 = VECTOR ( 'NONE', #19579, 1000.000000000000227 ) ;
#15699 = CARTESIAN_POINT ( 'NONE',  ( 21.09992658989239089, 29.22145308207318237, 47.04930799450051637 ) ) ;
#15700 = FACE_OUTER_BOUND ( 'NONE', #26891, .T. ) ;
#15701 = DIRECTION ( 'NONE',  ( -0.000000000000000000, -1.000000000000000000, 0.000000000000000000 ) ) ;
#15702 = CARTESIAN_POINT ( 'NONE',  ( 48.94625023931840957, 25.27124452788249442, 46.10640627770150246 ) ) ;
#15703 = CARTESIAN_POINT ( 'NONE',  ( -42.38687957179149635, 4.148162238788000167, 35.84930799450052064 ) ) ;
#15704 = FACE_OUTER_BOUND ( 'NONE', #8835, .T. ) ;
#15705 = ADVANCED_FACE ( 'NONE', ( #25745 ), #5564, .T. ) ;
#15706 = ORIENTED_EDGE ( 'NONE', *, *, #15843, .T. ) ;
#15707 = DIRECTION ( 'NONE',  ( 0.000000000000000000, 0.000000000000000000, -1.000000000000000000 ) ) ;
#15708 = ORIENTED_EDGE ( 'NONE', *, *, #15165, .T. ) ;
#15709 = AXIS2_PLACEMENT_3D ( 'NONE', #16100, #7933, #18404 ) ;
#15710 = AXIS2_PLACEMENT_3D ( 'NONE', #25840, #25685, #20754 ) ;
#15711 = CARTESIAN_POINT ( 'NONE',  ( -18.40214402394278892, -5.098646251524523443, 47.04930799450052348 ) ) ;
#15712 = ORIENTED_EDGE ( 'NONE', *, *, #6801, .F. ) ;
#15713 = AXIS2_PLACEMENT_3D ( 'NONE', #16390, #20833, #10842 ) ;
#15714 = EDGE_LOOP ( 'NONE', ( #32065, #12108, #23663, #7656 ) ) ;
#15715 = CARTESIAN_POINT ( 'NONE',  ( -9.745345167868416425, 4.618558202237278643, 99.33977322240662033 ) ) ;
#15716 = EDGE_CURVE ( 'NONE', #7248, #28192, #19535, .T. ) ;
#15717 = ORIENTED_EDGE ( 'NONE', *, *, #18845, .T. ) ;
#15718 = EDGE_CURVE ( 'NONE', #1319, #1121, #20319, .T. ) ;
#15719 = EDGE_CURVE ( 'NONE', #14982, #11505, #27422, .T. ) ;
#15720 = CIRCLE ( 'NONE', #1556, 12.62506659569710266 ) ;
#15721 = AXIS2_PLACEMENT_3D ( 'NONE', #2242, #12428, #18105 ) ;
#15722 = VERTEX_POINT ( 'NONE', #15898 ) ;
#15723 = LINE ( 'NONE', #3247, #15983 ) ;
#15724 = AXIS2_PLACEMENT_3D ( 'NONE', #5899, #15905, #2782 ) ;
#15725 = TOROIDAL_SURFACE ( 'NONE', #6281, 12.40141737965284641, 0.1249999999999995698 ) ;
#15726 = ORIENTED_EDGE ( 'NONE', *, *, #12359, .T. ) ;
#15727 = CARTESIAN_POINT ( 'NONE',  ( 48.74539165043771760, 22.91413368675619111, 47.78185833695556539 ) ) ;
#15728 = VECTOR ( 'NONE', #5641, 1000.000000000000114 ) ;
#15729 = CARTESIAN_POINT ( 'NONE',  ( -40.21210701746133509, 7.644196001419694575, 60.44930799450051495 ) ) ;
#15730 = CARTESIAN_POINT ( 'NONE',  ( -40.05313298863235616, 9.531126477505384997, 39.44930799450052206 ) ) ;
#15731 = CARTESIAN_POINT ( 'NONE',  ( 47.20353132263855400, 25.40956182964377419, 45.01455027646040463 ) ) ;
#15732 = TOROIDAL_SURFACE ( 'NONE', #9509, 12.61792373059894778, 0.1249999999999986539 ) ;
#15733 = VECTOR ( 'NONE', #23342, 1000.000000000000114 ) ;
#15734 = ORIENTED_EDGE ( 'NONE', *, *, #4298, .F. ) ;
#15735 = ORIENTED_EDGE ( 'NONE', *, *, #13182, .T. ) ;
#15736 = ORIENTED_EDGE ( 'NONE', *, *, #21228, .F. ) ;
#15737 = DIRECTION ( 'NONE',  ( 0.4848096202463365034, 0.8746197071393960742, -2.220446049250311602E-16 ) ) ;
#15738 = CARTESIAN_POINT ( 'NONE',  ( 53.30244988830531838, -5.573920848077356993, 105.0704484403068619 ) ) ;
#15739 = DIRECTION ( 'NONE',  ( 0.000000000000000000, 0.000000000000000000, 1.000000000000000000 ) ) ;
#15740 = B_SPLINE_CURVE_WITH_KNOTS ( 'NONE', 3,
 ( #23056, #3190, #8454, #15516, #25526, #13234 ),
 .UNSPECIFIED., .F., .F.,
 ( 4, 2, 4 ),
 ( 0.000000000000000000, 0.5000000000000000000, 1.000000000000000000 ),
 .UNSPECIFIED. ) ;
#15741 = CARTESIAN_POINT ( 'NONE',  ( 21.09992658989239089, 23.97145308207319658, 47.04930799450051637 ) ) ;
#15742 = DIRECTION ( 'NONE',  ( 0.8746197071393858602, -0.4848096202463547666, 0.000000000000000000 ) ) ;
#15743 = CONTEXT_DEPENDENT_SHAPE_REPRESENTATION ( #19776, #11131 ) ;
#15744 = ORIENTED_EDGE ( 'NONE', *, *, #2034, .T. ) ;
#15745 = CARTESIAN_POINT ( 'NONE',  ( -33.20214402394279318, 14.56454579224780232, 47.04930799450052348 ) ) ;
#15746 = AXIS2_PLACEMENT_3D ( 'NONE', #8903, #18905, #2495 ) ;
#15747 = DIRECTION ( 'NONE',  ( 1.000000000000000000, 0.000000000000000000, 0.000000000000000000 ) ) ;
#15748 = DIRECTION ( 'NONE',  ( -1.000000000000000000, 0.000000000000000000, 0.000000000000000000 ) ) ;
#15749 = DIRECTION ( 'NONE',  ( 0.000000000000000000, -1.000000000000000000, -0.000000000000000000 ) ) ;
#15750 = ORIENTED_EDGE ( 'NONE', *, *, #3746, .F. ) ;
#15751 = CARTESIAN_POINT ( 'NONE',  ( 21.09785597605720042, -13.59284023713420630, 47.04930799450051637 ) ) ;
#15752 = FACE_OUTER_BOUND ( 'NONE', #4207, .T. ) ;
#15753 = ADVANCED_FACE ( 'NONE', ( #17872 ), #3413, .T. ) ;
#15754 = ORIENTED_EDGE ( 'NONE', *, *, #24694, .T. ) ;
#15755 = ADVANCED_FACE ( 'NONE', ( #3082 ), #948, .T. ) ;
#15756 = EDGE_CURVE ( 'NONE', #3952, #28505, #20600, .T. ) ;
#15757 = ADVANCED_FACE ( 'NONE', ( #28533 ), #6049, .T. ) ;
#15758 = TOROIDAL_SURFACE ( 'NONE', #13658, 12.61792373059897798, 0.1249999999999968636 ) ;
#15759 = EDGE_CURVE ( 'NONE', #7622, #27343, #2928, .T. ) ;
#15760 = ADVANCED_FACE ( 'NONE', ( #22944 ), #2794, .T. ) ;
#15761 = AXIS2_PLACEMENT_3D ( 'NONE', #1087, #18479, #28507 ) ;
#15762 = CIRCLE ( 'NONE', #13075, 12.48414152717711190 ) ;
#15763 = CIRCLE ( 'NONE', #19403, 56.47014401861810029 ) ;
#15764 = ORIENTED_EDGE ( 'NONE', *, *, #28316, .T. ) ;
#15765 = ORIENTED_EDGE ( 'NONE', *, *, #28038, .T. ) ;
#15766 = DIRECTION ( 'NONE',  ( 0.4848096202463430537, 0.8746197071393926326, 1.323854077651070671E-16 ) ) ;
#15767 = CARTESIAN_POINT ( 'NONE',  ( 21.09992658989239089, 29.21664230456640254, 47.04930799450051637 ) ) ;
#15768 = DIRECTION ( 'NONE',  ( -1.000000000000000000, 0.000000000000000000, 0.000000000000000000 ) ) ;
#15769 = CIRCLE ( 'NONE', #21509, 54.10000000000000142 ) ;
#15770 = ORIENTED_EDGE ( 'NONE', *, *, #1538, .F. ) ;
#15771 = DIRECTION ( 'NONE',  ( -1.101824276508909887E-16, 1.000000000000000000, -0.000000000000000000 ) ) ;
#15772 = CARTESIAN_POINT ( 'NONE',  ( 81.51037581727311476, -5.935668773294344724, 15.94125244514089523 ) ) ;
#15773 = CARTESIAN_POINT ( 'NONE',  ( -40.98031486389898248, 9.265261353013489298, 39.44930799450052206 ) ) ;
#15774 = DIRECTION ( 'NONE',  ( -1.101824276508909887E-16, 1.000000000000000000, -0.000000000000000000 ) ) ;
#15775 = DIRECTION ( 'NONE',  ( 0.000000000000000000, 1.000000000000000000, 0.000000000000000000 ) ) ;
#15776 = CARTESIAN_POINT ( 'NONE',  ( 21.09785597605718621, 77.37241625295546044, 47.04930799450051637 ) ) ;
#15777 = CARTESIAN_POINT ( 'NONE',  ( 8.823509210239569356, 30.84164230456639544, 47.04930799450051637 ) ) ;
#15778 = CARTESIAN_POINT ( 'NONE',  ( -42.41019933908752648, 14.71530103803245915, 55.14139656020049785 ) ) ;
#15779 = TOROIDAL_SURFACE ( 'NONE', #13168, 23.50000000000000000, 1.500000000000001332 ) ;
#15780 = DIRECTION ( 'NONE',  ( -0.9612616959383200044, -0.2756373558169954996, 1.660411357259285896E-16 ) ) ;
#15781 = CARTESIAN_POINT ( 'NONE',  ( 21.09785597605719332, 25.56454579224779877, 35.04930799450050927 ) ) ;
#15782 = COLOUR_RGB ( '',0.7921568627450980005, 0.8196078431372548767, 0.9333333333333333481 ) ;
#15783 = FILL_AREA_STYLE_COLOUR ( '', #27588 ) ;
#15784 = VERTEX_POINT ( 'NONE', #8037 ) ;
#15785 = ORIENTED_EDGE ( 'NONE', *, *, #11243, .F. ) ;
#15786 = ADVANCED_FACE ( 'NONE', ( #23118 ), #13806, .T. ) ;
#15787 = FACE_OUTER_BOUND ( 'NONE', #16774, .T. ) ;
#15788 = AXIS2_PLACEMENT_3D ( 'NONE', #23045, #2866, #25359 ) ;
#15789 = DIRECTION ( 'NONE',  ( 0.000000000000000000, 0.000000000000000000, -1.000000000000000000 ) ) ;
#15790 = CARTESIAN_POINT ( 'NONE',  ( 54.49195827015791593, -0.5585041340025316270, 100.2085587256018471 ) ) ;
#15791 = ORIENTED_EDGE ( 'NONE', *, *, #21961, .T. ) ;
#15792 =( BOUNDED_CURVE ( )  B_SPLINE_CURVE ( 3, ( #841, #6414, #10866, #18393 ),
 .UNSPECIFIED., .F., .F. ) 
 B_SPLINE_CURVE_WITH_KNOTS ( ( 4, 4 ),
 ( 4.712388980384698556, 5.497787143782109531 ),
 .UNSPECIFIED. ) 
 CURVE ( )  GEOMETRIC_REPRESENTATION_ITEM ( )  RATIONAL_B_SPLINE_CURVE ( ( 1.000000000000000000, 0.9492530216741960070, 0.9492530216741960070, 1.000000000000000000 ) ) 
 REPRESENTATION_ITEM ( '' )  );
#15793 = DIRECTION ( 'NONE',  ( -1.000000000000000000, 0.000000000000000000, 0.000000000000000000 ) ) ;
#15794 = CARTESIAN_POINT ( 'NONE',  ( -40.02353495526242710, 6.996741961792354303, 39.54930799450052348 ) ) ;
#15795 = ORIENTED_EDGE ( 'NONE', *, *, #21881, .F. ) ;
#15796 = PLANE ( 'NONE',  #9985 ) ;
#15797 = CARTESIAN_POINT ( 'NONE',  ( 45.79384627280941089, 27.86618040159426357, 49.05938063676249072 ) ) ;
#15798 = AXIS2_PLACEMENT_3D ( 'NONE', #2174, #4308, #12188 ) ;
#15799 = CARTESIAN_POINT ( 'NONE',  ( 45.79384627280941089, 27.77957786121582018, 49.05938063676249072 ) ) ;
#15800 = CARTESIAN_POINT ( 'NONE',  ( -39.39937829020581006, -5.936106920828554401, 77.94045110924388098 ) ) ;
#15801 = ADVANCED_FACE ( 'NONE', ( #636 ), #24793, .F. ) ;
#15802 = EDGE_CURVE ( 'NONE', #13009, #32191, #3843, .T. ) ;
#15803 = ORIENTED_EDGE ( 'NONE', *, *, #30, .F. ) ;
#15804 = AXIS2_PLACEMENT_3D ( 'NONE', #28342, #25713, #5531 ) ;
#15805 = AXIS2_PLACEMENT_3D ( 'NONE', #4852, #88, #27501 ) ;
#15806 = CONICAL_SURFACE ( 'NONE', #1645, 13.00000000000000533, 0.7853981633974482790 ) ;
#15807 = CARTESIAN_POINT ( 'NONE',  ( -42.41019933908752648, 14.71530103803245915, 60.54930799450051637 ) ) ;
#15808 =( REPRESENTATION_RELATIONSHIP ('NONE','NONE', #20382, #11371 ) REPRESENTATION_RELATIONSHIP_WITH_TRANSFORMATION ( #17557 )SHAPE_REPRESENTATION_RELATIONSHIP( ) );
#15809 = CARTESIAN_POINT ( 'NONE',  ( 47.77416835495956349, 22.84434098701873950, 49.08712782507307537 ) ) ;
#15810 = VERTEX_POINT ( 'NONE', #9144 ) ;
#15811 = LINE ( 'NONE', #10890, #24329 ) ;
#15812 = TOROIDAL_SURFACE ( 'NONE', #20519, 2.799999999999998490, 0.2999999999999999334 ) ;
#15813 = DIRECTION ( 'NONE',  ( -1.000000000000000000, -1.101824276508909764E-16, 0.000000000000000000 ) ) ;
#15814 = EDGE_CURVE ( 'NONE', #3553, #19298, #12219, .T. ) ;
#15815 = ORIENTED_EDGE ( 'NONE', *, *, #13461, .F. ) ;
#15816 = CARTESIAN_POINT ( 'NONE',  ( -42.47434154250544225, 4.196643200812637531, 57.04930799450051637 ) ) ;
#15817 = CARTESIAN_POINT ( 'NONE',  ( 21.09785597605720042, 14.86454579224779771, 95.68336035963606889 ) ) ;
#15818 = DIRECTION ( 'NONE',  ( -0.000000000000000000, 1.000000000000000000, 0.000000000000000000 ) ) ;
#15819 = FACE_OUTER_BOUND ( 'NONE', #3324, .T. ) ;
#15820 = ORIENTED_EDGE ( 'NONE', *, *, #2814, .T. ) ;
#15821 = EDGE_CURVE ( 'NONE', #25773, #30925, #31616, .T. ) ;
#15822 = CARTESIAN_POINT ( 'NONE',  ( 46.33059210211230550, 22.93807716476589675, 45.54522087609679204 ) ) ;
#15823 = DIRECTION ( 'NONE',  ( -7.588956326749211550E-18, 4.206627182996911684E-18, -1.000000000000000000 ) ) ;
#15824 = EDGE_CURVE ( 'NONE', #12417, #12816, #21116, .T. ) ;
#15825 = CARTESIAN_POINT ( 'NONE',  ( 21.09785597605720753, 14.56454579224780055, 47.04930799450052348 ) ) ;
#15826 = DIRECTION ( 'NONE',  ( 0.000000000000000000, 1.000000000000000000, -0.000000000000000000 ) ) ;
#15827 = AXIS2_PLACEMENT_3D ( 'NONE', #25111, #22805, #10508 ) ;
#15828 = CARTESIAN_POINT ( 'NONE',  ( -40.54018958231235814, 7.005332542891154368, 39.07553933734813967 ) ) ;
#15829 = CIRCLE ( 'NONE', #14266, 2.000000000000001776 ) ;
#15830 = VERTEX_POINT ( 'NONE', #16201 ) ;
#15831 = CIRCLE ( 'NONE', #14781, 0.09999999999999753530 ) ;
#15832 = CARTESIAN_POINT ( 'NONE',  ( 44.59785597605720397, 14.86454579224779948, 47.04930799450052348 ) ) ;
#15833 = CARTESIAN_POINT ( 'NONE',  ( -4.902144023942810236, 25.56454579224779877, 49.54930799450078638 ) ) ;
#15834 = CARTESIAN_POINT ( 'NONE',  ( 21.09785597605720753, 13.86454579224779948, 47.04930799450052348 ) ) ;
#15835 = EDGE_LOOP ( 'NONE', ( #21951, #10135, #14429, #31068 ) ) ;
#15836 = CARTESIAN_POINT ( 'NONE',  ( -9.947536845470862588, -5.938447472589721166, -12.54648800223589333 ) ) ;
#15837 = CARTESIAN_POINT ( 'NONE',  ( 21.09992658989239089, 27.59143805560860940, 47.04930799450051637 ) ) ;
#15838 = CYLINDRICAL_SURFACE ( 'NONE', #26712, 30.00000000000000711 ) ;
#15839 = CARTESIAN_POINT ( 'NONE',  ( 54.78750462725908932, -3.218976025668799146, -8.600583132619711080 ) ) ;
#15840 = ORIENTED_EDGE ( 'NONE', *, *, #2358, .T. ) ;
#15841 = CARTESIAN_POINT ( 'NONE',  ( -40.62282199596570109, 7.625347238340324907, 60.15421819779515289 ) ) ;
#15842 = ORIENTED_EDGE ( 'NONE', *, *, #15866, .F. ) ;
#15843 = EDGE_CURVE ( 'NONE', #21286, #6401, #24353, .T. ) ;
#15844 = AXIS2_PLACEMENT_3D ( 'NONE', #29796, #14534, #11744 ) ;
#15845 = ORIENTED_EDGE ( 'NONE', *, *, #4117, .T. ) ;
#15846 = VECTOR ( 'NONE', #10784, 1000.000000000000000 ) ;
#15847 = CIRCLE ( 'NONE', #31063, 0.1250000000000018319 ) ;
#15848 = AXIS2_PLACEMENT_3D ( 'NONE', #2758, #9988, #2914 ) ;
#15849 = EDGE_CURVE ( 'NONE', #26, #21967, #13759, .T. ) ;
#15850 = DIRECTION ( 'NONE',  ( 0.4848096202463427762, 0.8746197071393926326, 0.000000000000000000 ) ) ;
#15851 = CARTESIAN_POINT ( 'NONE',  ( -35.59135993922510721, -5.255974443259752604, 79.62489112376373157 ) ) ;
#15852 = DIRECTION ( 'NONE',  ( -1.224646799147353207E-16, 0.000000000000000000, -1.000000000000000000 ) ) ;
#15853 = EDGE_CURVE ( 'NONE', #22659, #32483, #2247, .T. ) ;
#15854 = VERTEX_POINT ( 'NONE', #6851 ) ;
#15855 = DIRECTION ( 'NONE',  ( -1.101824276508909887E-16, 1.000000000000000000, -0.000000000000000000 ) ) ;
#15856 = ORIENTED_EDGE ( 'NONE', *, *, #30659, .F. ) ;
#15857 = DIRECTION ( 'NONE',  ( -1.101824276508909887E-16, 1.000000000000000000, -0.000000000000000000 ) ) ;
#15858 = FACE_OUTER_BOUND ( 'NONE', #31411, .T. ) ;
#15859 = CARTESIAN_POINT ( 'NONE',  ( -30.60184210043303921, 11.23625233873419305, 71.15371187152176446 ) ) ;
#15860 = CARTESIAN_POINT ( 'NONE',  ( 21.09992658989239089, 30.47145308207317882, 47.04930799450051637 ) ) ;
#15861 = ORIENTED_EDGE ( 'NONE', *, *, #1422, .T. ) ;
#15862 = DIRECTION ( 'NONE',  ( -1.101824276508909887E-16, 1.000000000000000000, -0.000000000000000000 ) ) ;
#15863 = ORIENTED_EDGE ( 'NONE', *, *, #26937, .T. ) ;
#15864 = CARTESIAN_POINT ( 'NONE',  ( 47.09785597605719687, 19.86454579224779948, 47.04930799450078638 ) ) ;
#15865 = CARTESIAN_POINT ( 'NONE',  ( -40.99173213700658636, 9.305078116158226109, 34.54930799450052348 ) ) ;
#15866 = EDGE_CURVE ( 'NONE', #23684, #31307, #25336, .T. ) ;
#15867 = ORIENTED_EDGE ( 'NONE', *, *, #2113, .T. ) ;
#15868 = DIRECTION ( 'NONE',  ( 0.8746197071393926326, -0.4848096202463430537, -8.676864087101709653E-18 ) ) ;
#15869 = DIRECTION ( 'NONE',  ( 0.000000000000000000, 0.000000000000000000, -1.000000000000000000 ) ) ;
#15870 = DIRECTION ( 'NONE',  ( 3.534951791954965799E-15, 3.759183808608825436E-15, -1.000000000000000000 ) ) ;
#15871 = CARTESIAN_POINT ( 'NONE',  ( 21.09785597605719332, -15.72540370141337007, 47.04930799450051637 ) ) ;
#15872 = EDGE_CURVE ( 'NONE', #27142, #14245, #14320, .T. ) ;
#15873 = AXIS2_PLACEMENT_3D ( 'NONE', #31364, #24450, #16900 ) ;
#15874 =( NAMED_UNIT ( * ) PLANE_ANGLE_UNIT ( ) SI_UNIT ( $, .RADIAN. ) );
#15875 = ORIENTED_EDGE ( 'NONE', *, *, #21513, .T. ) ;
#15876 = DIRECTION ( 'NONE',  ( 0.000000000000000000, 0.000000000000000000, -1.000000000000000000 ) ) ;
#15877 = DIRECTION ( 'NONE',  ( 1.000000000000000000, 0.000000000000000000, -1.224646799147353207E-16 ) ) ;
#15878 = CIRCLE ( 'NONE', #1710, 0.9999999999999998890 ) ;
#15879 = ORIENTED_EDGE ( 'NONE', *, *, #16149, .T. ) ;
#15880 = LINE ( 'NONE', #16658, #27707 ) ;
#15881 = AXIS2_PLACEMENT_3D ( 'NONE', #25064, #22917, #32297 ) ;
#15882 = CARTESIAN_POINT ( 'NONE',  ( 21.09785597605720753, -16.03545420775220265, 117.6483275080933169 ) ) ;
#15883 = ORIENTED_EDGE ( 'NONE', *, *, #25967, .T. ) ;
#15884 = AXIS2_PLACEMENT_3D ( 'NONE', #17645, #17808, #24881 ) ;
#15885 = ORIENTED_EDGE ( 'NONE', *, *, #8136, .F. ) ;
#15886 = CARTESIAN_POINT ( 'NONE',  ( -10.56084922076344235, 3.230235421722207345, 99.74989852988510108 ) ) ;
#15887 = VERTEX_POINT ( 'NONE', #31316 ) ;
#15888 = ORIENTED_EDGE ( 'NONE', *, *, #16753, .T. ) ;
#15889 = AXIS2_PLACEMENT_3D ( 'NONE', #17507, #24899, #2568 ) ;
#15890 = EDGE_CURVE ( 'NONE', #1774, #16834, #8816, .T. ) ;
#15891 = DIRECTION ( 'NONE',  ( -1.000000000000000000, -1.101824276508910010E-16, 0.000000000000000000 ) ) ;
#15892 = EDGE_CURVE ( 'NONE', #13866, #27623, #11184, .T. ) ;
#15893 = ORIENTED_EDGE ( 'NONE', *, *, #23902, .F. ) ;
#15894 = CARTESIAN_POINT ( 'NONE',  ( 81.70930933238793159, -5.935454207752202116, 77.87546120947918382 ) ) ;
#15895 = AXIS2_PLACEMENT_3D ( 'NONE', #21716, #1531, #19416 ) ;
#15896 = AXIS2_PLACEMENT_3D ( 'NONE', #16216, #26236, #1274 ) ;
#15897 = FACE_OUTER_BOUND ( 'NONE', #3197, .T. ) ;
#15898 = CARTESIAN_POINT ( 'NONE',  ( 54.59785597605721108, 13.86454579224779948, 47.04930799450051637 ) ) ;
#15899 = CARTESIAN_POINT ( 'NONE',  ( 48.16694854572211426, 26.51789516297709781, 49.14507740233662503 ) ) ;
#15900 = VERTEX_POINT ( 'NONE', #31794 ) ;
#15901 = ORIENTED_EDGE ( 'NONE', *, *, #1617, .T. ) ;
#15902 = DIRECTION ( 'NONE',  ( -1.101824276508909887E-16, 1.000000000000000000, -0.000000000000000000 ) ) ;
#15903 = ADVANCED_FACE ( 'NONE', ( #26543 ), #1213, .T. ) ;
#15904 = VERTEX_POINT ( 'NONE', #18813 ) ;
#15905 = DIRECTION ( 'NONE',  ( -0.000000000000000000, -1.000000000000000000, 0.000000000000000000 ) ) ;
#15906 = CARTESIAN_POINT ( 'NONE',  ( 53.89934057735932527, -5.043292969097945111, 104.3954240496316714 ) ) ;
#15907 = DIRECTION ( 'NONE',  ( -1.101824276508909887E-16, 1.000000000000000000, -0.000000000000000000 ) ) ;
#15908 = EDGE_LOOP ( 'NONE', ( #376, #18847, #31658, #907 ) ) ;
#15909 = PLANE ( 'NONE',  #7163 ) ;
#15910 = DIRECTION ( 'NONE',  ( -0.7141240004913248507, 0.3958453973319954744, 0.5773502691896323924 ) ) ;
#15911 = VECTOR ( 'NONE', #23570, 1000.000000000000000 ) ;
#15912 = CARTESIAN_POINT ( 'NONE',  ( 48.94625023931840246, 26.05784706826093355, 46.10640627770148825 ) ) ;
#15913 = AXIS2_PLACEMENT_3D ( 'NONE', #21854, #1076, #6011 ) ;
#15914 = ORIENTED_EDGE ( 'NONE', *, *, #21807, .T. ) ;
#15915 = DIRECTION ( 'NONE',  ( 0.9612616959383221138, 0.2756373558169876170, 0.000000000000000000 ) ) ;
#15916 = DIRECTION ( 'NONE',  ( -1.000000000000000000, 0.000000000000000000, 0.000000000000000000 ) ) ;
#15917 = AXIS2_PLACEMENT_3D ( 'NONE', #24877, #22395, #401 ) ;
#15918 = ORIENTED_EDGE ( 'NONE', *, *, #31944, .T. ) ;
#15919 = AXIS2_PLACEMENT_3D ( 'NONE', #14474, #26774, #26602 ) ;
#15920 = CIRCLE ( 'NONE', #13314, 4.200000000000000178 ) ;
#15921 = ORIENTED_EDGE ( 'NONE', *, *, #7538, .T. ) ;
#15922 = ORIENTED_EDGE ( 'NONE', *, *, #19025, .T. ) ;
#15923 = DIRECTION ( 'NONE',  ( 0.9612616959383207815, 0.2756373558169927240, 8.795445018804291370E-19 ) ) ;
#15924 = CARTESIAN_POINT ( 'NONE',  ( -44.85780503240869876, -5.258343014327087062, 52.53743480612791217 ) ) ;
#15925 = VERTEX_POINT ( 'NONE', #26385 ) ;
#15926 = CARTESIAN_POINT ( 'NONE',  ( 21.09785597605719687, -13.30631372918550959, 102.8621366805641770 ) ) ;
#15927 = CARTESIAN_POINT ( 'NONE',  ( 21.09785597605718976, 6.574714862014670480, 26.91277942630439668 ) ) ;
#15928 = DIRECTION ( 'NONE',  ( -1.224646799147353207E-16, -1.349345573449484691E-32, 1.000000000000000000 ) ) ;
#15929 = ORIENTED_EDGE ( 'NONE', *, *, #17029, .F. ) ;
#15930 = CARTESIAN_POINT ( 'NONE',  ( 21.09992658989239089, 30.34143805560860585, 47.04930799450051637 ) ) ;
#15931 = ADVANCED_FACE ( 'NONE', ( #13919 ), #19549, .T. ) ;
#15932 = VERTEX_POINT ( 'NONE', #8984 ) ;
#15933 = CARTESIAN_POINT ( 'NONE',  ( -42.25266656316760105, 14.76047283463325321, 59.54930799450050927 ) ) ;
#15934 = CARTESIAN_POINT ( 'NONE',  ( 8.823509210239574685, 31.09164230456639544, 47.04930799450051637 ) ) ;
#15936 = AXIS2_PLACEMENT_3D ( 'NONE', #9126, #29306, #6826 ) ;
#15935 = LINE ( 'NONE', #13803, #31073 ) ;
#15937 = CARTESIAN_POINT ( 'NONE',  ( 21.09992658989238734, 31.59164230456639544, 47.04930799450051637 ) ) ;
#15938 = EDGE_CURVE ( 'NONE', #30996, #20780, #21607, .T. ) ;
#15939 = CARTESIAN_POINT ( 'NONE',  ( -40.65740519188835123, 6.815948303523045482, 34.58882370767772585 ) ) ;
#15940 =( NAMED_UNIT ( * ) SI_UNIT ( $, .STERADIAN. ) SOLID_ANGLE_UNIT ( ) );
#15941 = ORIENTED_EDGE ( 'NONE', *, *, #2586, .F. ) ;
#15942 = ORIENTED_EDGE ( 'NONE', *, *, #3110, .F. ) ;
#15943 = DIRECTION ( 'NONE',  ( -1.101824276508909887E-16, 1.000000000000000000, -0.000000000000000000 ) ) ;
#15944 = CARTESIAN_POINT ( 'NONE',  ( 21.09785597605720042, -13.40182760052194588, 47.04930799450051637 ) ) ;
#15945 = CARTESIAN_POINT ( 'NONE',  ( 52.33191709358631272, 3.957035103101695928, 98.60043611252098117 ) ) ;
#15946 = ORIENTED_EDGE ( 'NONE', *, *, #10129, .T. ) ;
#15947 = CARTESIAN_POINT ( 'NONE',  ( 8.474859994195286461, 29.34143805560861296, 47.04930799450051637 ) ) ;
#15948 = CARTESIAN_POINT ( 'NONE',  ( 21.09785597605719332, 11.92558985988973497, 47.04930799450051637 ) ) ;
#15949 = EDGE_LOOP ( 'NONE', ( #3793, #14601, #31692, #24613 ) ) ;
#15950 = CARTESIAN_POINT ( 'NONE',  ( 44.91142894931555674, 28.69787913140503832, 45.63089057098605394 ) ) ;
#15951 = CARTESIAN_POINT ( 'NONE',  ( -39.39870728729693639, -5.936092197299768891, 77.94355715136961749 ) ) ;
#15952 = AXIS2_PLACEMENT_3D ( 'NONE', #11525, #24317, #19056 ) ;
#15953 = TOROIDAL_SURFACE ( 'NONE', #25912, 1.899999999999999467, 0.1000000000000000056 ) ;
#15954 = AXIS2_PLACEMENT_3D ( 'NONE', #28418, #20535, #5931 ) ;
#15955 = TOROIDAL_SURFACE ( 'NONE', #7058, 58.03288776117695846, 0.1999999999999970968 ) ;
#15956 = ORIENTED_EDGE ( 'NONE', *, *, #16441, .F. ) ;
#15957 = FACE_OUTER_BOUND ( 'NONE', #23808, .T. ) ;
#15958 = EDGE_CURVE ( 'NONE', #30715, #23081, #31957, .T. ) ;
#15959 = CARTESIAN_POINT ( 'NONE',  ( 47.03138641870017977, 22.86454579224779948, 49.04855133162938330 ) ) ;
#15960 = ORIENTED_EDGE ( 'NONE', *, *, #8451, .F. ) ;
#15961 = CARTESIAN_POINT ( 'NONE',  ( -40.74365851677129768, 8.439942589813741236, 39.54930799450052348 ) ) ;
#15962 = CARTESIAN_POINT ( 'NONE',  ( 21.09992658989238734, 38.56284415653841791, 47.04930799450051637 ) ) ;
#15963 = CARTESIAN_POINT ( 'NONE',  ( 72.33761410512941836, 5.053071141216427975, 16.47634976544295782 ) ) ;
#15964 = ORIENTED_EDGE ( 'NONE', *, *, #17213, .F. ) ;
#15965 = CARTESIAN_POINT ( 'NONE',  ( -41.96544240928614755, 13.75880317176705603, 54.54930799450051637 ) ) ;
#15966 = EDGE_CURVE ( 'NONE', #9355, #25738, #20080, .T. ) ;
#15967 = CARTESIAN_POINT ( 'NONE',  ( -48.25869185997735400, 10.94158050198885590, 59.53596428539564300 ) ) ;
#15969 = ADVANCED_FACE ( 'NONE', ( #7169 ), #16927, .T. ) ;
#15968 = CARTESIAN_POINT ( 'NONE',  ( 45.18933221474103590, 15.77906836436399374, 43.30797974740836764 ) ) ;
#15970 = VECTOR ( 'NONE', #12346, 1000.000000000000000 ) ;
#15971 = ADVANCED_FACE ( 'NONE', ( #29662 ), #23748, .F. ) ;
#15972 =( BOUNDED_CURVE ( )  B_SPLINE_CURVE ( 3, ( #22306, #4754, #2611, #2775 ),
 .UNSPECIFIED., .F., .F. ) 
 B_SPLINE_CURVE_WITH_KNOTS ( ( 4, 4 ),
 ( 5.062864179022698252, 5.184122060454619429 ),
 .UNSPECIFIED. ) 
 CURVE ( )  GEOMETRIC_REPRESENTATION_ITEM ( )  RATIONAL_B_SPLINE_CURVE ( ( 1.000000000000000000, 0.9987750858034806223, 0.9987750858034806223, 1.000000000000000000 ) ) 
 REPRESENTATION_ITEM ( '' )  );
#15973 = DIRECTION ( 'NONE',  ( -0.8746197071393925215, 0.4848096202463429982, 8.676864087101709653E-18 ) ) ;
#15974 = TOROIDAL_SURFACE ( 'NONE', #17545, 67.99999999999997158, 4.000000000000000000 ) ;
#15975 = EDGE_CURVE ( 'NONE', #13582, #22782, #23229, .T. ) ;
#15976 = EDGE_LOOP ( 'NONE', ( #12383, #12494, #30829, #21008 ) ) ;
#15977 = CARTESIAN_POINT ( 'NONE',  ( 21.09785597605720042, -13.98292989133646103, 47.04930799450051637 ) ) ;
#15978 = CARTESIAN_POINT ( 'NONE',  ( 47.18879033565401215, 29.58872476413164776, 44.97623416235143168 ) ) ;
#15979 = CIRCLE ( 'NONE', #3398, 0.7928932188134565351 ) ;
#15980 = AXIS2_PLACEMENT_3D ( 'NONE', #20781, #28652, #12927 ) ;
#15981 = DIRECTION ( 'NONE',  ( 0.000000000000000000, 0.000000000000000000, -1.000000000000000000 ) ) ;
#15982 = FACE_OUTER_BOUND ( 'NONE', #5465, .T. ) ;
#15983 = VECTOR ( 'NONE', #10816, 1000.000000000000000 ) ;
#15984 = CYLINDRICAL_SURFACE ( 'NONE', #2156, 12.62506659569710443 ) ;
#15985 = ORIENTED_EDGE ( 'NONE', *, *, #30320, .T. ) ;
#15986 = DIRECTION ( 'NONE',  ( 0.000000000000000000, 0.000000000000000000, -1.000000000000000000 ) ) ;
#15987 = DIRECTION ( 'NONE',  ( -0.000000000000000000, -1.000000000000000000, 0.000000000000000000 ) ) ;
#15988 = EDGE_LOOP ( 'NONE', ( #28631, #18443, #29447, #11615 ) ) ;
#15989 = DIRECTION ( 'NONE',  ( -0.7141240004912712269, 0.3958453973320736341, 0.5773502691896451600 ) ) ;
#15990 = CARTESIAN_POINT ( 'NONE',  ( -40.18454328187963398, 7.548069831825862330, 53.64930799450051779 ) ) ;
#15991 = DIRECTION ( 'NONE',  ( -0.000000000000000000, -1.000000000000000000, -0.000000000000000000 ) ) ;
#15992 = DIRECTION ( 'NONE',  ( -1.000000000000000000, 0.000000000000000000, 0.000000000000000000 ) ) ;
#15993 = EDGE_LOOP ( 'NONE', ( #25983, #2955, #27596, #9466 ) ) ;
#15994 = LINE ( 'NONE', #3358, #979 ) ;
#15995 = ORIENTED_EDGE ( 'NONE', *, *, #29460, .T. ) ;
#15996 = EDGE_LOOP ( 'NONE', ( #19124, #9127 ) ) ;
#15997 = CIRCLE ( 'NONE', #28586, 0.1250000000000001110 ) ;
#15998 = TOROIDAL_SURFACE ( 'NONE', #27540, 12.40141737965286062, 0.1249999999999998196 ) ;
#15999 = EDGE_CURVE ( 'NONE', #27032, #2499, #2414, .T. ) ;
#16000 = AXIS2_PLACEMENT_3D ( 'NONE', #1230, #18627, #18782 ) ;
#16001 = ADVANCED_FACE ( 'NONE', ( #4710 ), #1913, .F. ) ;
#16002 = AXIS2_PLACEMENT_3D ( 'NONE', #3867, #21576, #32217 ) ;
#16003 = AXIS2_PLACEMENT_3D ( 'NONE', #14036, #31759, #6483 ) ;
#16004 = DIRECTION ( 'NONE',  ( -0.000000000000000000, -1.000000000000000000, 0.000000000000000000 ) ) ;
#16005 = CARTESIAN_POINT ( 'NONE',  ( -35.00907444222341525, -4.763445661495945060, 80.08276038674898700 ) ) ;
#16006 = CARTESIAN_POINT ( 'NONE',  ( 21.09992658989239089, 25.84184655352419213, 47.04930799450051637 ) ) ;
#16007 = ORIENTED_EDGE ( 'NONE', *, *, #24800, .F. ) ;
#16008 = FACE_OUTER_BOUND ( 'NONE', #15976, .T. ) ;
#16009 = ORIENTED_EDGE ( 'NONE', *, *, #21183, .T. ) ;
#16010 = CARTESIAN_POINT ( 'NONE',  ( 21.09992658989238734, 38.56284415653841791, 47.04930799450051637 ) ) ;
#16011 = FACE_OUTER_BOUND ( 'NONE', #916, .T. ) ;
#16012 = CARTESIAN_POINT ( 'NONE',  ( 21.09785597605720042, -13.64309448858209528, 47.04930799450051637 ) ) ;
#16013 = DIRECTION ( 'NONE',  ( 0.000000000000000000, 0.7071067811865474617, 0.7071067811865475727 ) ) ;
#16014 = ADVANCED_FACE ( 'NONE', ( #14890 ), #9801, .F. ) ;
#16015 = ORIENTED_EDGE ( 'NONE', *, *, #26379, .F. ) ;
#16016 = CARTESIAN_POINT ( 'NONE',  ( -36.90670693849242667, -5.935454207752202116, 16.07118271501078510 ) ) ;
#16017 = ORIENTED_EDGE ( 'NONE', *, *, #2806, .T. ) ;
#16018 = CARTESIAN_POINT ( 'NONE',  ( 33.50134396954521776, 29.34164230456639899, 47.04930799450051637 ) ) ;
#16019 = FACE_OUTER_BOUND ( 'NONE', #11992, .T. ) ;
#16020 = VERTEX_POINT ( 'NONE', #9962 ) ;
#16021 = DIRECTION ( 'NONE',  ( -0.8746197071393926326, 0.4848096202463430537, 8.676864087101709653E-18 ) ) ;
#16022 = DIRECTION ( 'NONE',  ( -1.101824276508909887E-16, 1.000000000000000000, -0.000000000000000000 ) ) ;
#16023 = CARTESIAN_POINT ( 'NONE',  ( 33.46699938050304013, 25.72145308207319303, 47.04930799450050927 ) ) ;
#16024 = SURFACE_STYLE_FILL_AREA ( #28511 ) ;
#16025 = VERTEX_POINT ( 'NONE', #14728 ) ;
#16026 = CARTESIAN_POINT ( 'NONE',  ( 48.22193606911519481, 23.04411619146717882, 47.10768726602483980 ) ) ;
#16027 = CARTESIAN_POINT ( 'NONE',  ( -40.61337426079494151, 6.957937756950597574, 35.07960045310107233 ) ) ;
#16028 = ORIENTED_EDGE ( 'NONE', *, *, #10546, .T. ) ;
#16029 = CARTESIAN_POINT ( 'NONE',  ( -12.90214402394279603, 13.86454579224779948, 47.04930799450052348 ) ) ;
#16030 = AXIS2_PLACEMENT_3D ( 'NONE', #3173, #28772, #20582 ) ;
#16031 = DIRECTION ( 'NONE',  ( 0.000000000000000000, 0.000000000000000000, -1.000000000000000000 ) ) ;
#16032 = EDGE_LOOP ( 'NONE', ( #20526, #28107, #19180, #22738, #3898 ) ) ;
#16033 = EDGE_CURVE ( 'NONE', #28369, #20933, #21929, .T. ) ;
#16034 = VERTEX_POINT ( 'NONE', #27183 ) ;
#16035 = CARTESIAN_POINT ( 'NONE',  ( -12.58835873576790121, -1.823725651226728584, 101.7951854207034614 ) ) ;
#16036 = EDGE_CURVE ( 'NONE', #26371, #22928, #5937, .T. ) ;
#16037 = TOROIDAL_SURFACE ( 'NONE', #28089, 0.2000000000000000111, 0.1000000000000000056 ) ;
#16038 = ORIENTED_EDGE ( 'NONE', *, *, #6710, .F. ) ;
#16039 = ADVANCED_FACE ( 'NONE', ( #7667 ), #27959, .F. ) ;
#16040 = EDGE_CURVE ( 'NONE', #12208, #20299, #24273, .T. ) ;
#16041 = EDGE_CURVE ( 'NONE', #19917, #8660, #4363, .T. ) ;
#16042 = ORIENTED_EDGE ( 'NONE', *, *, #26386, .T. ) ;
#16043 = DIRECTION ( 'NONE',  ( 0.000000000000000000, 0.000000000000000000, -1.000000000000000000 ) ) ;
#16044 = CIRCLE ( 'NONE', #19700, 0.1000000000000018235 ) ;
#16045 = PRESENTATION_LAYER_ASSIGNMENT (  '', '', ( #20765 ) ) ;
#16046 = ORIENTED_EDGE ( 'NONE', *, *, #31584, .T. ) ;
#16047 = CARTESIAN_POINT ( 'NONE',  ( 48.22193606911519481, 23.04411619146717882, 47.10768726602483980 ) ) ;
#16048 = FACE_OUTER_BOUND ( 'NONE', #22140, .T. ) ;
#16049 = CARTESIAN_POINT ( 'NONE',  ( 49.44739180854976013, 28.73456182964376282, 47.17133137409169308 ) ) ;
#16050 = ADVANCED_FACE ( 'NONE', ( #24562 ), #124, .T. ) ;
#16051 = VERTEX_POINT ( 'NONE', #27681 ) ;
#16052 = ORIENTED_EDGE ( 'NONE', *, *, #6004, .T. ) ;
#16053 = DIRECTION ( 'NONE',  ( 0.000000000000000000, 0.000000000000000000, 1.000000000000000000 ) ) ;
#16054 = ORIENTED_EDGE ( 'NONE', *, *, #5799, .F. ) ;
#16055 = AXIS2_PLACEMENT_3D ( 'NONE', #28002, #30784, #25533 ) ;
#16056 = DIRECTION ( 'NONE',  ( 1.000000000000000000, 0.000000000000000000, 0.000000000000000000 ) ) ;
#16057 = CARTESIAN_POINT ( 'NONE',  ( -40.69332644341266558, 6.790879890547247832, 39.41319887685486378 ) ) ;
#16058 = CARTESIAN_POINT ( 'NONE',  ( -6.902144023942790696, -5.098646251524523443, 47.04930799450052348 ) ) ;
#16059 = CARTESIAN_POINT ( 'NONE',  ( 21.09785597605719332, 14.77310068074637961, 47.04930799450051637 ) ) ;
#16060 = EDGE_LOOP ( 'NONE', ( #19816, #25946, #13500, #21225 ) ) ;
#16061 = CARTESIAN_POINT ( 'NONE',  ( 21.09785597605719332, 30.56454579224779522, 47.04930799450051637 ) ) ;
#16062 = CARTESIAN_POINT ( 'NONE',  ( -40.02540636251514172, 2.839176264122877047, 55.74930799450051211 ) ) ;
#16063 = CARTESIAN_POINT ( 'NONE',  ( -40.15599670534037102, 7.478908884098772525, 34.64930799450051779 ) ) ;
#16064 = CARTESIAN_POINT ( 'NONE',  ( 48.54365229441402363, 22.98879437201065912, 46.79176277441978016 ) ) ;
#16065 = CARTESIAN_POINT ( 'NONE',  ( 21.09785597605719332, 14.86454579224779948, 47.04930799450051637 ) ) ;
#16066 = CARTESIAN_POINT ( 'NONE',  ( 49.49063479933183629, 25.99951373492759998, 47.17357720316391578 ) ) ;
#16067 = EDGE_CURVE ( 'NONE', #25102, #13126, #11724, .T. ) ;
#16068 = VERTEX_POINT ( 'NONE', #7336 ) ;
#16069 = DIRECTION ( 'NONE',  ( 0.000000000000000000, -1.000000000000000000, -0.000000000000000000 ) ) ;
#16070 = DIRECTION ( 'NONE',  ( -1.000000000000000000, 0.000000000000000000, 0.000000000000000000 ) ) ;
#16071 = TOROIDAL_SURFACE ( 'NONE', #5068, 46.69263079098917046, 1.200000000000001954 ) ;
#16072 = EDGE_CURVE ( 'NONE', #4922, #9470, #23245, .T. ) ;
#16073 = ORIENTED_EDGE ( 'NONE', *, *, #29076, .T. ) ;
#16074 = EDGE_CURVE ( 'NONE', #12012, #31925, #270, .T. ) ;
#16075 = CIRCLE ( 'NONE', #24467, 67.18681090792816235 ) ;
#16076 = EDGE_CURVE ( 'NONE', #321, #18497, #6393, .T. ) ;
#16077 = ORIENTED_EDGE ( 'NONE', *, *, #13854, .T. ) ;
#16078 = CARTESIAN_POINT ( 'NONE',  ( 33.50134396954527460, 24.09164230456639544, 47.04930799450051637 ) ) ;
#16079 = CARTESIAN_POINT ( 'NONE',  ( 33.72499318558949710, 27.09184655352419568, 47.04930799450051637 ) ) ;
#16080 = DIRECTION ( 'NONE',  ( -1.000000000000000000, -1.101824276508909887E-16, 0.000000000000000000 ) ) ;
#16081 = ORIENTED_EDGE ( 'NONE', *, *, #11629, .F. ) ;
#16082 = DIRECTION ( 'NONE',  ( -0.000000000000000000, -1.000000000000000000, 0.000000000000000000 ) ) ;
#16083 = DIRECTION ( 'NONE',  ( -1.101824276508909887E-16, 1.000000000000000000, -0.000000000000000000 ) ) ;
#16084 = DIRECTION ( 'NONE',  ( -1.000000000000000000, 0.000000000000000000, 0.000000000000000000 ) ) ;
#16085 = AXIS2_PLACEMENT_3D ( 'NONE', #9984, #15660, #10599 ) ;
#16086 = EDGE_LOOP ( 'NONE', ( #16488, #25924, #31141, #24271 ) ) ;
#16087 = DIRECTION ( 'NONE',  ( -1.101824276508909887E-16, 1.000000000000000000, -0.000000000000000000 ) ) ;
#16088 = ORIENTED_EDGE ( 'NONE', *, *, #21689, .T. ) ;
#16089 = FACE_OUTER_BOUND ( 'NONE', #5047, .T. ) ;
#16090 = DIRECTION ( 'NONE',  ( 0.000000000000000000, 1.000000000000000000, 0.000000000000000000 ) ) ;
#16091 = CARTESIAN_POINT ( 'NONE',  ( 21.09992658989239089, 28.84184655352418858, 47.04930799450051637 ) ) ;
#16092 = CYLINDRICAL_SURFACE ( 'NONE', #14712, 12.36707279061065101 ) ;
#16093 = ORIENTED_EDGE ( 'NONE', *, *, #17618, .F. ) ;
#16094 = ORIENTED_EDGE ( 'NONE', *, *, #23271, .T. ) ;
#16095 = CARTESIAN_POINT ( 'NONE',  ( 8.732853799281725671, 26.22145308207318593, 47.04930799450051637 ) ) ;
#16096 = CARTESIAN_POINT ( 'NONE',  ( -42.76364231915344050, 15.12166775071173852, 38.44930799450052206 ) ) ;
#16097 = CARTESIAN_POINT ( 'NONE',  ( 21.09785597605719332, -9.935454207752199451, 47.04930799450051637 ) ) ;
#16098 = ORIENTED_EDGE ( 'NONE', *, *, #19053, .T. ) ;
#16099 = CARTESIAN_POINT ( 'NONE',  ( 33.71785032049133690, 28.46664230456639899, 47.04930799450051637 ) ) ;
#16100 = CARTESIAN_POINT ( 'NONE',  ( -40.11286833322907341, 2.887657226147507306, 37.04930799450052348 ) ) ;
#16101 = B_SPLINE_CURVE_WITH_KNOTS ( 'NONE', 3,
 ( #308, #19514, #15088, #17211, #20004, #7548, #30034, #151, #27402, #10170, #15251, #29546 ),
 .UNSPECIFIED., .F., .F.,
 ( 4, 2, 2, 2, 2, 4 ),
 ( 0.0003078418816934435655, 0.0003848023521168015431, 0.0004232825873284805319, 0.0004617628225401594665, 0.0005387232929635211304, 0.0006156837633868826858 ),
 .UNSPECIFIED. ) ;
#16102 = VERTEX_POINT ( 'NONE', #10936 ) ;
#16103 = CARTESIAN_POINT ( 'NONE',  ( 47.09785597605719687, 24.86454579224779948, 49.54930799450042400 ) ) ;
#16104 = CARTESIAN_POINT ( 'NONE',  ( 45.73035263060504718, 29.33954579807170404, 44.36855633853329550 ) ) ;
#16105 = DIRECTION ( 'NONE',  ( -0.000000000000000000, -1.000000000000000000, 0.000000000000000000 ) ) ;
#16106 = AXIS2_PLACEMENT_3D ( 'NONE', #5767, #15774, #23645 ) ;
#16107 = TOROIDAL_SURFACE ( 'NONE', #20305, 12.40141737965285174, 0.1249999999999993200 ) ;
#16108 = VECTOR ( 'NONE', #17927, 1000.000000000000000 ) ;
#16109 = CIRCLE ( 'NONE', #1961, 13.20000000000000284 ) ;
#16110 = EDGE_CURVE ( 'NONE', #19824, #8349, #30793, .T. ) ;
#16111 = ORIENTED_EDGE ( 'NONE', *, *, #7905, .F. ) ;
#16112 = EDGE_CURVE ( 'NONE', #1878, #5045, #10667, .T. ) ;
#16113 = VECTOR ( 'NONE', #17636, 1000.000000000000000 ) ;
#16114 = DIRECTION ( 'NONE',  ( 0.000000000000000000, 0.000000000000000000, 1.000000000000000000 ) ) ;
#16115 = CARTESIAN_POINT ( 'NONE',  ( -40.50146157965988891, 7.595301493077382560, 38.66054537865625917 ) ) ;
#16116 = DIRECTION ( 'NONE',  ( -1.000000000000000000, 0.000000000000000000, 0.000000000000000000 ) ) ;
#16117 = AXIS2_PLACEMENT_3D ( 'NONE', #13244, #10928, #23873 ) ;
#16118 = ORIENTED_EDGE ( 'NONE', *, *, #1705, .F. ) ;
#16119 = CARTESIAN_POINT ( 'NONE',  ( 21.09992658989238734, 38.56284415653841791, 47.04930799450051637 ) ) ;
#16120 = DIRECTION ( 'NONE',  ( -1.101824276508909887E-16, 1.000000000000000000, -0.000000000000000000 ) ) ;
#16121 = DIRECTION ( 'NONE',  ( 0.4848096202463673676, 0.8746197071393789768, 0.000000000000000000 ) ) ;
#16122 = ORIENTED_EDGE ( 'NONE', *, *, #25570, .F. ) ;
#16123 = CARTESIAN_POINT ( 'NONE',  ( -4.902144023942810236, 25.56454579224779877, 47.04930799450078638 ) ) ;
#16124 = LINE ( 'NONE', #15967, #15224 ) ;
#16125 = DIRECTION ( 'NONE',  ( 0.000000000000000000, 0.000000000000000000, 1.000000000000000000 ) ) ;
#16126 = PRESENTATION_STYLE_ASSIGNMENT (( #6126 ) ) ;
#16127 = ORIENTED_EDGE ( 'NONE', *, *, #22990, .T. ) ;
#16128 = DIRECTION ( 'NONE',  ( -1.101824276508909887E-16, 1.000000000000000000, -0.000000000000000000 ) ) ;
#16129 = DIRECTION ( 'NONE',  ( -1.000000000000000000, 0.000000000000000000, 0.000000000000000000 ) ) ;
#16130 = CIRCLE ( 'NONE', #939, 13.20000000000000995 ) ;
#16131 = CARTESIAN_POINT ( 'NONE',  ( 21.09992658989238734, 31.09164230456639544, 47.04930799450051637 ) ) ;
#16132 = CARTESIAN_POINT ( 'NONE',  ( 8.474859994195282908, 38.56284415653841791, 47.04930799450051637 ) ) ;
#16133 = AXIS2_PLACEMENT_3D ( 'NONE', #26476, #8440, #28618 ) ;
#16134 = CARTESIAN_POINT ( 'NONE',  ( 106.0978559760573887, -5.935454207752198563, 77.87546120947926909 ) ) ;
#16135 = ORIENTED_EDGE ( 'NONE', *, *, #28030, .T. ) ;
#16136 = DIRECTION ( 'NONE',  ( -0.000000000000000000, -1.000000000000000000, 0.000000000000000000 ) ) ;
#16137 = DIRECTION ( 'NONE',  ( 0.000000000000000000, 0.000000000000000000, -1.000000000000000000 ) ) ;
#16138 = DIRECTION ( 'NONE',  ( 0.4848096202463424986, 0.8746197071393928546, -2.220446049250312834E-16 ) ) ;
#16139 = AXIS2_PLACEMENT_3D ( 'NONE', #17759, #27777, #5302 ) ;
#16140 = ORIENTED_EDGE ( 'NONE', *, *, #5496, .T. ) ;
#16141 = DIRECTION ( 'NONE',  ( 1.000000000000000000, 0.000000000000000000, 0.000000000000000000 ) ) ;
#16142 = DIRECTION ( 'NONE',  ( -0.000000000000000000, 1.000000000000000000, -0.000000000000000000 ) ) ;
#16143 = CARTESIAN_POINT ( 'NONE',  ( 52.75656117287782365, 3.230235421722231326, -5.651282540884040806 ) ) ;
#16144 = EDGE_LOOP ( 'NONE', ( #13913, #4082, #20845, #7456 ) ) ;
#16145 = CARTESIAN_POINT ( 'NONE',  ( 48.55356409855115629, 22.86454579224779593, 48.48022381235000466 ) ) ;
#16146 = ORIENTED_EDGE ( 'NONE', *, *, #10409, .T. ) ;
#16147 = ORIENTED_EDGE ( 'NONE', *, *, #27476, .T. ) ;
#16148 = ADVANCED_FACE ( 'NONE', ( #17826 ), #3320, .T. ) ;
#16149 = EDGE_CURVE ( 'NONE', #28443, #5065, #27849, .T. ) ;
#16150 = ADVANCED_FACE ( 'NONE', ( #22911 ), #24225, .F. ) ;
#16151 = ADVANCED_FACE ( 'NONE', ( #25863 ), #14651, .T. ) ;
#16152 = CIRCLE ( 'NONE', #14064, 67.18681090792816235 ) ;
#16153 = CIRCLE ( 'NONE', #9347, 85.00000000000001421 ) ;
#16154 = AXIS2_PLACEMENT_3D ( 'NONE', #20026, #7411, #12 ) ;
#16155 = AXIS2_PLACEMENT_3D ( 'NONE', #4281, #16577, #19529 ) ;
#16156 =( BOUNDED_CURVE ( )  B_SPLINE_CURVE ( 2, ( #20868, #17929, #25639, #3635, #31057, #18086, #25953, #18557, #852 ),
 .UNSPECIFIED., .F., .F. ) 
 B_SPLINE_CURVE_WITH_KNOTS ( ( 3, 2, 2, 2, 3 ),
 ( 0.6071428559815844617, 0.6190476190476190688, 0.6428571428571427937, 0.6666666666666667407, 0.6785714274101559695 ),
 .UNSPECIFIED. ) 
 CURVE ( )  GEOMETRIC_REPRESENTATION_ITEM ( )  RATIONAL_B_SPLINE_CURVE ( ( 0.9330127018922200755, 0.9330126953578157245, 1.000000000000000000, 0.8660254037844387076, 1.000000000000000000, 0.8660254037844387076, 1.000000000000000000, 0.9330127084266226500, 0.9330127018922199644 ) ) 
 REPRESENTATION_ITEM ( '' )  );
#16157 = AXIS2_PLACEMENT_3D ( 'NONE', #445, #18487, #30500 ) ;
#16159 = CARTESIAN_POINT ( 'NONE',  ( 33.46699938050303302, 38.56284415653841791, 47.04930799450051637 ) ) ;
#16158 = B_SPLINE_CURVE_WITH_KNOTS ( 'NONE', 3,
 ( #24441, #1310, #26581, #11332, #13963, #9027, #9193, #31358 ),
 .UNSPECIFIED., .F., .F.,
 ( 4, 2, 2, 4 ),
 ( 0.000000000000000000, 0.0005384193795069787359, 0.0008076290692604753138, 0.001076838759013972000 ),
 .UNSPECIFIED. ) ;
#16160 = CARTESIAN_POINT ( 'NONE',  ( 21.09785597605720042, -13.68834655544033652, 47.04930799450051637 ) ) ;
#16161 = DIRECTION ( 'NONE',  ( 0.9612616959383221138, 0.2756373558169876170, 0.000000000000000000 ) ) ;
#16162 = ORIENTED_EDGE ( 'NONE', *, *, #19059, .F. ) ;
#16163 = CYLINDRICAL_SURFACE ( 'NONE', #6184, 0.1000000000000008243 ) ;
#16164 = ORIENTED_EDGE ( 'NONE', *, *, #5002, .T. ) ;
#16165 = CARTESIAN_POINT ( 'NONE',  ( 33.46699938050304013, 29.47145308207317882, 47.04930799450050927 ) ) ;
#16166 = CARTESIAN_POINT ( 'NONE',  ( 8.474859994195286461, 30.59143805560860585, 47.04930799450051637 ) ) ;
#16167 = EDGE_CURVE ( 'NONE', #5653, #490, #30591, .T. ) ;
#16168 = DIRECTION ( 'NONE',  ( -2.779292025043186357E-18, 1.288349127009862211E-17, -1.000000000000000000 ) ) ;
#16169 = VERTEX_POINT ( 'NONE', #1841 ) ;
#16170 = FACE_OUTER_BOUND ( 'NONE', #29956, .T. ) ;
#16171 = CARTESIAN_POINT ( 'NONE',  ( -40.28779227465695811, 2.984619150196779369, 55.04930799450051637 ) ) ;
#16172 = DIRECTION ( 'NONE',  ( -0.4848096202463429427, -0.8746197071393925215, 2.352477780477436787E-16 ) ) ;
#16173 = LINE ( 'NONE', #13258, #18987 ) ;
#16174 = ORIENTED_EDGE ( 'NONE', *, *, #20234, .F. ) ;
#16175 = CARTESIAN_POINT ( 'NONE',  ( 47.19823469859255738, 22.88065857334294861, 45.11653766655789610 ) ) ;
#16176 = CARTESIAN_POINT ( 'NONE',  ( 21.09992658989238734, 38.56284415653841791, 47.04930799450051637 ) ) ;
#16177 = FACE_OUTER_BOUND ( 'NONE', #21362, .T. ) ;
#16178 = CARTESIAN_POINT ( 'NONE',  ( 48.40186567930498285, 26.02957786121582373, 45.03923535223908203 ) ) ;
#16179 = ORIENTED_EDGE ( 'NONE', *, *, #27387, .T. ) ;
#16180 = CARTESIAN_POINT ( 'NONE',  ( 21.09992658989238734, 32.09184655352418503, 47.04930799450051637 ) ) ;
#16181 = CARTESIAN_POINT ( 'NONE',  ( 21.09992658989238734, 38.56284415653841791, 47.04930799450051637 ) ) ;
#16182 = ORIENTED_EDGE ( 'NONE', *, *, #2403, .F. ) ;
#16184 = EDGE_CURVE ( 'NONE', #21016, #2064, #11700, .T. ) ;
#16183 = DIRECTION ( 'NONE',  ( -1.101824276508909887E-16, 1.000000000000000000, -0.000000000000000000 ) ) ;
#16185 = TOROIDAL_SURFACE ( 'NONE', #26136, 12.40141737965284108, 0.1249999999999997918 ) ;
#16186 = CIRCLE ( 'NONE', #24573, 0.1249999999999966416 ) ;
#16187 = PLANE ( 'NONE',  #23205 ) ;
#16188 = AXIS2_PLACEMENT_3D ( 'NONE', #8243, #13811, #18550 ) ;
#16189 = VERTEX_POINT ( 'NONE', #16601 ) ;
#16190 = ORIENTED_EDGE ( 'NONE', *, *, #25532, .F. ) ;
#16191 = AXIS2_PLACEMENT_3D ( 'NONE', #19820, #29851, #4405 ) ;
#16192 = ORIENTED_EDGE ( 'NONE', *, *, #6933, .T. ) ;
#16193 = EDGE_CURVE ( 'NONE', #32110, #7566, #30073, .T. ) ;
#16194 = ORIENTED_EDGE ( 'NONE', *, *, #13754, .T. ) ;
#16195 = CYLINDRICAL_SURFACE ( 'NONE', #12315, 0.09999999999999945044 ) ;
#16196 = AXIS2_PLACEMENT_3D ( 'NONE', #26342, #16323, #16492 ) ;
#16197 = AXIS2_PLACEMENT_3D ( 'NONE', #7806, #18445, #11080 ) ;
#16198 = ORIENTED_EDGE ( 'NONE', *, *, #24557, .T. ) ;
#16199 = DIRECTION ( 'NONE',  ( -1.101824276508909887E-16, 1.000000000000000000, -0.000000000000000000 ) ) ;
#16200 = CARTESIAN_POINT ( 'NONE',  ( -4.902144023942810236, 24.86454579224779948, 47.04930799450078638 ) ) ;
#16201 = CARTESIAN_POINT ( 'NONE',  ( 21.09785597605719332, 30.56454579224779522, 75.54930799450052348 ) ) ;
#16202 = ADVANCED_FACE ( 'NONE', ( #6766 ), #20029, .T. ) ;
#16203 = CARTESIAN_POINT ( 'NONE',  ( 46.02876340639226527, 28.26789516297709071, 44.95353858666495483 ) ) ;
#16204 = EDGE_LOOP ( 'NONE', ( #7733, #4685 ) ) ;
#16205 = ORIENTED_EDGE ( 'NONE', *, *, #13837, .F. ) ;
#16206 = DIRECTION ( 'NONE',  ( 0.8746197071393925215, -0.4848096202463429982, -8.676864087101708112E-18 ) ) ;
#16207 = ORIENTED_EDGE ( 'NONE', *, *, #27458, .T. ) ;
#16209 = EDGE_CURVE ( 'NONE', #2007, #7282, #31631, .T. ) ;
#16208 = CARTESIAN_POINT ( 'NONE',  ( 49.17081279531085158, 29.55164023231963455, 46.60812646017934213 ) ) ;
#16210 = VECTOR ( 'NONE', #10764, 1000.000000000000114 ) ;
#16211 = CARTESIAN_POINT ( 'NONE',  ( -40.70323106273436053, 6.774493230553227718, 39.52357759537398607 ) ) ;
#16212 = CARTESIAN_POINT ( 'NONE',  ( 21.09785597605718621, 77.37241625295546044, -36.90555089683208223 ) ) ;
#16213 = DIRECTION ( 'NONE',  ( 0.000000000000000000, 1.000000000000000000, 0.000000000000000000 ) ) ;
#16214 = VECTOR ( 'NONE', #24266, 1000.000000000000000 ) ;
#16215 = CARTESIAN_POINT ( 'NONE',  ( -5.148203073178546418, 10.06999148276586808, -4.322672743066429568 ) ) ;
#16216 = CARTESIAN_POINT ( 'NONE',  ( 21.09992658989239089, 29.72145308207318237, 47.04930799450051637 ) ) ;
#16217 = EDGE_LOOP ( 'NONE', ( #9929, #12427, #11964, #7564 ) ) ;
#16218 = CARTESIAN_POINT ( 'NONE',  ( 33.46699938050303302, 38.56284415653841791, 47.04930799450051637 ) ) ;
#16220 = ADVANCED_FACE ( 'NONE', ( #29247 ), #24747, .F. ) ;
#16219 = DIRECTION ( 'NONE',  ( -0.000000000000000000, -1.000000000000000000, 0.000000000000000000 ) ) ;
#16221 = DIRECTION ( 'NONE',  ( -1.101824276508909887E-16, 1.000000000000000000, -0.000000000000000000 ) ) ;
#16222 = EDGE_CURVE ( 'NONE', #27140, #31848, #27440, .T. ) ;
#16223 = CARTESIAN_POINT ( 'NONE',  ( 46.34827318194108159, 20.53597436367636675, 45.57988155192556690 ) ) ;
#16224 = DIRECTION ( 'NONE',  ( -1.188208965918165239E-16, -1.880121038077813132E-16, -1.000000000000000000 ) ) ;
#16225 = ORIENTED_EDGE ( 'NONE', *, *, #3298, .F. ) ;
#16226 = ORIENTED_EDGE ( 'NONE', *, *, #2929, .F. ) ;
#16227 = CARTESIAN_POINT ( 'NONE',  ( 21.09785597605719332, 25.56454579224779877, 18.54930799450050927 ) ) ;
#16228 = CARTESIAN_POINT ( 'NONE',  ( -40.73091736380679606, 9.483895492497156354, 35.44930799450052206 ) ) ;
#16229 = AXIS2_PLACEMENT_3D ( 'NONE', #10099, #17470, #29787 ) ;
#16230 = AXIS2_PLACEMENT_3D ( 'NONE', #12210, #16947, #9905 ) ;
#16231 = EDGE_LOOP ( 'NONE', ( #16637, #2275, #9918, #4739 ) ) ;
#16232 = EDGE_CURVE ( 'NONE', #17298, #4462, #29091, .T. ) ;
#16233 = AXIS2_PLACEMENT_3D ( 'NONE', #9248, #26807, #31579 ) ;
#16234 = CIRCLE ( 'NONE', #5782, 12.27641737965288193 ) ;
#16235 = TOROIDAL_SURFACE ( 'NONE', #7868, 46.67448298906162307, 0.7000000000000006217 ) ;
#16236 = ORIENTED_EDGE ( 'NONE', *, *, #20814, .F. ) ;
#16237 = AXIS2_PLACEMENT_3D ( 'NONE', #21293, #14254, #24249 ) ;
#16238 = CARTESIAN_POINT ( 'NONE',  ( -41.13825658839732569, 9.453274076459845077, 38.50788663826321567 ) ) ;
#16239 = AXIS2_PLACEMENT_3D ( 'NONE', #18919, #26324, #9086 ) ;
#16240 = CYLINDRICAL_SURFACE ( 'NONE', #19681, 0.1000000000000020595 ) ;
#16241 = DIRECTION ( 'NONE',  ( -1.000000000000000000, 0.000000000000000000, 0.000000000000000000 ) ) ;
#16242 = ORIENTED_EDGE ( 'NONE', *, *, #9066, .T. ) ;
#16243 = CARTESIAN_POINT ( 'NONE',  ( 3.114080794088308846, -13.30632128221581034, -5.912965210926084403 ) ) ;
#16244 = DIRECTION ( 'NONE',  ( -0.8746197071393926326, 0.4848096202463430537, 8.676864087101709653E-18 ) ) ;
#16245 = EDGE_CURVE ( 'NONE', #32203, #11810, #24162, .T. ) ;
#16246 = ORIENTED_EDGE ( 'NONE', *, *, #15431, .F. ) ;
#16247 = CIRCLE ( 'NONE', #7886, 12.62506659569710443 ) ;
#16248 = ORIENTED_EDGE ( 'NONE', *, *, #13354, .F. ) ;
#16249 = EDGE_CURVE ( 'NONE', #313, #6650, #10089, .T. ) ;
#16250 = DIRECTION ( 'NONE',  ( 1.000000000000000000, 0.000000000000000000, 1.224646799147353207E-16 ) ) ;
#16251 = DIRECTION ( 'NONE',  ( -1.000000000000000000, 0.000000000000000000, 0.000000000000000000 ) ) ;
#16252 = DIRECTION ( 'NONE',  ( 0.9612616959383194493, 0.2756373558169974980, 8.795445018804946186E-19 ) ) ;
#16253 = VERTEX_POINT ( 'NONE', #19394 ) ;
#16254 = EDGE_LOOP ( 'NONE', ( #23147, #10561, #23590, #2778 ) ) ;
#16255 = LINE ( 'NONE', #26594, #3977 ) ;
#16256 = DIRECTION ( 'NONE',  ( -0.000000000000000000, -1.000000000000000000, 0.000000000000000000 ) ) ;
#16257 = EDGE_CURVE ( 'NONE', #8095, #30111, #17406, .T. ) ;
#16258 = CONICAL_SURFACE ( 'NONE', #27251, 67.36417311134205477, 1.291543646476234874 ) ;
#16259 = CIRCLE ( 'NONE', #11559, 16.99999999999999289 ) ;
#16260 = ADVANCED_FACE ( 'NONE', ( #6929 ), #7534, .T. ) ;
#16261 = CARTESIAN_POINT ( 'NONE',  ( -10.27276115262104561, -5.884593569754286158, 106.2621915093639871 ) ) ;
#16262 = VERTEX_POINT ( 'NONE', #31562 ) ;
#16263 = DIRECTION ( 'NONE',  ( -1.000000000000000000, -1.101824276508909887E-16, 0.000000000000000000 ) ) ;
#16264 = VECTOR ( 'NONE', #16412, 1000.000000000000000 ) ;
#16265 = CARTESIAN_POINT ( 'NONE',  ( 33.46699938050303302, 38.56284415653841791, 47.04930799450051637 ) ) ;
#16266 = ORIENTED_EDGE ( 'NONE', *, *, #16890, .F. ) ;
#16267 = FACE_OUTER_BOUND ( 'NONE', #31598, .T. ) ;
#16268 = AXIS2_PLACEMENT_3D ( 'NONE', #21683, #22417, #14561 ) ;
#16269 = CARTESIAN_POINT ( 'NONE',  ( 50.10320668408830613, 29.80621246473836905, 47.20539118556276037 ) ) ;
#16270 = VECTOR ( 'NONE', #2356, 1000.000000000000114 ) ;
#16271 = AXIS2_PLACEMENT_3D ( 'NONE', #6501, #4360, #31454 ) ;
#16272 = DIRECTION ( 'NONE',  ( -1.000000000000000000, 0.000000000000000000, 0.000000000000000000 ) ) ;
#16273 = AXIS2_PLACEMENT_3D ( 'NONE', #21618, #14252, #31651 ) ;
#16274 = ORIENTED_EDGE ( 'NONE', *, *, #6351, .F. ) ;
#16275 = DIRECTION ( 'NONE',  ( -1.000000000000000000, -1.101824276508909887E-16, 0.000000000000000000 ) ) ;
#16276 = DIRECTION ( 'NONE',  ( -2.779292025043186357E-18, 1.288349127009862211E-17, -1.000000000000000000 ) ) ;
#16277 = CARTESIAN_POINT ( 'NONE',  ( 46.99023568444673060, 29.32451373492759217, 49.12151524109405898 ) ) ;
#16278 = AXIS2_PLACEMENT_3D ( 'NONE', #19111, #23730, #18633 ) ;
#16279 = ORIENTED_EDGE ( 'NONE', *, *, #15042, .T. ) ;
#16280 = AXIS2_PLACEMENT_3D ( 'NONE', #23765, #6212, #13608 ) ;
#16281 = CONICAL_SURFACE ( 'NONE', #10548, 72.00502525316939284, 0.7853981633974482790 ) ;
#16282 = FACE_OUTER_BOUND ( 'NONE', #23170, .T. ) ;
#16283 = CARTESIAN_POINT ( 'NONE',  ( 33.37634396954521065, 29.84164230456639899, 47.04930799450051637 ) ) ;
#16284 = EDGE_CURVE ( 'NONE', #1905, #11711, #21693, .T. ) ;
#16285 = AXIS2_PLACEMENT_3D ( 'NONE', #21088, #3534, #10626 ) ;
#16286 = DIRECTION ( 'NONE',  ( -1.000000000000000000, -1.101824276508909764E-16, 0.000000000000000000 ) ) ;
#16287 = AXIS2_PLACEMENT_3D ( 'NONE', #15344, #8442, #3347 ) ;
#16288 = VERTEX_POINT ( 'NONE', #17094 ) ;
#16289 = CARTESIAN_POINT ( 'NONE',  ( 8.698509210239533829, 26.84164230456639899, 47.04930799450051637 ) ) ;
#16290 = DIRECTION ( 'NONE',  ( 0.000000000000000000, -0.000000000000000000, -1.000000000000000000 ) ) ;
#16291 = CARTESIAN_POINT ( 'NONE',  ( -39.64148344771002286, 7.657122216028890982, 62.04930799450052348 ) ) ;
#16292 = CARTESIAN_POINT ( 'NONE',  ( 21.09785597605720753, -13.64309448858209528, 105.9390803697710339 ) ) ;
#16293 = VERTEX_POINT ( 'NONE', #9068 ) ;
#16294 = DIRECTION ( 'NONE',  ( 0.000000000000000000, 0.000000000000000000, -1.000000000000000000 ) ) ;
#16295 = CARTESIAN_POINT ( 'NONE',  ( 45.79384627280941800, 26.37957786121582160, 49.05938063676250493 ) ) ;
#16296 = CIRCLE ( 'NONE', #6889, 1.003191532947548925 ) ;
#16297 = CARTESIAN_POINT ( 'NONE',  ( 21.09992658989239089, 29.96183152705961206, 47.04930799450051637 ) ) ;
#16298 = EDGE_CURVE ( 'NONE', #12727, #3952, #22657, .T. ) ;
#16299 = CARTESIAN_POINT ( 'NONE',  ( -40.12425944110432852, 6.890664497466326033, 34.56792418805707712 ) ) ;
#16300 = CARTESIAN_POINT ( 'NONE',  ( 21.09785597605719332, 11.92558985988973497, 102.9072182181210451 ) ) ;
#16301 = ORIENTED_EDGE ( 'NONE', *, *, #19208, .T. ) ;
#16302 = FACE_OUTER_BOUND ( 'NONE', #1288, .T. ) ;
#16303 = CARTESIAN_POINT ( 'NONE',  ( -44.85737707344571135, -5.257416160756734236, 41.56220475672508741 ) ) ;
#16304 = CYLINDRICAL_SURFACE ( 'NONE', #30409, 12.36707279061065101 ) ;
#16305 = ORIENTED_EDGE ( 'NONE', *, *, #28401, .T. ) ;
#16306 = CARTESIAN_POINT ( 'NONE',  ( 60.59785597605719687, 13.86454579224779948, 47.04930799450051637 ) ) ;
#16307 = LINE ( 'NONE', #23538, #5748 ) ;
#16308 = CARTESIAN_POINT ( 'NONE',  ( 21.09785597605720753, 14.99513937955032716, 47.04930799450052348 ) ) ;
#16309 = DIRECTION ( 'NONE',  ( -1.000000000000000000, -1.101824276508909887E-16, 0.000000000000000000 ) ) ;
#16310 = ORIENTED_EDGE ( 'NONE', *, *, #31702, .T. ) ;
#16311 = CARTESIAN_POINT ( 'NONE',  ( 73.54853330490307428, 11.86909835304794392, 25.53840420133489175 ) ) ;
#16312 = AXIS2_PLACEMENT_3D ( 'NONE', #22731, #19608, #2392 ) ;
#16313 = VERTEX_POINT ( 'NONE', #9561 ) ;
#16314 = AXIS2_PLACEMENT_3D ( 'NONE', #1924, #20137, #32302 ) ;
#16315 = ORIENTED_EDGE ( 'NONE', *, *, #13751, .F. ) ;
#16316 = AXIS2_PLACEMENT_3D ( 'NONE', #18312, #27689, #8002 ) ;
#16317 = DIRECTION ( 'NONE',  ( 0.000000000000000000, 0.000000000000000000, 1.000000000000000000 ) ) ;
#16318 = CARTESIAN_POINT ( 'NONE',  ( -33.51206715926824842, -3.083556648223061192, 80.76191266582368655 ) ) ;
#16319 = DIRECTION ( 'NONE',  ( -0.000000000000000000, -1.000000000000000000, -0.000000000000000000 ) ) ;
#16320 = EDGE_LOOP ( 'NONE', ( #2801, #6894, #32037, #24661 ) ) ;
#16321 = DIRECTION ( 'NONE',  ( -0.9612616959383207815, -0.2756373558169927240, 3.618802040241776925E-17 ) ) ;
#16322 = VERTEX_POINT ( 'NONE', #27112 ) ;
#16323 = DIRECTION ( 'NONE',  ( -1.224646799147353207E-16, -1.349345573449484691E-32, 1.000000000000000000 ) ) ;
#16324 = AXIS2_PLACEMENT_3D ( 'NONE', #19733, #19574, #15150 ) ;
#16325 = CYLINDRICAL_SURFACE ( 'NONE', #17022, 1.199999999999999734 ) ;
#16326 = CARTESIAN_POINT ( 'NONE',  ( -4.652357239589691495, 10.40257568944043243, 97.56955547902282433 ) ) ;
#16327 = ORIENTED_EDGE ( 'NONE', *, *, #9005, .F. ) ;
#16328 = DIRECTION ( 'NONE',  ( 0.000000000000000000, 1.000000000000000000, 0.000000000000000000 ) ) ;
#16329 = DIRECTION ( 'NONE',  ( -0.4848096202463484938, -0.8746197071393896350, 2.220446049250314067E-16 ) ) ;
#16330 = DIRECTION ( 'NONE',  ( -0.8746197071393926326, 0.4848096202463430537, 8.676864087101709653E-18 ) ) ;
#16331 = CARTESIAN_POINT ( 'NONE',  ( 45.42003181263716272, 22.93807716476589675, 46.80027486889689214 ) ) ;
#16332 = ORIENTED_EDGE ( 'NONE', *, *, #23391, .F. ) ;
#16333 = DIRECTION ( 'NONE',  ( -0.000000000000000000, -1.000000000000000000, 0.000000000000000000 ) ) ;
#16334 = EDGE_CURVE ( 'NONE', #24129, #25156, #31054, .T. ) ;
#16335 = DIRECTION ( 'NONE',  ( 0.4848096202463637039, 0.8746197071393810862, 0.000000000000000000 ) ) ;
#16336 = CARTESIAN_POINT ( 'NONE',  ( 8.474859994195286461, 27.09184655352419568, 47.04930799450051637 ) ) ;
#16337 = DIRECTION ( 'NONE',  ( -1.000000000000000000, 0.000000000000000000, 0.000000000000000000 ) ) ;
#16338 = ADVANCED_FACE ( 'NONE', ( #25467 ), #2493, .T. ) ;
#16339 = ADVANCED_FACE ( 'NONE', ( #508 ), #26851, .F. ) ;
#16340 = EDGE_CURVE ( 'NONE', #31649, #8369, #21592, .T. ) ;
#16341 = ORIENTED_EDGE ( 'NONE', *, *, #28209, .T. ) ;
#16342 = CARTESIAN_POINT ( 'NONE',  ( -40.23397449525940317, 6.794506605641760011, 34.54930799450052348 ) ) ;
#16343 = CARTESIAN_POINT ( 'NONE',  ( -40.47677217214081224, 7.509199159541737778, 35.32896003352318814 ) ) ;
#16344 = ORIENTED_EDGE ( 'NONE', *, *, #22060, .F. ) ;
#16345 = DIRECTION ( 'NONE',  ( -1.000000000000000000, -1.101824276508909764E-16, 0.000000000000000000 ) ) ;
#16346 = ADVANCED_FACE ( 'NONE', ( #7432 ), #20617, .F. ) ;
#16347 = AXIS2_PLACEMENT_3D ( 'NONE', #6496, #16021, #26026 ) ;
#16348 = CARTESIAN_POINT ( 'NONE',  ( 21.09992658989239089, 30.34164230456639544, 47.04930799450051637 ) ) ;
#16349 = ORIENTED_EDGE ( 'NONE', *, *, #20637, .T. ) ;
#16350 = ORIENTED_EDGE ( 'NONE', *, *, #15975, .F. ) ;
#16351 = MECHANICAL_DESIGN_GEOMETRIC_PRESENTATION_REPRESENTATION (  '', ( #29488 ), #9098 ) ;
#16352 = ORIENTED_EDGE ( 'NONE', *, *, #26065, .T. ) ;
#16353 = TOROIDAL_SURFACE ( 'NONE', #27918, 78.39999999999999147, 0.1000000000000014211 ) ;
#16354 = ORIENTED_EDGE ( 'NONE', *, *, #18490, .T. ) ;
#16355 = CARTESIAN_POINT ( 'NONE',  ( 33.46699938050304013, 29.96183152705961206, 47.04930799450051637 ) ) ;
#16356 = ADVANCED_FACE ( 'NONE', ( #17587 ), #15296, .T. ) ;
#16357 = VERTEX_POINT ( 'NONE', #20049 ) ;
#16358 = CARTESIAN_POINT ( 'NONE',  ( 33.46699938050304013, 31.96183152705962272, 47.04930799450051637 ) ) ;
#16359 = AXIS2_PLACEMENT_3D ( 'NONE', #22677, #17745, #7747 ) ;
#16360 = CARTESIAN_POINT ( 'NONE',  ( -42.47434154250544225, 4.196643200812637531, 58.94930799450051495 ) ) ;
#16361 = DIRECTION ( 'NONE',  ( -1.000000000000000000, 0.000000000000000000, 0.000000000000000000 ) ) ;
#16362 = DIRECTION ( 'NONE',  ( -1.000000000000000000, 0.000000000000000000, 0.000000000000000000 ) ) ;
#16363 = AXIS2_PLACEMENT_3D ( 'NONE', #23479, #3122, #30876 ) ;
#16364 = CARTESIAN_POINT ( 'NONE',  ( 48.91284552371730143, 26.73619643316632377, 46.12344667017377020 ) ) ;
#16365 = ORIENTED_EDGE ( 'NONE', *, *, #20835, .F. ) ;
#16366 = EDGE_LOOP ( 'NONE', ( #25581, #23628, #23133, #28116 ) ) ;
#16367 = DIRECTION ( 'NONE',  ( -0.000000000000000000, -1.000000000000000000, 0.000000000000000000 ) ) ;
#16368 = ORIENTED_EDGE ( 'NONE', *, *, #22373, .F. ) ;
#16369 = CARTESIAN_POINT ( 'NONE',  ( 21.09785597605719332, 7.264443105416139801, 47.04930799450051637 ) ) ;
#16370 = FACE_OUTER_BOUND ( 'NONE', #18328, .T. ) ;
#16371 = DIRECTION ( 'NONE',  ( -0.8746197071393925215, 0.4848096202463429982, 8.676864087101708112E-18 ) ) ;
#16372 = DIRECTION ( 'NONE',  ( -1.000000000000000000, 0.000000000000000000, 0.000000000000000000 ) ) ;
#16373 = EDGE_CURVE ( 'NONE', #18749, #19345, #12721, .T. ) ;
#16374 = ADVANCED_FACE ( 'NONE', ( #5120 ), #6965, .T. ) ;
#16375 = CARTESIAN_POINT ( 'NONE',  ( 44.91142894931555674, 27.99787913140503903, 45.63089057098605394 ) ) ;
#16376 = EDGE_CURVE ( 'NONE', #13273, #12963, #6474, .T. ) ;
#16377 = AXIS2_PLACEMENT_3D ( 'NONE', #29483, #4366, #16984 ) ;
#16378 = LINE ( 'NONE', #18672, #22585 ) ;
#16379 = LINE ( 'NONE', #23929, #1742 ) ;
#16380 = EDGE_CURVE ( 'NONE', #19744, #23803, #14870, .T. ) ;
#16381 = VERTEX_POINT ( 'NONE', #10214 ) ;
#16382 = DIRECTION ( 'NONE',  ( -0.000000000000000000, -1.000000000000000000, 0.000000000000000000 ) ) ;
#16383 = CARTESIAN_POINT ( 'NONE',  ( 8.482002859293455543, 29.71664230456640254, 47.04930799450051637 ) ) ;
#16384 = DIRECTION ( 'NONE',  ( -1.000000000000000000, -1.101824276508909887E-16, 0.000000000000000000 ) ) ;
#16385 = DIRECTION ( 'NONE',  ( 0.3435019893673583735, 0.6546536707079779749, 0.6733757901270565061 ) ) ;
#16386 = CARTESIAN_POINT ( 'NONE',  ( -40.66586793973302605, 8.138261812237592707, 59.50788663826320146 ) ) ;
#16387 = VERTEX_POINT ( 'NONE', #195 ) ;
#16388 = DIRECTION ( 'NONE',  ( -1.000000000000000000, 0.000000000000000000, 0.000000000000000000 ) ) ;
#16389 = ORIENTED_EDGE ( 'NONE', *, *, #11216, .F. ) ;
#16390 = CARTESIAN_POINT ( 'NONE',  ( 21.09785597605719332, 25.76454579224776964, 47.04930799450051637 ) ) ;
#16391 = B_SPLINE_CURVE_WITH_KNOTS ( 'NONE', 3,
 ( #32421, #5173, #12564, #7143, #20254, #15341, #32264, #17307, #30281, #22066, #22552, #22389 ),
 .UNSPECIFIED., .F., .F.,
 ( 4, 2, 2, 2, 2, 4 ),
 ( 0.000000000000000000, 7.696047042336268032E-05, 0.0001154407056350440679, 0.0001539209408467254419, 0.0002308814112700844766, 0.0003078418816934435655 ),
 .UNSPECIFIED. ) ;
#16392 = ORIENTED_EDGE ( 'NONE', *, *, #25760, .F. ) ;
#16393 = AXIS2_PLACEMENT_3D ( 'NONE', #29515, #14412, #6536 ) ;
#16394 = VECTOR ( 'NONE', #8670, 1000.000000000000114 ) ;
#16395 = CIRCLE ( 'NONE', #28997, 1.199999999999999734 ) ;
#16396 = AXIS2_PLACEMENT_3D ( 'NONE', #26720, #16537, #14095 ) ;
#16397 = ORIENTED_EDGE ( 'NONE', *, *, #4149, .F. ) ;
#16398 = PLANE ( 'NONE',  #29077 ) ;
#16399 = ADVANCED_FACE ( 'NONE', ( #12689 ), #30079, .T. ) ;
#16400 = LINE ( 'NONE', #26259, #9218 ) ;
#16401 = DIRECTION ( 'NONE',  ( -0.000000000000000000, -1.000000000000000000, -0.000000000000000000 ) ) ;
#16402 = EDGE_CURVE ( 'NONE', #19851, #12159, #15454, .T. ) ;
#16403 = EDGE_LOOP ( 'NONE', ( #8811, #31444, #14704, #21671 ) ) ;
#16404 = CARTESIAN_POINT ( 'NONE',  ( -31.86441722936942611, -13.30632128221581212, 29.06553281253165011 ) ) ;
#16405 = DIRECTION ( 'NONE',  ( 0.000000000000000000, 1.000000000000000000, -0.000000000000000000 ) ) ;
#16406 = DIRECTION ( 'NONE',  ( -1.101824276508909887E-16, 1.000000000000000000, -0.000000000000000000 ) ) ;
#16407 = ORIENTED_EDGE ( 'NONE', *, *, #17408, .F. ) ;
#16408 = CARTESIAN_POINT ( 'NONE',  ( -43.43257085947613660, 1.024086014757300989, 53.64930799450051779 ) ) ;
#16409 = ORIENTED_EDGE ( 'NONE', *, *, #8767, .T. ) ;
#16410 = FACE_OUTER_BOUND ( 'NONE', #4865, .T. ) ;
#16411 = AXIS2_PLACEMENT_3D ( 'NONE', #11418, #11587, #26519 ) ;
#16412 = DIRECTION ( 'NONE',  ( 1.234978253042719660E-16, -1.000000000000000000, -1.109335647967047851E-31 ) ) ;
#16413 = AXIS2_PLACEMENT_3D ( 'NONE', #4629, #12187, #22182 ) ;
#16414 = ADVANCED_FACE ( 'NONE', ( #24819 ), #3789, .T. ) ;
#16415 = ORIENTED_EDGE ( 'NONE', *, *, #3935, .F. ) ;
#16416 = ORIENTED_EDGE ( 'NONE', *, *, #11647, .T. ) ;
#16417 =( REPRESENTATION_RELATIONSHIP ('NONE','NONE', #20382, #5723 ) REPRESENTATION_RELATIONSHIP_WITH_TRANSFORMATION ( #18037 )SHAPE_REPRESENTATION_RELATIONSHIP( ) );
#16418 = CARTESIAN_POINT ( 'NONE',  ( 57.98048228007293403, -13.30632128221581034, 5.000640598253887070 ) ) ;
#16419 = LINE ( 'NONE', #10871, #27174 ) ;
#16420 = B_SPLINE_CURVE_WITH_KNOTS ( 'NONE', 3,
 ( #17046, #11814, #7986, #12141, #14440, #20440, #24434, #32162, #17981, #24767, #9671, #17370 ),
 .UNSPECIFIED., .F., .F.,
 ( 4, 2, 2, 2, 2, 4 ),
 ( 0.000000000000000000, 7.988424390471597321E-05, 0.0001597684878094319464, 0.0001997106097617916745, 0.0002396527317141514026, 0.0003195369756188888837 ),
 .UNSPECIFIED. ) ;
#16421 = AXIS2_PLACEMENT_3D ( 'NONE', #9781, #14869, #17640 ) ;
#16422 = FACE_OUTER_BOUND ( 'NONE', #15304, .T. ) ;
#16423 = VERTEX_POINT ( 'NONE', #12352 ) ;
#16424 = AXIS2_PLACEMENT_3D ( 'NONE', #574, #8610, #25524 ) ;
#16425 = CARTESIAN_POINT ( 'NONE',  ( -5.602943079677954685, 9.702389020015065313, -4.315940132965163656 ) ) ;
#16426 = DIRECTION ( 'NONE',  ( 0.4848096202463424431, 0.8746197071393927436, -2.220446049250312588E-16 ) ) ;
#16427 = AXIS2_PLACEMENT_3D ( 'NONE', #25396, #12448, #5057 ) ;
#16428 = ORIENTED_EDGE ( 'NONE', *, *, #18157, .F. ) ;
#16429 = CARTESIAN_POINT ( 'NONE',  ( -40.50726676055796105, 7.559560307024983494, 60.29072935073781991 ) ) ;
#16430 = CARTESIAN_POINT ( 'NONE',  ( 48.46535932150934656, 29.68954579807170191, 49.73005965046827015 ) ) ;
#16431 = DIRECTION ( 'NONE',  ( 1.000000000000000000, 0.000000000000000000, -1.224646799147353207E-16 ) ) ;
#16432 = ADVANCED_FACE ( 'NONE', ( #2658 ), #27767, .T. ) ;
#16433 = ADVANCED_FACE ( 'NONE', ( #23800 ), #1315, .T. ) ;
#16434 = ORIENTED_EDGE ( 'NONE', *, *, #146, .F. ) ;
#16435 = CIRCLE ( 'NONE', #27981, 12.36707279061065101 ) ;
#16436 = DIRECTION ( 'NONE',  ( -1.101824276508909887E-16, 1.000000000000000000, -0.000000000000000000 ) ) ;
#16437 = CARTESIAN_POINT ( 'NONE',  ( 52.00918302503911406, -5.936918610400973684, -13.64030521451139677 ) ) ;
#16438 = EDGE_CURVE ( 'NONE', #7765, #294, #28964, .T. ) ;
#16439 = CARTESIAN_POINT ( 'NONE',  ( 49.19517401419062708, 28.40920399681022701, 48.40991706654173754 ) ) ;
#16440 = CARTESIAN_POINT ( 'NONE',  ( 46.02876340639226527, 25.51119643316632235, 44.95353858666495483 ) ) ;
#16441 = EDGE_CURVE ( 'NONE', #3511, #4649, #15935, .T. ) ;
#16442 = EDGE_LOOP ( 'NONE', ( #14047, #22519, #10597, #6133 ) ) ;
#16443 = EDGE_CURVE ( 'NONE', #27795, #2831, #30563, .T. ) ;
#16444 = AXIS2_PLACEMENT_3D ( 'NONE', #14541, #11752, #2058 ) ;
#16445 = DIRECTION ( 'NONE',  ( -1.000000000000000000, 0.000000000000000000, 0.000000000000000000 ) ) ;
#16446 = DIRECTION ( 'NONE',  ( 1.000000000000000000, 0.000000000000000000, 0.000000000000000000 ) ) ;
#16447 = CARTESIAN_POINT ( 'NONE',  ( 72.23777473803548332, 5.417291301124342873, 16.70329581060054380 ) ) ;
#16448 = DIRECTION ( 'NONE',  ( 0.9612616959383221138, 0.2756373558169876170, 0.000000000000000000 ) ) ;
#16449 = CARTESIAN_POINT ( 'NONE',  ( 21.09785597605720753, 14.86454579224779948, 47.04930799450052348 ) ) ;
#16450 = CYLINDRICAL_SURFACE ( 'NONE', #11552, 12.36707279061065279 ) ;
#16451 = CARTESIAN_POINT ( 'NONE',  ( 45.00053793792376666, 27.93655426599985248, 45.68869892245983522 ) ) ;
#16452 = ADVANCED_FACE ( 'NONE', ( #8078 ), #11137, .T. ) ;
#16453 = ORIENTED_EDGE ( 'NONE', *, *, #25569, .T. ) ;
#16454 = DIRECTION ( 'NONE',  ( -1.000000000000000000, 0.000000000000000000, 0.000000000000000000 ) ) ;
#16455 = CARTESIAN_POINT ( 'NONE',  ( 48.40186567930497574, 28.12957786121581805, 45.03923535223908203 ) ) ;
#16456 = DIRECTION ( 'NONE',  ( -1.101824276508909887E-16, 1.000000000000000000, -0.000000000000000000 ) ) ;
#16457 = FACE_OUTER_BOUND ( 'NONE', #24931, .T. ) ;
#16458 = DIRECTION ( 'NONE',  ( -1.000000000000000000, 0.000000000000000000, 0.000000000000000000 ) ) ;
#16459 = CIRCLE ( 'NONE', #24860, 0.1000000000000012962 ) ;
#16460 = ORIENTED_EDGE ( 'NONE', *, *, #13434, .T. ) ;
#16461 = CARTESIAN_POINT ( 'NONE',  ( 45.96182992765472619, 28.70087065737811827, 44.82232689504103007 ) ) ;
#16462 = CARTESIAN_POINT ( 'NONE',  ( -40.22836982583548604, 6.952244300597152815, 39.38126462244056114 ) ) ;
#16463 = CARTESIAN_POINT ( 'NONE',  ( 73.09176707068579049, 11.92558985988973497, 26.63511333407100778 ) ) ;
#16464 = ORIENTED_EDGE ( 'NONE', *, *, #23861, .F. ) ;
#16466 = CIRCLE ( 'NONE', #29051, 0.1249999999999983763 ) ;
#16465 = DIRECTION ( 'NONE',  ( 0.000000000000000000, 0.000000000000000000, -1.000000000000000000 ) ) ;
#16467 = DIRECTION ( 'NONE',  ( 1.000000000000000000, 0.000000000000000000, 0.000000000000000000 ) ) ;
#16468 = AXIS2_PLACEMENT_3D ( 'NONE', #32369, #12185, #4959 ) ;
#16469 = DIRECTION ( 'NONE',  ( 0.000000000000000000, -0.000000000000000000, -1.000000000000000000 ) ) ;
#16470 = DIRECTION ( 'NONE',  ( 0.2530443915476854322, -0.8824706660164470806, 0.3965022818682764627 ) ) ;
#16471 = AXIS2_PLACEMENT_3D ( 'NONE', #16078, #26086, #31191 ) ;
#16472 = ORIENTED_EDGE ( 'NONE', *, *, #2221, .F. ) ;
#16473 = CARTESIAN_POINT ( 'NONE',  ( 47.38797297166576072, 29.43365986774335497, 49.26645484953866116 ) ) ;
#16474 = ORIENTED_EDGE ( 'NONE', *, *, #26572, .F. ) ;
#16475 = ADVANCED_FACE ( 'NONE', ( #13165 ), #21099, .F. ) ;
#16476 = EDGE_CURVE ( 'NONE', #5096, #23253, #26103, .T. ) ;
#16477 = VERTEX_POINT ( 'NONE', #23162 ) ;
#16478 = EDGE_CURVE ( 'NONE', #28743, #12476, #3278, .T. ) ;
#16479 = ADVANCED_FACE ( 'NONE', ( #31046 ), #1162, .T. ) ;
#16480 = TOROIDAL_SURFACE ( 'NONE', #258, 83.95481021798164534, 94.94530576803560962 ) ;
#16481 = CARTESIAN_POINT ( 'NONE',  ( -30.89605511857125464, 11.92558985988973497, 67.46350265493038023 ) ) ;
#16482 = CARTESIAN_POINT ( 'NONE',  ( 21.09785597605719332, -16.63545420775219696, 126.2593585008393831 ) ) ;
#16483 = AXIS2_PLACEMENT_3D ( 'NONE', #5856, #909, #13723 ) ;
#16484 = LINE ( 'NONE', #4013, #24024 ) ;
#16485 = ADVANCED_FACE ( 'NONE', ( #8712 ), #28255, .T. ) ;
#16486 = AXIS2_PLACEMENT_3D ( 'NONE', #30722, #18220, #28253 ) ;
#16487 = AXIS2_PLACEMENT_3D ( 'NONE', #10459, #22916, #23251 ) ;
#16488 = ORIENTED_EDGE ( 'NONE', *, *, #8967, .F. ) ;
#16489 = CARTESIAN_POINT ( 'NONE',  ( 52.07878664889356912, -5.935345006353229813, -13.39445452378610568 ) ) ;
#16490 = VERTEX_POINT ( 'NONE', #8393 ) ;
#16491 = AXIS2_PLACEMENT_3D ( 'NONE', #11478, #29042, #6561 ) ;
#16492 = DIRECTION ( 'NONE',  ( 1.000000000000000000, 0.000000000000000000, 0.000000000000000000 ) ) ;
#16493 = ORIENTED_EDGE ( 'NONE', *, *, #27255, .F. ) ;
#16494 = CARTESIAN_POINT ( 'NONE',  ( 21.09992658989238734, 31.21664230456641675, 47.04930799450051637 ) ) ;
#16495 = CARTESIAN_POINT ( 'NONE',  ( -40.73091736380679606, 9.483895492497158131, 39.44930799450052206 ) ) ;
#16496 = FACE_BOUND ( 'NONE', #18793, .T. ) ;
#16497 = CARTESIAN_POINT ( 'NONE',  ( -40.57832940339291383, 7.446916344587776848, 53.85980283506936672 ) ) ;
#16498 = ORIENTED_EDGE ( 'NONE', *, *, #18518, .F. ) ;
#16499 = CARTESIAN_POINT ( 'NONE',  ( 47.47194490827082092, 22.91413368675619111, 45.28548791484912783 ) ) ;
#16500 = SPHERICAL_SURFACE ( 'NONE', #17315, 0.1000000000000000056 ) ;
#16501 = DIRECTION ( 'NONE',  ( -0.000000000000000000, 1.000000000000000000, -0.000000000000000000 ) ) ;
#16502 = CARTESIAN_POINT ( 'NONE',  ( 21.09785597605720042, -13.40182760052194588, 47.04930799450051637 ) ) ;
#16503 = ORIENTED_EDGE ( 'NONE', *, *, #11132, .F. ) ;
#16504 = CARTESIAN_POINT ( 'NONE',  ( -40.00476266209307852, 7.314288625132040700, 35.33031476312594066 ) ) ;
#16505 = DIRECTION ( 'NONE',  ( -1.101824276508909887E-16, 1.000000000000000000, -0.000000000000000000 ) ) ;
#16506 = ORIENTED_EDGE ( 'NONE', *, *, #15483, .T. ) ;
#16507 = CARTESIAN_POINT ( 'NONE',  ( 21.09785597605719332, -16.43042895458278352, -24.95571725866887292 ) ) ;
#16508 = DIRECTION ( 'NONE',  ( -1.000000000000000000, 0.000000000000000000, 0.000000000000000000 ) ) ;
#16509 = ORIENTED_EDGE ( 'NONE', *, *, #28578, .F. ) ;
#16510 = VECTOR ( 'NONE', #3253, 1000.000000000000000 ) ;
#16511 = ORIENTED_EDGE ( 'NONE', *, *, #8213, .T. ) ;
#16512 = CIRCLE ( 'NONE', #28049, 12.36707279061065101 ) ;
#16513 = CIRCLE ( 'NONE', #24388, 12.27641737965283042 ) ;
#16514 = CIRCLE ( 'NONE', #7628, 12.27641737965288193 ) ;
#16515 = VERTEX_POINT ( 'NONE', #15777 ) ;
#16516 = EDGE_CURVE ( 'NONE', #6910, #28202, #22127, .T. ) ;
#16517 = EDGE_CURVE ( 'NONE', #655, #2291, #8536, .T. ) ;
#16518 = DIRECTION ( 'NONE',  ( -1.101824276508909887E-16, 1.000000000000000000, -0.000000000000000000 ) ) ;
#16519 = ORIENTED_EDGE ( 'NONE', *, *, #18212, .F. ) ;
#16520 = CARTESIAN_POINT ( 'NONE',  ( 21.09992658989238734, 38.56284415653841791, 47.04930799450051637 ) ) ;
#16521 = DIRECTION ( 'NONE',  ( -1.101824276508909887E-16, 1.000000000000000000, -0.000000000000000000 ) ) ;
#16522 = DIRECTION ( 'NONE',  ( -1.000000000000000000, 0.000000000000000000, -1.224646799147353207E-16 ) ) ;
#16523 = CARTESIAN_POINT ( 'NONE',  ( 8.482002859293405805, 24.96664230456639899, 47.04930799450051637 ) ) ;
#16524 = CARTESIAN_POINT ( 'NONE',  ( 48.80717017713595141, 28.01952976649964810, 48.15820438821415195 ) ) ;
#16525 = VERTEX_POINT ( 'NONE', #10864 ) ;
#16526 = ORIENTED_EDGE ( 'NONE', *, *, #7464, .T. ) ;
#16528 = CARTESIAN_POINT ( 'NONE',  ( 21.09785597605719332, -15.93545420775219945, 118.3493079945004922 ) ) ;
#16527 = AXIS2_PLACEMENT_3D ( 'NONE', #27610, #7269, #5132 ) ;
#16529 = MECHANICAL_DESIGN_GEOMETRIC_PRESENTATION_REPRESENTATION (  '', ( #10284 ), #21775 ) ;
#16530 = ORIENTED_EDGE ( 'NONE', *, *, #24008, .F. ) ;
#16531 = CARTESIAN_POINT ( 'NONE',  ( -39.02270517653035853, 5.305726650763236130, 42.04930799450051637 ) ) ;
#16532 = CARTESIAN_POINT ( 'NONE',  ( 34.29963999142011488, 17.16467605102632632, 47.04930799450052348 ) ) ;
#16533 = CARTESIAN_POINT ( 'NONE',  ( -40.57495275781087685, 7.492308784444112746, 38.76861099430816893 ) ) ;
#16534 = AXIS2_PLACEMENT_3D ( 'NONE', #14490, #19392, #14161 ) ;
#16535 = DIRECTION ( 'NONE',  ( -1.000000000000000000, 0.000000000000000000, 0.000000000000000000 ) ) ;
#16536 = CARTESIAN_POINT ( 'NONE',  ( 44.09250526802607340, 25.25621246473838255, 46.89322480343881949 ) ) ;
#16537 = DIRECTION ( 'NONE',  ( -0.000000000000000000, -1.000000000000000000, 0.000000000000000000 ) ) ;
#16538 = ORIENTED_EDGE ( 'NONE', *, *, #30062, .F. ) ;
#16539 = FACE_OUTER_BOUND ( 'NONE', #19305, .T. ) ;
#16540 = DIRECTION ( 'NONE',  ( 1.431146867680865853E-17, 2.558717127065790464E-17, 1.000000000000000000 ) ) ;
#16541 = VECTOR ( 'NONE', #2285, 999.9999999999998863 ) ;
#16542 = DIRECTION ( 'NONE',  ( 0.000000000000000000, 0.000000000000000000, 1.000000000000000000 ) ) ;
#16543 = DIRECTION ( 'NONE',  ( 0.000000000000000000, -0.000000000000000000, -1.000000000000000000 ) ) ;
#16544 = ORIENTED_EDGE ( 'NONE', *, *, #15999, .T. ) ;
#16545 = CARTESIAN_POINT ( 'NONE',  ( -40.02540636251514172, 2.839176264122877047, 55.54930799450051637 ) ) ;
#16546 = VERTEX_POINT ( 'NONE', #18544 ) ;
#16547 = CARTESIAN_POINT ( 'NONE',  ( 21.09992658989239089, 28.59184655352419213, 47.04930799450051637 ) ) ;
#16548 = CARTESIAN_POINT ( 'NONE',  ( 48.23388214087538017, 25.16454579224780019, 49.27628903457465270 ) ) ;
#16549 = ORIENTED_EDGE ( 'NONE', *, *, #19785, .T. ) ;
#16550 = AXIS2_PLACEMENT_3D ( 'NONE', #18706, #23656, #28261 ) ;
#16551 = AXIS2_PLACEMENT_3D ( 'NONE', #31847, #14458, #14128 ) ;
#16552 = EDGE_CURVE ( 'NONE', #25764, #16020, #28200, .T. ) ;
#16553 = ADVANCED_FACE ( 'NONE', ( #17061 ), #8006, .T. ) ;
#16554 = EDGE_LOOP ( 'NONE', ( #3713, #28498, #6502, #9148 ) ) ;
#16555 = EDGE_CURVE ( 'NONE', #12544, #28026, #27076, .T. ) ;
#16556 = EDGE_CURVE ( 'NONE', #2570, #28996, #18480, .T. ) ;
#16557 = CARTESIAN_POINT ( 'NONE',  ( 21.09785597605720753, 13.86454579224779948, 47.04930799450052348 ) ) ;
#16558 = DIRECTION ( 'NONE',  ( -1.101824276508909887E-16, 1.000000000000000000, -0.000000000000000000 ) ) ;
#16559 = CYLINDRICAL_SURFACE ( 'NONE', #4742, 0.09999999999999945044 ) ;
#16560 = AXIS2_PLACEMENT_3D ( 'NONE', #5326, #5154, #15166 ) ;
#16561 = ORIENTED_EDGE ( 'NONE', *, *, #28676, .F. ) ;
#16562 = CARTESIAN_POINT ( 'NONE',  ( 33.72499318558949710, 27.09143805560860940, 47.04930799450051637 ) ) ;
#16563 = CARTESIAN_POINT ( 'NONE',  ( -35.12632216515690686, 11.92558985988973674, 40.04930799450050216 ) ) ;
#16564 = CARTESIAN_POINT ( 'NONE',  ( 75.42722807921533956, -1.035104995754000834, 13.52045531812380474 ) ) ;
#16565 = ORIENTED_EDGE ( 'NONE', *, *, #14719, .T. ) ;
#16566 = DIRECTION ( 'NONE',  ( -1.224646799147353207E-16, -1.349345573449484691E-32, 1.000000000000000000 ) ) ;
#16567 = ORIENTED_EDGE ( 'NONE', *, *, #6594, .T. ) ;
#16568 = DIRECTION ( 'NONE',  ( 0.000000000000000000, 0.000000000000000000, 1.000000000000000000 ) ) ;
#16569 = DIRECTION ( 'NONE',  ( 0.000000000000000000, 0.000000000000000000, -1.000000000000000000 ) ) ;
#16570 = CARTESIAN_POINT ( 'NONE',  ( 21.09785597605719332, 30.56454579224779522, 47.04930799450051637 ) ) ;
#16571 = DIRECTION ( 'NONE',  ( 0.1884548733085489869, 2.775557561562891351E-17, 0.9820818503191365290 ) ) ;
#16572 = ORIENTED_EDGE ( 'NONE', *, *, #10044, .F. ) ;
#16573 = ORIENTED_EDGE ( 'NONE', *, *, #3433, .T. ) ;
#16574 = CARTESIAN_POINT ( 'NONE',  ( 71.26428788917343127, -13.30632128221581212, 22.31577484639327125 ) ) ;
#16575 = AXIS2_PLACEMENT_3D ( 'NONE', #23297, #3096, #15425 ) ;
#16576 = PRODUCT_DEFINITION_FORMATION_WITH_SPECIFIED_SOURCE ( 'ANY', '', #3299, .NOT_KNOWN. ) ;
#16577 = DIRECTION ( 'NONE',  ( -0.4848096202463430537, -0.8746197071393926326, -9.920727850371701658E-18 ) ) ;
#16578 = CARTESIAN_POINT ( 'NONE',  ( -9.985300507345989729, -5.931148802125862929, 106.5968259136538023 ) ) ;
#16579 = ORIENTED_EDGE ( 'NONE', *, *, #10669, .F. ) ;
#16580 = CARTESIAN_POINT ( 'NONE',  ( -11.36318842908626081, -5.379633064793121200, -10.70487703641348354 ) ) ;
#16581 = CARTESIAN_POINT ( 'NONE',  ( 77.45956091363649421, -13.74047052604243113, 62.14575043855074910 ) ) ;
#16582 = EDGE_LOOP ( 'NONE', ( #20342, #32169, #15744, #15310, #13927, #3359, #8666 ) ) ;
#16583 = DIRECTION ( 'NONE',  ( -1.000000000000000000, 0.000000000000000000, 0.000000000000000000 ) ) ;
#16584 = CARTESIAN_POINT ( 'NONE',  ( 48.46535932150934656, 26.18954579807170902, 49.73005965046827015 ) ) ;
#16585 = EDGE_CURVE ( 'NONE', #3968, #22382, #15326, .T. ) ;
#16586 = ADVANCED_FACE ( 'NONE', ( #29553 ), #24616, .T. ) ;
#16587 = VECTOR ( 'NONE', #10178, 1000.000000000000000 ) ;
#16588 = CARTESIAN_POINT ( 'NONE',  ( -35.64882101543633297, 9.925589859889724309, 52.04930799450051637 ) ) ;
#16589 = ORIENTED_EDGE ( 'NONE', *, *, #31702, .F. ) ;
#16590 = DIRECTION ( 'NONE',  ( -1.000000000000000000, 0.000000000000000000, 0.000000000000000000 ) ) ;
#16591 = ADVANCED_FACE ( 'NONE', ( #19355 ), #6577, .T. ) ;
#16592 = CARTESIAN_POINT ( 'NONE',  ( 21.09785597605718976, -13.68121847681060643, 47.04930799450051637 ) ) ;
#16593 = CIRCLE ( 'NONE', #2469, 12.36707279061065101 ) ;
#16594 = CARTESIAN_POINT ( 'NONE',  ( -40.55202315603388286, 7.223587105649684759, 35.33283365102737861 ) ) ;
#16595 = CARTESIAN_POINT ( 'NONE',  ( 48.83862994770794330, 28.04118040159426428, 48.17861352429476796 ) ) ;
#16596 = ORIENTED_EDGE ( 'NONE', *, *, #8807, .T. ) ;
#16597 = DIRECTION ( 'NONE',  ( -0.8746197071393926326, 0.4848096202463430537, 8.676864087101709653E-18 ) ) ;
#16598 = LINE ( 'NONE', #24318, #31871 ) ;
#16599 = DIRECTION ( 'NONE',  ( 0.000000000000000000, -8.673617379884027583E-16, -1.000000000000000000 ) ) ;
#16600 = CARTESIAN_POINT ( 'NONE',  ( 45.96182992765472619, 26.47822092656774728, 44.82232689504103007 ) ) ;
#16601 = CARTESIAN_POINT ( 'NONE',  ( 45.33322567907855927, 22.86454579224779948, 47.99136533781562974 ) ) ;
#16602 = CARTESIAN_POINT ( 'NONE',  ( 13.47645946438857401, -13.74047052604243646, -10.79927602576051093 ) ) ;
#16603 = CARTESIAN_POINT ( 'NONE',  ( 8.580227611973585411, 32.55121380581068991, 47.04930799450051637 ) ) ;
#16604 = EDGE_CURVE ( 'NONE', #3840, #32154, #6934, .T. ) ;
#16605 = DIRECTION ( 'NONE',  ( -1.101824276508909887E-16, 1.000000000000000000, -0.000000000000000000 ) ) ;
#16606 =( NAMED_UNIT ( * ) SI_UNIT ( $, .STERADIAN. ) SOLID_ANGLE_UNIT ( ) );
#16607 = EDGE_LOOP ( 'NONE', ( #11185, #31266, #10552, #24076 ) ) ;
#16608 = CYLINDRICAL_SURFACE ( 'NONE', #15489, 12.62506659569710266 ) ;
#16609 = CARTESIAN_POINT ( 'NONE',  ( 48.94625023931840246, 28.77124452788248377, 46.10640627770150246 ) ) ;
#16610 = ADVANCED_FACE ( 'NONE', ( #21325 ), #4336, .T. ) ;
#16611 = DIRECTION ( 'NONE',  ( -0.000000000000000000, 1.000000000000000000, -0.000000000000000000 ) ) ;
#16612 = DIRECTION ( 'NONE',  ( 1.000000000000000000, 0.000000000000000000, 1.224646799147353207E-16 ) ) ;
#16613 = ORIENTED_EDGE ( 'NONE', *, *, #17891, .F. ) ;
#16614 = DIRECTION ( 'NONE',  ( -1.000000000000000000, 0.000000000000000000, 0.000000000000000000 ) ) ;
#16615 = CARTESIAN_POINT ( 'NONE',  ( 46.96997866373305186, 23.12036939723557083, 46.79862680810013131 ) ) ;
#16616 = PLANE ( 'NONE',  #9428 ) ;
#16617 = VERTEX_POINT ( 'NONE', #26918 ) ;
#16618 = CARTESIAN_POINT ( 'NONE',  ( 21.09785597605719332, 15.24673779880127178, 59.53344952167763182 ) ) ;
#16619 = CARTESIAN_POINT ( 'NONE',  ( 21.09992658989238734, 30.96664230456641675, 47.04930799450051637 ) ) ;
#16620 = ADVANCED_FACE ( 'NONE', ( #4435 ), #27915, .T. ) ;
#16621 = AXIS2_PLACEMENT_3D ( 'NONE', #14832, #12372, #22359 ) ;
#16622 = EDGE_CURVE ( 'NONE', #31962, #14214, #6421, .T. ) ;
#16623 = CARTESIAN_POINT ( 'NONE',  ( 8.474859994195286461, 24.84184655352419213, 47.04930799450051637 ) ) ;
#16624 = CARTESIAN_POINT ( 'NONE',  ( 21.09992658989239089, 25.34164230456639899, 47.04930799450051637 ) ) ;
#16625 = PRODUCT_DEFINITION_SHAPE ( 'NONE', 'NONE',  #32507 ) ;
#16626 = EDGE_LOOP ( 'NONE', ( #6354, #29197, #7164, #16015 ) ) ;
#16627 = CARTESIAN_POINT ( 'NONE',  ( 47.08544753267502614, 29.42444312243182836, 49.29451668004490728 ) ) ;
#16628 = CIRCLE ( 'NONE', #14024, 78.50000000000000000 ) ;
#16629 = ORIENTED_EDGE ( 'NONE', *, *, #29770, .F. ) ;
#16630 = ORIENTED_EDGE ( 'NONE', *, *, #31643, .F. ) ;
#16631 = ADVANCED_FACE ( 'NONE', ( #31689 ), #32008, .F. ) ;
#16632 = DIRECTION ( 'NONE',  ( 0.000000000000000000, 0.000000000000000000, -1.000000000000000000 ) ) ;
#16633 = DIRECTION ( 'NONE',  ( -1.000000000000000000, 0.000000000000000000, 0.000000000000000000 ) ) ;
#16634 = CARTESIAN_POINT ( 'NONE',  ( 21.09785597605720753, -5.098646251524523443, 47.04930799450052348 ) ) ;
#16635 = CARTESIAN_POINT ( 'NONE',  ( 81.79525877758869967, -5.936960083300406588, 77.94871473493923020 ) ) ;
#16636 = AXIS2_PLACEMENT_3D ( 'NONE', #27578, #17398, #10344 ) ;
#16637 = ORIENTED_EDGE ( 'NONE', *, *, #8709, .F. ) ;
#16638 = CARTESIAN_POINT ( 'NONE',  ( 21.09785597605720753, 14.86454579224779948, 47.04930799450052348 ) ) ;
#16639 = ORIENTED_EDGE ( 'NONE', *, *, #6521, .F. ) ;
#16640 = CARTESIAN_POINT ( 'NONE',  ( -42.21195563036361875, 4.051200314738730768, 39.04930799450052348 ) ) ;
#16641 = AXIS2_PLACEMENT_3D ( 'NONE', #4068, #1610, #21459 ) ;
#16642 = EDGE_CURVE ( 'NONE', #5063, #22685, #12637, .T. ) ;
#16643 = FACE_OUTER_BOUND ( 'NONE', #4054, .T. ) ;
#16644 = ORIENTED_EDGE ( 'NONE', *, *, #13278, .T. ) ;
#16645 = DIRECTION ( 'NONE',  ( -2.779292025043186357E-18, 1.288349127009862211E-17, -1.000000000000000000 ) ) ;
#16646 = DIRECTION ( 'NONE',  ( 0.2756373558169932236, -0.9612616959383206705, -2.918609477355926788E-15 ) ) ;
#16647 = DIRECTION ( 'NONE',  ( -0.000000000000000000, -1.000000000000000000, 0.000000000000000000 ) ) ;
#16648 = VERTEX_POINT ( 'NONE', #11492 ) ;
#16649 = DIRECTION ( 'NONE',  ( -0.000000000000000000, -1.000000000000000000, -0.000000000000000000 ) ) ;
#16650 = FACE_OUTER_BOUND ( 'NONE', #8908, .T. ) ;
#16651 = AXIS2_PLACEMENT_3D ( 'NONE', #19753, #7467, #28287 ) ;
#16652 = FACE_OUTER_BOUND ( 'NONE', #18048, .T. ) ;
#16653 = CARTESIAN_POINT ( 'NONE',  ( -42.26497471389478733, 14.66834543456874940, 60.54930799450051637 ) ) ;
#16654 = ORIENTED_EDGE ( 'NONE', *, *, #22616, .T. ) ;
#16655 = CARTESIAN_POINT ( 'NONE',  ( 21.09785597605719332, 25.76454579224776964, 47.04930799450051637 ) ) ;
#16656 = DIRECTION ( 'NONE',  ( -0.1949050434465267878, 0.6797146636928675933, 0.7071067811865471286 ) ) ;
#16657 = ORIENTED_EDGE ( 'NONE', *, *, #23459, .T. ) ;
#16658 = CARTESIAN_POINT ( 'NONE',  ( 21.09785597605719332, 34.11266481626051217, 34.06511779397349216 ) ) ;
#16659 = EDGE_CURVE ( 'NONE', #13866, #2064, #14817, .T. ) ;
#16660 = CARTESIAN_POINT ( 'NONE',  ( 33.72499318558949000, 38.56284415653841791, 47.04930799450051637 ) ) ;
#16661 = EDGE_CURVE ( 'NONE', #16423, #29220, #17944, .T. ) ;
#16662 = VERTEX_POINT ( 'NONE', #21659 ) ;
#16663 = VERTEX_POINT ( 'NONE', #26755 ) ;
#16664 = AXIS2_PLACEMENT_3D ( 'NONE', #20560, #25173, #539 ) ;
#16665 = UNCERTAINTY_MEASURE_WITH_UNIT (LENGTH_MEASURE( 1.000000000000000082E-05 ), #26106, 'distance_accuracy_value', 'NONE');
#16666 = VECTOR ( 'NONE', #22089, 1000.000000000000114 ) ;
#16667 = ORIENTED_EDGE ( 'NONE', *, *, #3851, .T. ) ;
#16668 = TOROIDAL_SURFACE ( 'NONE', #2533, 12.40141737965286772, 0.1250000000000003331 ) ;
#16669 = CIRCLE ( 'NONE', #29266, 1.899999999999999023 ) ;
#16670 = CIRCLE ( 'NONE', #19826, 0.1250000000000001110 ) ;
#16671 = CARTESIAN_POINT ( 'NONE',  ( -40.09211399732166115, 9.667069410243957606, 38.64930799450052490 ) ) ;
#16672 = VERTEX_POINT ( 'NONE', #9198 ) ;
#16673 = CARTESIAN_POINT ( 'NONE',  ( 8.474859994195286461, 25.84184655352419213, 47.04930799450051637 ) ) ;
#16674 = CYLINDRICAL_SURFACE ( 'NONE', #21435, 12.62506659569710266 ) ;
#16675 = DIRECTION ( 'NONE',  ( 0.000000000000000000, -1.000000000000000000, 0.000000000000000000 ) ) ;
#16676 = CARTESIAN_POINT ( 'NONE',  ( -40.50844712113364920, 7.574537053903299899, 53.86130065048124038 ) ) ;
#16677 = EDGE_CURVE ( 'NONE', #9196, #18541, #19190, .T. ) ;
#16678 = CARTESIAN_POINT ( 'NONE',  ( 48.37829923888483563, 28.89452976649964810, 45.07556196625585443 ) ) ;
#16679 = EDGE_LOOP ( 'NONE', ( #13437, #26922, #17775, #11804 ) ) ;
#16680 = DIRECTION ( 'NONE',  ( -0.000000000000000000, -1.000000000000000000, 0.000000000000000000 ) ) ;
#16681 = ORIENTED_EDGE ( 'NONE', *, *, #23594, .F. ) ;
#16682 = DIRECTION ( 'NONE',  ( -1.101824276508909887E-16, 1.000000000000000000, -0.000000000000000000 ) ) ;
#16683 = CIRCLE ( 'NONE', #23504, 12.62506659569710443 ) ;
#16684 = ORIENTED_EDGE ( 'NONE', *, *, #11523, .F. ) ;
#16685 = DIRECTION ( 'NONE',  ( 0.4544104193609915243, 0.000000000000000000, 0.8907924397839082076 ) ) ;
#16686 = DIRECTION ( 'NONE',  ( 0.000000000000000000, -0.000000000000000000, -1.000000000000000000 ) ) ;
#16687 = CIRCLE ( 'NONE', #2556, 46.03812797983318461 ) ;
#16688 = DIRECTION ( 'NONE',  ( -1.000000000000000000, 0.000000000000000000, 0.000000000000000000 ) ) ;
#16689 = CARTESIAN_POINT ( 'NONE',  ( 33.37634396954521065, 30.34164230456639544, 47.04930799450051637 ) ) ;
#16690 = CARTESIAN_POINT ( 'NONE',  ( -3.902144023942795581, 14.86454579224779948, 47.04930799450052348 ) ) ;
#16691 = AXIS2_PLACEMENT_3D ( 'NONE', #11343, #18399, #15789 ) ;
#16692 = CARTESIAN_POINT ( 'NONE',  ( 44.77625694075215534, 24.61454579807171328, 48.23360063142255427 ) ) ;
#16693 = CARTESIAN_POINT ( 'NONE',  ( 47.86511985000206693, 22.93807716476589320, 48.55339511290479493 ) ) ;
#16694 = LINE ( 'NONE', #4065, #23754 ) ;
#16695 = ORIENTED_EDGE ( 'NONE', *, *, #19049, .F. ) ;
#16696 = DIRECTION ( 'NONE',  ( -1.101824276508909887E-16, 1.000000000000000000, -0.000000000000000000 ) ) ;
#16697 = DIRECTION ( 'NONE',  ( -0.000000000000000000, -1.000000000000000000, 0.000000000000000000 ) ) ;
#16698 = CARTESIAN_POINT ( 'NONE',  ( -40.60251150970604073, 6.748447833883064462, 60.44930799450051495 ) ) ;
#16699 = EDGE_CURVE ( 'NONE', #14290, #17233, #30021, .T. ) ;
#16700 = CIRCLE ( 'NONE', #25106, 70.59901951359279337 ) ;
#16701 = DIRECTION ( 'NONE',  ( -1.101824276508909887E-16, 1.000000000000000000, -0.000000000000000000 ) ) ;
#16702 = CARTESIAN_POINT ( 'NONE',  ( -29.27337757263006424, 5.786705267067572933, 16.84970013494222840 ) ) ;
#16703 = ORIENTED_EDGE ( 'NONE', *, *, #2031, .F. ) ;
#16704 = DIRECTION ( 'NONE',  ( 0.000000000000000000, -1.000000000000000000, 0.000000000000000000 ) ) ;
#16705 = ORIENTED_EDGE ( 'NONE', *, *, #25967, .F. ) ;
#16706 = CARTESIAN_POINT ( 'NONE',  ( -42.34864001897648933, 13.69590355195401266, 54.59258074835306473 ) ) ;
#16707 = CARTESIAN_POINT ( 'NONE',  ( 21.09785597605719332, 25.56454579224779877, 47.04930799450051637 ) ) ;
#16708 = VERTEX_POINT ( 'NONE', #24780 ) ;
#16709 = AXIS2_PLACEMENT_3D ( 'NONE', #14116, #24604, #14603 ) ;
#16710 = VECTOR ( 'NONE', #10767, 1000.000000000000114 ) ;
#16711 = VERTEX_POINT ( 'NONE', #9848 ) ;
#16712 = CARTESIAN_POINT ( 'NONE',  ( -40.50146157965988891, 7.595301493077382560, 38.44930799450052916 ) ) ;
#16713 = CARTESIAN_POINT ( 'NONE',  ( 21.09785597605719332, 30.36454579224779238, 47.04930799450051637 ) ) ;
#16714 = DIRECTION ( 'NONE',  ( -1.000000000000000000, 0.000000000000000000, 0.000000000000000000 ) ) ;
#16715 = ORIENTED_EDGE ( 'NONE', *, *, #4202, .F. ) ;
#16716 = CYLINDRICAL_SURFACE ( 'NONE', #2010, 25.50000000000000355 ) ;
#16717 = TOROIDAL_SURFACE ( 'NONE', #14117, 48.63405236513555963, 2.000000000000000000 ) ;
#16718 = DIRECTION ( 'NONE',  ( 0.4848096202460961957, 0.8746197071395293010, 0.000000000000000000 ) ) ;
#16719 = CARTESIAN_POINT ( 'NONE',  ( 44.67624849883564053, 19.86454579224779948, 46.92354143986608506 ) ) ;
#16720 = ORIENTED_EDGE ( 'NONE', *, *, #14234, .T. ) ;
#16721 = FACE_OUTER_BOUND ( 'NONE', #18555, .T. ) ;
#16722 = ORIENTED_EDGE ( 'NONE', *, *, #13315, .T. ) ;
#16723 = DIRECTION ( 'NONE',  ( -0.9612616959383194493, -0.2756373558169974980, -8.795445018804946186E-19 ) ) ;
#16724 = CARTESIAN_POINT ( 'NONE',  ( 8.698509210239588896, 32.59164230456639899, 47.04930799450051637 ) ) ;
#16725 = CARTESIAN_POINT ( 'NONE',  ( 21.09992658989239089, 27.96664230456639899, 47.04930799450051637 ) ) ;
#16726 = DIRECTION ( 'NONE',  ( 0.000000000000000000, 0.000000000000000000, 1.000000000000000000 ) ) ;
#16727 = ORIENTED_EDGE ( 'NONE', *, *, #24638, .F. ) ;
#16728 = ORIENTED_EDGE ( 'NONE', *, *, #11928, .T. ) ;
#16729 = CARTESIAN_POINT ( 'NONE',  ( 52.59785597605720397, 14.86454579224779948, 47.04930799450051637 ) ) ;
#16730 = AXIS2_PLACEMENT_3D ( 'NONE', #26015, #15857, #8152 ) ;
#16731 = LINE ( 'NONE', #21984, #26653 ) ;
#16733 = EDGE_CURVE ( 'NONE', #24243, #30037, #10114, .T. ) ;
#16732 = CIRCLE ( 'NONE', #23023, 0.1250000000000001110 ) ;
#16734 = EDGE_CURVE ( 'NONE', #5667, #17822, #27868, .T. ) ;
#16735 = LINE ( 'NONE', #29225, #30872 ) ;
#16736 = ADVANCED_FACE ( 'NONE', ( #20013 ), #10337, .T. ) ;
#16737 = EDGE_CURVE ( 'NONE', #17055, #11782, #12482, .T. ) ;
#16738 = ORIENTED_EDGE ( 'NONE', *, *, #28985, .F. ) ;
#16739 = CARTESIAN_POINT ( 'NONE',  ( -12.00369637303955450, -4.668720686625170480, -9.884046729306300350 ) ) ;
#16740 = CARTESIAN_POINT ( 'NONE',  ( 76.34803497562474206, -13.74047052604243646, 65.80996039395137132 ) ) ;
#16741 = ADVANCED_FACE ( 'NONE', ( #30362 ), #14299, .T. ) ;
#16742 = EDGE_LOOP ( 'NONE', ( #14482, #10955, #31127 ) ) ;
#16743 = DIRECTION ( 'NONE',  ( 0.000000000000000000, 0.000000000000000000, -1.000000000000000000 ) ) ;
#16744 = EDGE_CURVE ( 'NONE', #28434, #7034, #142, .T. ) ;
#16745 = CARTESIAN_POINT ( 'NONE',  ( 49.28428300279882990, 25.54787913140504685, 48.46772541801551171 ) ) ;
#16746 = CIRCLE ( 'NONE', #16233, 0.09999999999999864553 ) ;
#16747 = AXIS2_PLACEMENT_3D ( 'NONE', #13386, #23382, #889 ) ;
#16748 = CARTESIAN_POINT ( 'NONE',  ( 21.09785597605719332, 14.86454579224779771, -1.584744370635042587 ) ) ;
#16749 = AXIS2_PLACEMENT_3D ( 'NONE', #21637, #14272, #9013 ) ;
#16750 = AXIS2_PLACEMENT_3D ( 'NONE', #11463, #1778, #29188 ) ;
#16751 = VERTEX_POINT ( 'NONE', #10180 ) ;
#16752 = FACE_OUTER_BOUND ( 'NONE', #11038, .T. ) ;
#16753 = EDGE_CURVE ( 'NONE', #16795, #20430, #26866, .T. ) ;
#16754 = DIRECTION ( 'NONE',  ( -0.8746197071393926326, 0.4848096202463430537, 8.676864087101709653E-18 ) ) ;
#16755 = CARTESIAN_POINT ( 'NONE',  ( -40.54770213959441350, 7.393765961829920741, 35.41885462099428139 ) ) ;
#16756 = CARTESIAN_POINT ( 'NONE',  ( 48.80717017713595141, 25.91952976649965734, 48.15820438821415195 ) ) ;
#16757 = AXIS2_PLACEMENT_3D ( 'NONE', #10743, #23365, #5485 ) ;
#16758 = CIRCLE ( 'NONE', #1557, 0.09999999999999753530 ) ;
#16759 = ORIENTED_EDGE ( 'NONE', *, *, #8537, .F. ) ;
#16760 = CARTESIAN_POINT ( 'NONE',  ( -41.94956971822180947, 3.905757428664828890, 45.74930799450051211 ) ) ;
#16761 = CARTESIAN_POINT ( 'NONE',  ( -43.37834615508418068, 1.121909970995876416, 34.64930799450052490 ) ) ;
#16762 = EDGE_CURVE ( 'NONE', #1546, #2789, #7880, .T. ) ;
#16763 = DIRECTION ( 'NONE',  ( 0.4848096202463425541, 0.8746197071393929656, -2.220446049250313081E-16 ) ) ;
#16764 = VECTOR ( 'NONE', #29674, 1000.000000000000000 ) ;
#16765 = AXIS2_PLACEMENT_3D ( 'NONE', #1143, #11480, #26577 ) ;
#16766 = DIRECTION ( 'NONE',  ( 0.000000000000000000, 0.000000000000000000, -1.000000000000000000 ) ) ;
#16767 = CARTESIAN_POINT ( 'NONE',  ( -40.75848109938849717, 9.580021662090986823, 35.54930799450051637 ) ) ;
#16768 = CARTESIAN_POINT ( 'NONE',  ( -35.26384896152210757, -13.74047052604243646, 31.95286555045027299 ) ) ;
#16769 = DIRECTION ( 'NONE',  ( 0.000000000000000000, 0.000000000000000000, -1.000000000000000000 ) ) ;
#16770 = CIRCLE ( 'NONE', #14687, 2.000000000000001776 ) ;
#16771 = CARTESIAN_POINT ( 'NONE',  ( 44.87087493598345134, 28.05322093266651962, 48.18533415931919706 ) ) ;
#16772 = AXIS2_PLACEMENT_3D ( 'NONE', #9223, #13994, #3805 ) ;
#16773 =( NAMED_UNIT ( * ) PLANE_ANGLE_UNIT ( ) SI_UNIT ( $, .RADIAN. ) );
#16774 = EDGE_LOOP ( 'NONE', ( #29357, #13248, #12285, #22370, #6088 ) ) ;
#16775 = TOROIDAL_SURFACE ( 'NONE', #3686, 19.31976987914897848, 0.2000000000000029809 ) ;
#16776 = CARTESIAN_POINT ( 'NONE',  ( 21.09992658989238734, 38.56284415653841791, 47.04930799450051637 ) ) ;
#16777 = CARTESIAN_POINT ( 'NONE',  ( -40.45528000798979917, 8.522633796558835684, 34.54930799450052348 ) ) ;
#16778 = DIRECTION ( 'NONE',  ( 0.2756373558170013283, -0.9612616959383183390, 0.000000000000000000 ) ) ;
#16779 = ADVANCED_FACE ( 'NONE', ( #2784 ), #5935, .T. ) ;
#16780 = CARTESIAN_POINT ( 'NONE',  ( 33.72499318558949000, 38.56284415653841791, 47.04930799450051637 ) ) ;
#16781 = ADVANCED_FACE ( 'NONE', ( #12317 ), #12809, .T. ) ;
#16782 = ORIENTED_EDGE ( 'NONE', *, *, #15601, .T. ) ;
#16783 = LINE ( 'NONE', #21705, #17655 ) ;
#16784 = LINE ( 'NONE', #18751, #30510 ) ;
#16785 = CARTESIAN_POINT ( 'NONE',  ( 33.46699938050304013, 38.56284415653841791, 47.04930799450051637 ) ) ;
#16786 = VERTEX_POINT ( 'NONE', #29879 ) ;
#16787 = ORIENTED_EDGE ( 'NONE', *, *, #20700, .F. ) ;
#16788 = CARTESIAN_POINT ( 'NONE',  ( -40.13135354151336998, 6.899777549362542395, 39.53627064559790938 ) ) ;
#16789 = ADVANCED_FACE ( 'NONE', ( #7395 ), #10845, .F. ) ;
#16790 = AXIS2_PLACEMENT_3D ( 'NONE', #12691, #197, #29424 ) ;
#16791 = CARTESIAN_POINT ( 'NONE',  ( 21.09785597605719332, 14.86454579224779771, 47.04930799450051637 ) ) ;
#16792 = CARTESIAN_POINT ( 'NONE',  ( 21.09785597605720753, 17.36474115922713324, 47.04930799450052348 ) ) ;
#16793 = VERTEX_POINT ( 'NONE', #12650 ) ;
#16794 = CARTESIAN_POINT ( 'NONE',  ( 73.45468653378273416, 11.83469976691315928, 25.26135771474555369 ) ) ;
#16795 = VERTEX_POINT ( 'NONE', #22638 ) ;
#16796 = CIRCLE ( 'NONE', #1085, 1.500000000000001332 ) ;
#16797 = VERTEX_POINT ( 'NONE', #158 ) ;
#16798 = CIRCLE ( 'NONE', #17318, 12.62506659569710266 ) ;
#16799 = AXIS2_PLACEMENT_3D ( 'NONE', #10133, #22588, #14730 ) ;
#16800 = LINE ( 'NONE', #26821, #17358 ) ;
#16801 = CIRCLE ( 'NONE', #14716, 0.09999999999999795164 ) ;
#16802 = EDGE_CURVE ( 'NONE', #29052, #31613, #25842, .T. ) ;
#16803 = DIRECTION ( 'NONE',  ( -1.101824276508909887E-16, 1.000000000000000000, -0.000000000000000000 ) ) ;
#16804 = CARTESIAN_POINT ( 'NONE',  ( 56.59785597605721108, 14.86454579224779948, 47.04930799450051637 ) ) ;
#16805 = CARTESIAN_POINT ( 'NONE',  ( 8.732853799281738105, 24.21183152705959785, 47.04930799450051637 ) ) ;
#16806 = EDGE_CURVE ( 'NONE', #14245, #27142, #24272, .T. ) ;
#16807 = AXIS2_PLACEMENT_3D ( 'NONE', #28102, #16859, #11622 ) ;
#16808 = ADVANCED_FACE ( 'NONE', ( #6209 ), #23291, .F. ) ;
#16809 = EDGE_LOOP ( 'NONE', ( #2438, #15524 ) ) ;
#16810 = CYLINDRICAL_SURFACE ( 'NONE', #28081, 13.50178401536290806 ) ;
#16811 = ORIENTED_EDGE ( 'NONE', *, *, #17817, .F. ) ;
#16812 = DIRECTION ( 'NONE',  ( -1.101824276508909887E-16, 1.000000000000000000, -0.000000000000000000 ) ) ;
#16813 = DIRECTION ( 'NONE',  ( 0.000000000000000000, 0.000000000000000000, -1.000000000000000000 ) ) ;
#16814 = FACE_OUTER_BOUND ( 'NONE', #15670, .T. ) ;
#16815 = VERTEX_POINT ( 'NONE', #20980 ) ;
#16816 = CARTESIAN_POINT ( 'NONE',  ( 21.09785597605720753, 14.86454579224779948, 47.04930799450052348 ) ) ;
#16817 = DIRECTION ( 'NONE',  ( -1.000000000000000000, 0.000000000000000000, 0.000000000000000000 ) ) ;
#16818 = DIRECTION ( 'NONE',  ( -0.4848096202463636484, -0.8746197071393810862, 0.000000000000000000 ) ) ;
#16819 = DIRECTION ( 'NONE',  ( -1.000000000000000000, 0.000000000000000000, 0.000000000000000000 ) ) ;
#16820 = CARTESIAN_POINT ( 'NONE',  ( 21.09785597605720042, -16.03545420775220265, -22.94971151909227203 ) ) ;
#16821 = DIRECTION ( 'NONE',  ( -1.101824276508909887E-16, 1.000000000000000000, -0.000000000000000000 ) ) ;
#16822 = VERTEX_POINT ( 'NONE', #25432 ) ;
#16823 = AXIS2_PLACEMENT_3D ( 'NONE', #2265, #10147, #12781 ) ;
#16824 = CARTESIAN_POINT ( 'NONE',  ( -40.23847960489091236, 6.935107575317839057, 34.54930799450050927 ) ) ;
#16825 = DIRECTION ( 'NONE',  ( 1.234978253042719660E-16, -1.000000000000000000, -1.109335647967047851E-31 ) ) ;
#16826 = ORIENTED_EDGE ( 'NONE', *, *, #7723, .T. ) ;
#16827 = AXIS2_PLACEMENT_3D ( 'NONE', #24527, #12067, #22061 ) ;
#16828 = ADVANCED_FACE ( 'NONE', ( #31008 ), #13786, .F. ) ;
#16829 = DIRECTION ( 'NONE',  ( -1.101824276508909887E-16, 1.000000000000000000, -0.000000000000000000 ) ) ;
#16830 = CIRCLE ( 'NONE', #25741, 32.50000000000000000 ) ;
#16831 = DIRECTION ( 'NONE',  ( 0.000000000000000000, -9.698999007525318993E-17, 1.000000000000000000 ) ) ;
#16832 = ORIENTED_EDGE ( 'NONE', *, *, #26982, .T. ) ;
#16833 =( BOUNDED_CURVE ( )  B_SPLINE_CURVE ( 3, ( #30213, #12666, #27424, #4939 ),
 .UNSPECIFIED., .F., .F. ) 
 B_SPLINE_CURVE_WITH_KNOTS ( ( 4, 4 ),
 ( 3.141592653589793116, 3.493814887450676032 ),
 .UNSPECIFIED. ) 
 CURVE ( )  GEOMETRIC_REPRESENTATION_ITEM ( )  RATIONAL_B_SPLINE_CURVE ( ( 1.000000000000000000, 0.9896883177220923145, 0.9896883177220923145, 1.000000000000000000 ) ) 
 REPRESENTATION_ITEM ( '' )  );
#16834 = VERTEX_POINT ( 'NONE', #5573 ) ;
#16835 = ORIENTED_EDGE ( 'NONE', *, *, #32323, .F. ) ;
#16836 = ADVANCED_FACE ( 'NONE', ( #30691 ), #2792, .T. ) ;
#16837 = EDGE_CURVE ( 'NONE', #18936, #15519, #29501, .T. ) ;
#16838 = AXIS2_PLACEMENT_3D ( 'NONE', #10902, #10750, #1044 ) ;
#16839 = AXIS2_PLACEMENT_3D ( 'NONE', #24051, #9453, #6338 ) ;
#16840 = PRESENTATION_LAYER_ASSIGNMENT (  '', '', ( #8475 ) ) ;
#16841 = DIRECTION ( 'NONE',  ( 0.2756373558169931126, -0.9612616959383206705, 1.479773560108267642E-16 ) ) ;
#16842 = EDGE_CURVE ( 'NONE', #1328, #15339, #8202, .T. ) ;
#16843 = EDGE_CURVE ( 'NONE', #30925, #10687, #7503, .T. ) ;
#16844 = VERTEX_POINT ( 'NONE', #30530 ) ;
#16845 = ORIENTED_EDGE ( 'NONE', *, *, #20445, .F. ) ;
#16846 = DIRECTION ( 'NONE',  ( 0.000000000000000000, 1.000000000000000000, 0.000000000000000000 ) ) ;
#16847 = EDGE_CURVE ( 'NONE', #21737, #14877, #25753, .T. ) ;
#16848 = CARTESIAN_POINT ( 'NONE',  ( 21.09785597605720042, 13.74476430820393347, -8.950692005499485404 ) ) ;
#16849 = PLANE ( 'NONE',  #2856 ) ;
#16850 = CARTESIAN_POINT ( 'NONE',  ( -40.51045226066063520, 7.589116544599140646, 53.87859731638185679 ) ) ;
#16851 = CARTESIAN_POINT ( 'NONE',  ( 45.38854177497844944, 29.06952976649964882, 45.94041160078741370 ) ) ;
#16852 = ORIENTED_EDGE ( 'NONE', *, *, #1399, .T. ) ;
#16853 = CARTESIAN_POINT ( 'NONE',  ( 21.09785597605718266, -13.68121847681060643, 105.0821957556774890 ) ) ;
#16854 = ORIENTED_EDGE ( 'NONE', *, *, #32101, .F. ) ;
#16855 = CARTESIAN_POINT ( 'NONE',  ( -12.29624631804354706, -0.5585041340025408418, -6.109942736600796565 ) ) ;
#16856 = AXIS2_PLACEMENT_3D ( 'NONE', #13415, #18152, #5693 ) ;
#16857 = ORIENTED_EDGE ( 'NONE', *, *, #26072, .F. ) ;
#16858 = FACE_OUTER_BOUND ( 'NONE', #639, .T. ) ;
#16859 = DIRECTION ( 'NONE',  ( -0.000000000000000000, -0.000000000000000000, -1.000000000000000000 ) ) ;
#16860 = CARTESIAN_POINT ( 'NONE',  ( 21.09992658989238734, 38.56284415653841791, 47.04930799450051637 ) ) ;
#16861 = CARTESIAN_POINT ( 'NONE',  ( 21.09992658989238734, 38.56284415653841791, 47.04930799450051637 ) ) ;
#16862 = CARTESIAN_POINT ( 'NONE',  ( 21.09992658989239089, 25.22145308207319303, 47.04930799450051637 ) ) ;
#16863 = CARTESIAN_POINT ( 'NONE',  ( 46.96268396749378127, 27.53121246473837402, 49.65201805493727960 ) ) ;
#16864 = DIRECTION ( 'NONE',  ( 0.000000000000000000, 0.000000000000000000, -1.000000000000000000 ) ) ;
#16865 = DIRECTION ( 'NONE',  ( 1.188208965918164993E-16, 1.880121038077812639E-16, 1.000000000000000000 ) ) ;
#16866 = EDGE_LOOP ( 'NONE', ( #28712, #18996, #26244, #9275 ) ) ;
#16867 = LINE ( 'NONE', #16218, #22894 ) ;
#16868 = CARTESIAN_POINT ( 'NONE',  ( -42.03703168893574116, 3.954238390689463145, 47.04930799450051637 ) ) ;
#16869 = CARTESIAN_POINT ( 'NONE',  ( -40.52510752649232728, 7.677764709599122384, 34.54930799450052348 ) ) ;
#16870 = AXIS2_PLACEMENT_3D ( 'NONE', #25275, #479, #30693 ) ;
#16871 = DIRECTION ( 'NONE',  ( 0.8746197071393926326, -0.4848096202463430537, -8.676864087101709653E-18 ) ) ;
#16872 = ORIENTED_EDGE ( 'NONE', *, *, #31352, .T. ) ;
#16873 = CARTESIAN_POINT ( 'NONE',  ( 21.09785597605719332, -19.93545420775220123, 132.0493079945005377 ) ) ;
#16874 = AXIS2_PLACEMENT_3D ( 'NONE', #13381, #23377, #15508 ) ;
#16875 = ORIENTED_EDGE ( 'NONE', *, *, #15495, .F. ) ;
#16876 = FACE_OUTER_BOUND ( 'NONE', #5812, .T. ) ;
#16877 = DIRECTION ( 'NONE',  ( 7.588956326749211550E-18, -4.206627182996912454E-18, 1.000000000000000000 ) ) ;
#16878 = ORIENTED_EDGE ( 'NONE', *, *, #28439, .F. ) ;
#16879 = EDGE_CURVE ( 'NONE', #4161, #29641, #20194, .T. ) ;
#16880 = CIRCLE ( 'NONE', #15844, 0.1250000000000001110 ) ;
#16881 = EDGE_CURVE ( 'NONE', #1375, #17361, #8025, .T. ) ;
#16882 = AXIS2_PLACEMENT_3D ( 'NONE', #349, #29918, #24978 ) ;
#16883 = ORIENTED_EDGE ( 'NONE', *, *, #11399, .T. ) ;
#16884 = CYLINDRICAL_SURFACE ( 'NONE', #10242, 31.50000000000000000 ) ;
#16885 = CARTESIAN_POINT ( 'NONE',  ( 21.09992658989239089, 29.84164230456639899, 47.04930799450051637 ) ) ;
#16886 = CARTESIAN_POINT ( 'NONE',  ( 8.474859994195286461, 27.59184655352419568, 47.04930799450051637 ) ) ;
#16887 = EDGE_CURVE ( 'NONE', #28351, #13209, #23224, .T. ) ;
#16888 = AXIS2_PLACEMENT_3D ( 'NONE', #12310, #32335, #7707 ) ;
#16889 = ORIENTED_EDGE ( 'NONE', *, *, #22403, .F. ) ;
#16890 = EDGE_CURVE ( 'NONE', #9599, #6626, #5734, .T. ) ;
#16891 = DIRECTION ( 'NONE',  ( 0.9612616959383205595, 0.2756373558169930016, -1.660411357259282199E-16 ) ) ;
#16892 = AXIS2_PLACEMENT_3D ( 'NONE', #7691, #1096, #16031 ) ;
#16893 = CYLINDRICAL_SURFACE ( 'NONE', #3930, 12.62506659569710266 ) ;
#16894 = CARTESIAN_POINT ( 'NONE',  ( 8.474859994195282908, 38.56284415653841791, 47.04930799450051637 ) ) ;
#16895 = ORIENTED_EDGE ( 'NONE', *, *, #19025, .F. ) ;
#16896 = ORIENTED_EDGE ( 'NONE', *, *, #20154, .F. ) ;
#16897 = SURFACE_STYLE_FILL_AREA ( #21818 ) ;
#16898 = ORIENTED_EDGE ( 'NONE', *, *, #21668, .T. ) ;
#16899 = CARTESIAN_POINT ( 'NONE',  ( -40.51565501380215295, 9.065589196111961456, 57.04930799450051637 ) ) ;
#16900 = DIRECTION ( 'NONE',  ( 0.000000000000000000, 0.000000000000000000, -1.000000000000000000 ) ) ;
#16901 = DIRECTION ( 'NONE',  ( 1.234978253042719660E-16, -1.000000000000000000, -1.109335647967047851E-31 ) ) ;
#16902 = DIRECTION ( 'NONE',  ( 0.000000000000000000, 0.000000000000000000, 1.000000000000000000 ) ) ;
#16903 = ORIENTED_EDGE ( 'NONE', *, *, #22531, .F. ) ;
#16904 = ORIENTED_EDGE ( 'NONE', *, *, #19219, .T. ) ;
#16905 = DIRECTION ( 'NONE',  ( -1.101824276508909887E-16, 1.000000000000000000, -0.000000000000000000 ) ) ;
#16906 = CARTESIAN_POINT ( 'NONE',  ( 54.59785597605721108, -5.098646251524523443, 47.04930799450051637 ) ) ;
#16907 = CARTESIAN_POINT ( 'NONE',  ( -42.37913764077812573, 15.23192269303852875, 35.64930799450052490 ) ) ;
#16908 = EDGE_LOOP ( 'NONE', ( #21205, #24641, #940, #25182 ) ) ;
#16909 = CARTESIAN_POINT ( 'NONE',  ( -11.10673793619094241, -5.573920848077346335, -10.97183245130580254 ) ) ;
#16910 = CARTESIAN_POINT ( 'NONE',  ( -40.60333149162104860, 7.557375771971046596, 54.01510846932454513 ) ) ;
#16911 = CIRCLE ( 'NONE', #4862, 0.1000000000000018235 ) ;
#16912 = VERTEX_POINT ( 'NONE', #18353 ) ;
#16913 = CYLINDRICAL_SURFACE ( 'NONE', #14196, 2.500000000000002220 ) ;
#16914 = CARTESIAN_POINT ( 'NONE',  ( -40.65487266620045403, 9.475231293617264683, 39.43717596014455040 ) ) ;
#16915 = CYLINDRICAL_SURFACE ( 'NONE', #30083, 12.62506659569710266 ) ;
#16916 = CIRCLE ( 'NONE', #6432, 0.09999999999999795164 ) ;
#16917 = ORIENTED_EDGE ( 'NONE', *, *, #9574, .F. ) ;
#16918 = CARTESIAN_POINT ( 'NONE',  ( 46.95686452149019630, 22.86454579224779948, 49.04468102550210773 ) ) ;
#16919 = DIRECTION ( 'NONE',  ( 0.000000000000000000, 1.000000000000000000, -0.000000000000000000 ) ) ;
#16920 = DIRECTION ( 'NONE',  ( 0.000000000000000000, 0.000000000000000000, 1.000000000000000000 ) ) ;
#16921 = CARTESIAN_POINT ( 'NONE',  ( 48.40186567930498285, 28.21618040159426499, 45.03923535223908203 ) ) ;
#16922 = ADVANCED_FACE ( 'NONE', ( #5901 ), #5397, .T. ) ;
#16923 = ORIENTED_EDGE ( 'NONE', *, *, #23890, .T. ) ;
#16924 = CIRCLE ( 'NONE', #30052, 0.1249999999999966416 ) ;
#16925 = ADVANCED_FACE ( 'NONE', ( #3580 ), #9060, .T. ) ;
#16926 = CARTESIAN_POINT ( 'NONE',  ( 47.99562520726186676, 20.53597436367637386, 45.66543703126890819 ) ) ;
#16928 = LINE ( 'NONE', #9388, #12513 ) ;
#16927 = CONICAL_SURFACE ( 'NONE', #5427, 54.74424859897010975, 1.291543646475813212 ) ;
#16929 = CARTESIAN_POINT ( 'NONE',  ( 49.97900733303978882, 7.511668073839842030, -3.600006413221115587 ) ) ;
#16930 = CYLINDRICAL_SURFACE ( 'NONE', #23363, 2.000000000000001776 ) ;
#16931 = DIRECTION ( 'NONE',  ( 0.000000000000000000, 1.000000000000000000, 0.000000000000000000 ) ) ;
#16932 = DIRECTION ( 'NONE',  ( 2.779292025043186357E-18, -1.288349127009862211E-17, 1.000000000000000000 ) ) ;
#16933 = CIRCLE ( 'NONE', #25847, 13.30165371409683850 ) ;
#16934 = CIRCLE ( 'NONE', #15896, 12.36707279061065101 ) ;
#16935 = LINE ( 'NONE', #4965, #18414 ) ;
#16936 = ORIENTED_EDGE ( 'NONE', *, *, #22431, .T. ) ;
#16937 = CARTESIAN_POINT ( 'NONE',  ( 45.46177120706448704, 22.89977464660286444, 46.15605224449101485 ) ) ;
#16938 = CARTESIAN_POINT ( 'NONE',  ( 44.57318751115185052, 25.19787913140503477, 45.41146063192157101 ) ) ;
#16939 = CARTESIAN_POINT ( 'NONE',  ( -30.66771913184581777, 11.92469184102449908, 26.05320424947958458 ) ) ;
#16940 = DIRECTION ( 'NONE',  ( 0.2756373558169942228, -0.9612616959383203374, 0.000000000000000000 ) ) ;
#16941 = ORIENTED_EDGE ( 'NONE', *, *, #1031, .T. ) ;
#16942 = CARTESIAN_POINT ( 'NONE',  ( 47.42898969722134694, 14.98691807112498964, 46.53888023006170727 ) ) ;
#16943 = CARTESIAN_POINT ( 'NONE',  ( 45.41653742442153430, 19.86454579224779948, 43.75337596730032175 ) ) ;
#16944 = DIRECTION ( 'NONE',  ( -1.101824276508909887E-16, 1.000000000000000000, -0.000000000000000000 ) ) ;
#16945 = ORIENTED_EDGE ( 'NONE', *, *, #6228, .T. ) ;
#16946 = EDGE_LOOP ( 'NONE', ( #27781, #19227, #2398, #21502 ) ) ;
#16947 = DIRECTION ( 'NONE',  ( 0.8746197071393926326, -0.4848096202463430537, -8.676864087101709653E-18 ) ) ;
#16948 = CARTESIAN_POINT ( 'NONE',  ( -40.02540636251513462, 2.839176264122873050, 38.24930799450051921 ) ) ;
#16949 = CARTESIAN_POINT ( 'NONE',  ( 52.07598125554711999, -5.935454207752202116, 106.7232700815558957 ) ) ;
#16950 = AXIS2_PLACEMENT_3D ( 'NONE', #5871, #30974, #20463 ) ;
#16951 = ORIENTED_EDGE ( 'NONE', *, *, #23234, .F. ) ;
#16952 = CARTESIAN_POINT ( 'NONE',  ( 71.56946472858759023, 10.07047442526145531, 20.80384636583699987 ) ) ;
#16953 = VERTEX_POINT ( 'NONE', #28383 ) ;
#16954 = ORIENTED_EDGE ( 'NONE', *, *, #5229, .T. ) ;
#16955 = TOROIDAL_SURFACE ( 'NONE', #15917, 12.40141737965286062, 0.1249999999999998196 ) ;
#16956 = AXIS2_PLACEMENT_3D ( 'NONE', #5315, #14842, #15319 ) ;
#16957 = DIRECTION ( 'NONE',  ( 0.2756373558169974980, -0.9612616959383194493, -1.315048337272770743E-17 ) ) ;
#16958 = ORIENTED_EDGE ( 'NONE', *, *, #3928, .F. ) ;
#16959 = EDGE_CURVE ( 'NONE', #28042, #23355, #22705, .T. ) ;
#16960 = EDGE_CURVE ( 'NONE', #22668, #27774, #16924, .T. ) ;
#16961 = EDGE_CURVE ( 'NONE', #9654, #3824, #19487, .T. ) ;
#16962 = DIRECTION ( 'NONE',  ( -1.000000000000000000, 0.000000000000000000, 0.000000000000000000 ) ) ;
#16963 = DIRECTION ( 'NONE',  ( -1.101824276508909887E-16, 1.000000000000000000, -0.000000000000000000 ) ) ;
#16964 = FACE_OUTER_BOUND ( 'NONE', #20553, .T. ) ;
#16965 = EDGE_CURVE ( 'NONE', #5962, #16253, #3411, .T. ) ;
#16966 = EDGE_LOOP ( 'NONE', ( #21336, #26687, #21645, #25797 ) ) ;
#16967 = FACE_OUTER_BOUND ( 'NONE', #26691, .T. ) ;
#16968 = ORIENTED_EDGE ( 'NONE', *, *, #12421, .T. ) ;
#16969 = DIRECTION ( 'NONE',  ( 1.000000000000000000, 0.000000000000000000, 0.000000000000000000 ) ) ;
#16970 = CIRCLE ( 'NONE', #16237, 1.042135311067126979 ) ;
#16971 = FACE_OUTER_BOUND ( 'NONE', #32284, .T. ) ;
#16972 = ORIENTED_EDGE ( 'NONE', *, *, #22293, .T. ) ;
#16973 = FACE_OUTER_BOUND ( 'NONE', #10798, .T. ) ;
#16974 = LINE ( 'NONE', #29794, #27472 ) ;
#16975 = CARTESIAN_POINT ( 'NONE',  ( 21.09992658989239089, 25.96664230456639899, 47.04930799450051637 ) ) ;
#16976 = DIRECTION ( 'NONE',  ( 0.000000000000000000, 1.000000000000000000, -0.000000000000000000 ) ) ;
#16977 = CARTESIAN_POINT ( 'NONE',  ( 21.09992658989238734, 31.84164230456639544, 47.04930799450051637 ) ) ;
#16978 = DIRECTION ( 'NONE',  ( -1.101824276508909887E-16, 1.000000000000000000, -0.000000000000000000 ) ) ;
#16979 = ORIENTED_EDGE ( 'NONE', *, *, #30990, .F. ) ;
#16980 = FACE_OUTER_BOUND ( 'NONE', #10952, .T. ) ;
#16981 = DIRECTION ( 'NONE',  ( 0.000000000000000000, 0.7071067811865260344, 0.7071067811865690000 ) ) ;
#16982 = VERTEX_POINT ( 'NONE', #13771 ) ;
#16983 = CARTESIAN_POINT ( 'NONE',  ( -45.06166779280743384, -5.721341737285086992, 53.14897153969102561 ) ) ;
#16984 = DIRECTION ( 'NONE',  ( 1.000000000000000000, 0.000000000000000000, 0.000000000000000000 ) ) ;
#16985 = VERTEX_POINT ( 'NONE', #1604 ) ;
#16986 = ORIENTED_EDGE ( 'NONE', *, *, #12545, .T. ) ;
#16987 = EDGE_CURVE ( 'NONE', #10568, #17364, #31105, .T. ) ;
#16988 = UNCERTAINTY_MEASURE_WITH_UNIT (LENGTH_MEASURE( 1.000000000000000082E-05 ), #22510, 'distance_accuracy_value', 'NONE');
#16989 = ADVANCED_FACE ( 'NONE', ( #11945 ), #9155, .T. ) ;
#16990 = ORIENTED_EDGE ( 'NONE', *, *, #10772, .T. ) ;
#16991 = AXIS2_PLACEMENT_3D ( 'NONE', #26783, #4131, #28760 ) ;
#16992 = VECTOR ( 'NONE', #6727, 1000.000000000000000 ) ;
#16993 = CIRCLE ( 'NONE', #24862, 12.62506659569710266 ) ;
#16994 = CONICAL_SURFACE ( 'NONE', #26970, 85.00000000000001421, 0.7853981633974621568 ) ;
#16995 = AXIS2_PLACEMENT_3D ( 'NONE', #20455, #13257, #6016 ) ;
#16996 = AXIS2_PLACEMENT_3D ( 'NONE', #27099, #31868, #11690 ) ;
#16997 = CYLINDRICAL_SURFACE ( 'NONE', #25048, 12.62506659569710266 ) ;
#16998 = ADVANCED_FACE ( 'NONE', ( #24250, #26554 ), #31488, .T. ) ;
#16999 = ORIENTED_EDGE ( 'NONE', *, *, #28355, .F. ) ;
#17000 = ORIENTED_EDGE ( 'NONE', *, *, #21788, .T. ) ;
#17001 = CARTESIAN_POINT ( 'NONE',  ( 33.46699938050303302, 38.56284415653841791, 47.04930799450051637 ) ) ;
#17002 = DIRECTION ( 'NONE',  ( -0.4848096202463429982, -0.8746197071393925215, -9.920727850371698576E-18 ) ) ;
#17003 = DIRECTION ( 'NONE',  ( 0.000000000000000000, 1.000000000000000000, 0.000000000000000000 ) ) ;
#17004 = DIRECTION ( 'NONE',  ( 0.000000000000000000, 0.000000000000000000, 1.000000000000000000 ) ) ;
#17005 = CARTESIAN_POINT ( 'NONE',  ( 48.80717017713595141, 29.41952976649965024, 48.15820438821415195 ) ) ;
#17006 = EDGE_LOOP ( 'NONE', ( #15232, #28212, #28409, #4693 ) ) ;
#17007 = LINE ( 'NONE', #27033, #9168 ) ;
#17008 = ORIENTED_EDGE ( 'NONE', *, *, #27990, .T. ) ;
#17009 = CARTESIAN_POINT ( 'NONE',  ( -10.08218489754580638, -5.944439029104265693, -10.85306528164251993 ) ) ;
#17010 = ORIENTED_EDGE ( 'NONE', *, *, #27901, .F. ) ;
#17011 = DIRECTION ( 'NONE',  ( 0.2756373558169932236, -0.9612616959383204485, 1.479773560108267395E-16 ) ) ;
#17012 = DIRECTION ( 'NONE',  ( 0.4848096202463673121, 0.8746197071393789768, 0.000000000000000000 ) ) ;
#17013 = CARTESIAN_POINT ( 'NONE',  ( 52.11354816884804819, -5.936701049740607417, 107.6763359263316602 ) ) ;
#17014 = DIRECTION ( 'NONE',  ( 1.000000000000000000, 0.000000000000000000, 0.000000000000000000 ) ) ;
#17015 = CARTESIAN_POINT ( 'NONE',  ( 21.09785597605719332, 6.547041198165487685, 47.04930799450051637 ) ) ;
#17016 = CARTESIAN_POINT ( 'NONE',  ( 44.91142894931555674, 26.59787913140504401, 45.63089057098605394 ) ) ;
#17017 = CIRCLE ( 'NONE', #1271, 19.25826962553310295 ) ;
#17018 = SHAPE_REPRESENTATION ( 'Coil Support', ( #8172 ), #26498 ) ;
#17019 = CARTESIAN_POINT ( 'NONE',  ( -58.11219453028166981, 25.56454579224780232, 47.04930799450023926 ) ) ;
#17020 = CARTESIAN_POINT ( 'NONE',  ( -40.21210701746132798, 7.644196001419686581, 53.84930799450049932 ) ) ;
#17021 = ADVANCED_FACE ( 'NONE', ( #29341, #11787, #28864, #8829, #14090, #24086 ), #13932, .F. ) ;
#17022 = AXIS2_PLACEMENT_3D ( 'NONE', #26343, #13882, #23880 ) ;
#17023 = ORIENTED_EDGE ( 'NONE', *, *, #4701, .F. ) ;
#17024 = CARTESIAN_POINT ( 'NONE',  ( 47.15451600283464728, 29.59167404947196900, 44.97719271889386050 ) ) ;
#17025 = DIRECTION ( 'NONE',  ( -1.101824276508909887E-16, 1.000000000000000000, -0.000000000000000000 ) ) ;
#17026 = AXIS2_PLACEMENT_3D ( 'NONE', #23406, #915, #28815 ) ;
#17027 = FACE_OUTER_BOUND ( 'NONE', #25538, .T. ) ;
#17028 = CIRCLE ( 'NONE', #2884, 58.09216821878681003 ) ;
#17029 = EDGE_CURVE ( 'NONE', #31427, #12749, #25335, .T. ) ;
#17030 = AXIS2_PLACEMENT_3D ( 'NONE', #16712, #4572, #12140 ) ;
#17031 = DIRECTION ( 'NONE',  ( -1.101824276508909887E-16, 1.000000000000000000, -0.000000000000000000 ) ) ;
#17032 = CARTESIAN_POINT ( 'NONE',  ( -36.76418579970419387, 10.14130568307076352, 56.14611646155296398 ) ) ;
#17033 = EDGE_LOOP ( 'NONE', ( #26212, #27474, #20476 ) ) ;
#17034 = VERTEX_POINT ( 'NONE', #23926 ) ;
#17035 = DIRECTION ( 'NONE',  ( -1.101824276508909887E-16, 1.000000000000000000, -0.000000000000000000 ) ) ;
#17036 = EDGE_CURVE ( 'NONE', #17110, #23862, #12218, .T. ) ;
#17037 = EDGE_CURVE ( 'NONE', #23072, #24621, #22157, .T. ) ;
#17038 = EDGE_CURVE ( 'NONE', #17244, #27529, #3745, .T. ) ;
#17039 = ORIENTED_EDGE ( 'NONE', *, *, #29081, .F. ) ;
#17040 = APPLICATION_CONTEXT ( 'automotive_design' ) ;
#17041 = VECTOR ( 'NONE', #32330, 1000.000000000000000 ) ;
#17042 = ORIENTED_EDGE ( 'NONE', *, *, #23838, .T. ) ;
#17043 = VECTOR ( 'NONE', #27409, 1000.000000000000000 ) ;
#17044 = DIRECTION ( 'NONE',  ( -1.000000000000000000, 0.000000000000000000, 0.000000000000000000 ) ) ;
#17045 = EDGE_CURVE ( 'NONE', #30194, #607, #26355, .T. ) ;
#17046 = CARTESIAN_POINT ( 'NONE',  ( 51.92400919103563695, -5.935454207752202116, -13.56214536183033381 ) ) ;
#17048 = CYLINDRICAL_SURFACE ( 'NONE', #8789, 0.1000000000000028644 ) ;
#17047 = TOROIDAL_SURFACE ( 'NONE', #20717, 70.59901951359279337, 1.000000000000000444 ) ;
#17049 = CIRCLE ( 'NONE', #7105, 72.49999999999997158 ) ;
#17050 = EDGE_LOOP ( 'NONE', ( #23950, #17198, #8403, #27248 ) ) ;
#17051 = DIRECTION ( 'NONE',  ( 0.2756373558169958327, -0.9612616959383198934, 0.000000000000000000 ) ) ;
#17052 = FACE_OUTER_BOUND ( 'NONE', #7392, .T. ) ;
#17053 = CARTESIAN_POINT ( 'NONE',  ( -63.90214402394282445, 9.925589859889722533, 52.04930799450051637 ) ) ;
#17054 = EDGE_LOOP ( 'NONE', ( #24506, #11295, #3617, #4656 ) ) ;
#17055 = VERTEX_POINT ( 'NONE', #16690 ) ;
#17056 = CARTESIAN_POINT ( 'NONE',  ( -9.728297238921268075, -5.935454207752198563, 105.1347781458764103 ) ) ;
#17057 = ORIENTED_EDGE ( 'NONE', *, *, #226, .F. ) ;
#17058 = AXIS2_PLACEMENT_3D ( 'NONE', #23789, #6718, #31673 ) ;
#17059 = DIRECTION ( 'NONE',  ( 1.000000000000000000, -3.756723415560144304E-15, 0.000000000000000000 ) ) ;
#17060 = LINE ( 'NONE', #29552, #15488 ) ;
#17061 = FACE_OUTER_BOUND ( 'NONE', #25788, .T. ) ;
#17062 = ADVANCED_FACE ( 'NONE', ( #31325 ), #20596, .T. ) ;
#17063 = DIRECTION ( 'NONE',  ( 1.000000000000000000, 0.000000000000000000, 0.000000000000000000 ) ) ;
#17064 = EDGE_LOOP ( 'NONE', ( #17578, #11413, #31029, #8381, #12752, #8500 ) ) ;
#17065 = ORIENTED_EDGE ( 'NONE', *, *, #9539, .T. ) ;
#17066 = CARTESIAN_POINT ( 'NONE',  ( 33.37634396954524618, 26.59164230456639899, 47.04930799450051637 ) ) ;
#17067 = CARTESIAN_POINT ( 'NONE',  ( -40.23397449525940317, 6.794506605641760899, 39.54930799450052348 ) ) ;
#17068 = EDGE_CURVE ( 'NONE', #16102, #8095, #24789, .T. ) ;
#17069 = CARTESIAN_POINT ( 'NONE',  ( 21.09992658989239089, 28.84164230456639544, 47.04930799450051637 ) ) ;
#17070 = EDGE_LOOP ( 'NONE', ( #8408, #8611, #480, #1970 ) ) ;
#17071 = DIRECTION ( 'NONE',  ( 0.000000000000000000, 0.000000000000000000, -1.000000000000000000 ) ) ;
#17072 = CARTESIAN_POINT ( 'NONE',  ( 21.09785597605719332, 30.56454579224779522, 47.04930799450051637 ) ) ;
#17073 = VERTEX_POINT ( 'NONE', #8996 ) ;
#17074 = DIRECTION ( 'NONE',  ( -0.2756373558169974980, 0.9612616959383193382, 1.315048337272770589E-17 ) ) ;
#17075 = CARTESIAN_POINT ( 'NONE',  ( -40.32034427004700916, 8.384459687302960873, 59.44930799450051495 ) ) ;
#17076 = AXIS2_PLACEMENT_3D ( 'NONE', #28942, #1518, #19068 ) ;
#17077 = AXIS2_PLACEMENT_3D ( 'NONE', #24127, #26921, #19192 ) ;
#17078 = EDGE_CURVE ( 'NONE', #9758, #21045, #18991, .T. ) ;
#17079 = DIRECTION ( 'NONE',  ( -1.000000000000000000, 0.000000000000000000, 0.000000000000000000 ) ) ;
#17080 = ADVANCED_FACE ( 'NONE', ( #10307 ), #7349, .F. ) ;
#17081 = AXIS2_PLACEMENT_3D ( 'NONE', #5998, #16004, #26009 ) ;
#17082 = ORIENTED_EDGE ( 'NONE', *, *, #21360, .T. ) ;
#17083 = ORIENTED_EDGE ( 'NONE', *, *, #1985, .F. ) ;
#17084 = DIRECTION ( 'NONE',  ( -0.9612616959383193382, -0.2756373558169974980, -8.795445018804950038E-19 ) ) ;
#17085 = CARTESIAN_POINT ( 'NONE',  ( 21.09785597605719687, -13.30631372918550959, 102.8621366805641770 ) ) ;
#17086 = CARTESIAN_POINT ( 'NONE',  ( 47.20547626766766314, 25.47451373492760140, 44.97710074790751378 ) ) ;
#17087 = ORIENTED_EDGE ( 'NONE', *, *, #19481, .T. ) ;
#17088 = DIRECTION ( 'NONE',  ( 0.000000000000000000, 0.000000000000000000, -1.000000000000000000 ) ) ;
#17089 = FACE_OUTER_BOUND ( 'NONE', #23898, .T. ) ;
#17090 = AXIS2_PLACEMENT_3D ( 'NONE', #1813, #4104, #31536 ) ;
#17091 = CARTESIAN_POINT ( 'NONE',  ( 21.09785597605719332, 30.56454579224779522, 47.04930799450051637 ) ) ;
#17092 = CARTESIAN_POINT ( 'NONE',  ( 21.09785597605719332, -16.63545420775219696, -32.16074251183835031 ) ) ;
#17093 = CARTESIAN_POINT ( 'NONE',  ( 21.09992658989238734, 38.56284415653841791, 47.04930799450051637 ) ) ;
#17094 = CARTESIAN_POINT ( 'NONE',  ( -40.11729073372970333, 6.802967823440400963, 39.44930799450052206 ) ) ;
#17095 = LINE ( 'NONE', #14492, #11601 ) ;
#17096 = PLANE ( 'NONE',  #24645 ) ;
#17097 = CARTESIAN_POINT ( 'NONE',  ( 21.09992658989239089, 28.59164230456639544, 47.04930799450051637 ) ) ;
#17098 = DIRECTION ( 'NONE',  ( -1.000000000000000000, 0.000000000000000000, 0.000000000000000000 ) ) ;
#17099 = ORIENTED_EDGE ( 'NONE', *, *, #23039, .F. ) ;
#17100 = CARTESIAN_POINT ( 'NONE',  ( 45.98154733146137119, 23.04411657098542676, 46.84134192585683820 ) ) ;
#17101 = DIRECTION ( 'NONE',  ( -0.4544104193609908027, 6.737912671758736131E-17, -0.8907924397839086517 ) ) ;
#17102 = CARTESIAN_POINT ( 'NONE',  ( -29.72578043774887391, 6.684485874209331158, 17.55139590643513614 ) ) ;
#17103 = VECTOR ( 'NONE', #17774, 1000.000000000000000 ) ;
#17104 = DIRECTION ( 'NONE',  ( -1.101824276508909887E-16, 1.000000000000000000, -0.000000000000000000 ) ) ;
#17105 = VERTEX_POINT ( 'NONE', #2582 ) ;
#17106 = CARTESIAN_POINT ( 'NONE',  ( -39.56610103014499202, -5.935834405102645484, 77.89388049883636711 ) ) ;
#17107 = DIRECTION ( 'NONE',  ( -1.000000000000000000, 0.000000000000000000, 0.000000000000000000 ) ) ;
#17108 = DIRECTION ( 'NONE',  ( -1.000000000000000000, 0.000000000000000000, 0.000000000000000000 ) ) ;
#17109 = VERTEX_POINT ( 'NONE', #17179 ) ;
#17110 = VERTEX_POINT ( 'NONE', #2093 ) ;
#17111 = CARTESIAN_POINT ( 'NONE',  ( 21.09785597605719332, 25.56454579224779167, 73.04930799450052348 ) ) ;
#17112 = DIRECTION ( 'NONE',  ( 1.000000000000000000, 0.000000000000000000, 0.000000000000000000 ) ) ;
#17113 = DIRECTION ( 'NONE',  ( 0.000000000000000000, -0.000000000000000000, -1.000000000000000000 ) ) ;
#17114 = EDGE_CURVE ( 'NONE', #8095, #15696, #29676, .T. ) ;
#17115 = DIRECTION ( 'NONE',  ( -0.1949050434465251780, 0.6797146636928671493, -0.7071067811865480168 ) ) ;
#17116 = EDGE_CURVE ( 'NONE', #3003, #6052, #17351, .T. ) ;
#17117 = EDGE_CURVE ( 'NONE', #1400, #12749, #682, .T. ) ;
#17118 = CARTESIAN_POINT ( 'NONE',  ( 44.74510487398335812, 29.30808892249564934, 46.84805612806227515 ) ) ;
#17119 = EDGE_LOOP ( 'NONE', ( #4569, #11284, #6484, #5131 ) ) ;
#17120 = AXIS2_PLACEMENT_3D ( 'NONE', #31494, #11308, #26238 ) ;
#17121 = ORIENTED_EDGE ( 'NONE', *, *, #23309, .T. ) ;
#17122 = CARTESIAN_POINT ( 'NONE',  ( 21.09785597605719332, 15.06454579224778456, 47.04930799450051637 ) ) ;
#17123 = AXIS2_PLACEMENT_3D ( 'NONE', #15767, #17734, #18378 ) ;
#17124 = ORIENTED_EDGE ( 'NONE', *, *, #17668, .F. ) ;
#17125 = DIRECTION ( 'NONE',  ( -1.000000000000000000, 0.000000000000000000, 0.000000000000000000 ) ) ;
#17126 = CARTESIAN_POINT ( 'NONE',  ( -29.37097840176921792, 10.01373725922364599, 73.36819798580265228 ) ) ;
#17127 = EDGE_LOOP ( 'NONE', ( #24523, #30681, #22887, #4898 ) ) ;
#17128 = CARTESIAN_POINT ( 'NONE',  ( -40.15599670534037102, 7.478908884098772525, 35.90717268343339441 ) ) ;
#17129 = ORIENTED_EDGE ( 'NONE', *, *, #19523, .F. ) ;
#17130 = DIRECTION ( 'NONE',  ( 1.000000000000000000, 0.000000000000000000, 0.000000000000000000 ) ) ;
#17131 = CARTESIAN_POINT ( 'NONE',  ( 33.46699938050304013, 24.47145308207319303, 47.04930799450050927 ) ) ;
#17132 = CARTESIAN_POINT ( 'NONE',  ( 72.87831073108154101, 11.92558985988973141, 68.00716504909145499 ) ) ;
#17133 = ORIENTED_EDGE ( 'NONE', *, *, #24722, .F. ) ;
#17134 = CARTESIAN_POINT ( 'NONE',  ( -40.02540636251513462, 2.839176264122873050, 35.54930799450051637 ) ) ;
#17135 = CARTESIAN_POINT ( 'NONE',  ( 8.698509210239523171, 25.84164230456639899, 47.04930799450051637 ) ) ;
#17137 = DIRECTION ( 'NONE',  ( 0.9986540920324801229, 1.233316085972235327E-16, 0.05186525298099653458 ) ) ;
#17136 = CIRCLE ( 'NONE', #28674, 46.53489018157424084 ) ;
#17138 = FACE_OUTER_BOUND ( 'NONE', #13464, .T. ) ;
#17139 = CARTESIAN_POINT ( 'NONE',  ( 21.09785597605719332, 15.43591091851532759, 47.04930799450051637 ) ) ;
#17140 = CARTESIAN_POINT ( 'NONE',  ( -40.18454328187963398, 7.548069831825862330, 60.44930799450051495 ) ) ;
#17141 = VERTEX_POINT ( 'NONE', #7518 ) ;
#17142 = CARTESIAN_POINT ( 'NONE',  ( 8.732853799281738105, 25.21183152705960140, 47.04930799450051637 ) ) ;
#17143 = FACE_OUTER_BOUND ( 'NONE', #9245, .T. ) ;
#17144 = ORIENTED_EDGE ( 'NONE', *, *, #9949, .T. ) ;
#17145 = CARTESIAN_POINT ( 'NONE',  ( 21.09992658989239089, 24.59164230456639544, 47.04930799450051637 ) ) ;
#17146 = EDGE_CURVE ( 'NONE', #32483, #6923, #4873, .T. ) ;
#17147 = FACE_OUTER_BOUND ( 'NONE', #12328, .T. ) ;
#17148 = EDGE_CURVE ( 'NONE', #4270, #22296, #18522, .T. ) ;
#17149 = EDGE_CURVE ( 'NONE', #15696, #12384, #22175, .T. ) ;
#17150 = ORIENTED_EDGE ( 'NONE', *, *, #21063, .F. ) ;
#17151 = EDGE_CURVE ( 'NONE', #20020, #20587, #4906, .T. ) ;
#17152 = VERTEX_POINT ( 'NONE', #4555 ) ;
#17153 = EDGE_CURVE ( 'NONE', #24330, #2165, #15222, .T. ) ;
#17154 = EDGE_CURVE ( 'NONE', #9965, #1158, #25860, .T. ) ;
#17155 = ORIENTED_EDGE ( 'NONE', *, *, #6591, .T. ) ;
#17156 = AXIS2_PLACEMENT_3D ( 'NONE', #8404, #10719, #23809 ) ;
#17157 = AXIS2_PLACEMENT_3D ( 'NONE', #13778, #3271, #8688 ) ;
#17158 = AXIS2_PLACEMENT_3D ( 'NONE', #20257, #22885, #30452 ) ;
#17159 = DIRECTION ( 'NONE',  ( 0.000000000000000000, 0.000000000000000000, 1.000000000000000000 ) ) ;
#17160 = ORIENTED_EDGE ( 'NONE', *, *, #9028, .T. ) ;
#17161 = VECTOR ( 'NONE', #30785, 1000.000000000000000 ) ;
#17162 = ORIENTED_EDGE ( 'NONE', *, *, #23572, .T. ) ;
#17163 = CARTESIAN_POINT ( 'NONE',  ( 75.92816826855421652, -3.374355247260707014, 13.38734790222314075 ) ) ;
#17164 = DIRECTION ( 'NONE',  ( 0.4848096202463430537, 0.8746197071393926326, -1.125439520643636483E-16 ) ) ;
#17165 = DIRECTION ( 'NONE',  ( -1.000000000000000000, 0.000000000000000000, 0.000000000000000000 ) ) ;
#17166 = DIRECTION ( 'NONE',  ( 0.000000000000000000, -1.668003342285388297E-15, -1.000000000000000000 ) ) ;
#17167 = DIRECTION ( 'NONE',  ( -1.000000000000000000, -1.101824276508909764E-16, 0.000000000000000000 ) ) ;
#17168 = ADVANCED_FACE ( 'NONE', ( #121 ), #1209, .T. ) ;
#17169 = EDGE_LOOP ( 'NONE', ( #23811, #26703, #4931, #24778 ) ) ;
#17170 = DIRECTION ( 'NONE',  ( -0.8746197071393925215, 0.4848096202463429982, 8.676864087101708112E-18 ) ) ;
#17171 = ORIENTED_EDGE ( 'NONE', *, *, #14465, .F. ) ;
#17172 = CARTESIAN_POINT ( 'NONE',  ( 8.474859994195286461, 28.34143805560861296, 47.04930799450051637 ) ) ;
#17173 = DIRECTION ( 'NONE',  ( 0.4544104193609900810, 5.611869858668441979E-17, 0.8907924397839090958 ) ) ;
#17174 = ORIENTED_EDGE ( 'NONE', *, *, #19102, .T. ) ;
#17175 = DIRECTION ( 'NONE',  ( -1.000000000000000000, 0.000000000000000000, 0.000000000000000000 ) ) ;
#17176 = DIRECTION ( 'NONE',  ( -0.000000000000000000, -1.000000000000000000, -0.000000000000000000 ) ) ;
#17177 = CARTESIAN_POINT ( 'NONE',  ( 52.17809377605063048, -5.936602078651307401, 107.6389665681752348 ) ) ;
#17178 = CARTESIAN_POINT ( 'NONE',  ( -43.72819403793993587, 1.315833819094413659, 34.64930799450052490 ) ) ;
#17179 = CARTESIAN_POINT ( 'NONE',  ( -30.88361636257000598, 11.92558985988973141, 67.49515520264003499 ) ) ;
#17180 = CARTESIAN_POINT ( 'NONE',  ( 46.99023568444673060, 26.43791119454915517, 49.12151524109405898 ) ) ;
#17181 = CARTESIAN_POINT ( 'NONE',  ( 47.72109904461037644, 22.93807716476589320, 48.62686290590787053 ) ) ;
#17182 = DIRECTION ( 'NONE',  ( -0.1138751963119829791, 0.8685717160922530322, -0.4823024089401439785 ) ) ;
#17183 = ORIENTED_EDGE ( 'NONE', *, *, #13321, .T. ) ;
#17184 = DIRECTION ( 'NONE',  ( 1.000000000000000000, 0.000000000000000000, 0.000000000000000000 ) ) ;
#17185 = CARTESIAN_POINT ( 'NONE',  ( 48.82187354100420151, 22.88065857334294861, 46.16985335424439540 ) ) ;
#17186 = ORIENTED_EDGE ( 'NONE', *, *, #13988, .F. ) ;
#17187 = AXIS2_PLACEMENT_3D ( 'NONE', #11891, #21394, #14031 ) ;
#17188 = DIRECTION ( 'NONE',  ( 0.000000000000000000, 1.000000000000000000, 0.000000000000000000 ) ) ;
#17189 = CARTESIAN_POINT ( 'NONE',  ( -38.57628410747783221, -3.086620340690746644, 13.27411520529475020 ) ) ;
#17190 = VECTOR ( 'NONE', #17101, 1000.000000000000114 ) ;
#17191 = ORIENTED_EDGE ( 'NONE', *, *, #10970, .F. ) ;
#17192 = TOROIDAL_SURFACE ( 'NONE', #13533, 12.40141737965286239, 0.1250000000000005551 ) ;
#17193 = ORIENTED_EDGE ( 'NONE', *, *, #30063, .T. ) ;
#17194 = DIRECTION ( 'NONE',  ( 0.4848096202463673121, 0.8746197071393789768, 0.000000000000000000 ) ) ;
#17195 = EDGE_CURVE ( 'NONE', #2754, #14753, #25357, .T. ) ;
#17196 = CIRCLE ( 'NONE', #11963, 2.000000000000001776 ) ;
#17197 = EDGE_LOOP ( 'NONE', ( #11630, #367, #3269, #19310 ) ) ;
#17198 = ORIENTED_EDGE ( 'NONE', *, *, #16806, .F. ) ;
#17199 = CARTESIAN_POINT ( 'NONE',  ( 46.18676869530867179, 23.03451764446790051, 47.84429317205637489 ) ) ;
#17200 = AXIS2_PLACEMENT_3D ( 'NONE', #27797, #25337, #20240 ) ;
#17201 = LINE ( 'NONE', #4260, #21241 ) ;
#17202 = VECTOR ( 'NONE', #6891, 1000.000000000000227 ) ;
#17203 = ADVANCED_FACE ( 'NONE', ( #9813 ), #8054, .F. ) ;
#17204 = CIRCLE ( 'NONE', #21389, 55.69429210806286079 ) ;
#17205 = VERTEX_POINT ( 'NONE', #20138 ) ;
#17206 = AXIS2_PLACEMENT_3D ( 'NONE', #21666, #31537, #2143 ) ;
#17207 = CARTESIAN_POINT ( 'NONE',  ( 21.09785597605720753, 14.86454579224779948, 47.04930799450052348 ) ) ;
#17208 =( BOUNDED_CURVE ( )  B_SPLINE_CURVE ( 2, ( #1130, #13462, #8690, #26563, #23460, #10994, #3920, #14102, #971 ),
 .UNSPECIFIED., .F., .F. ) 
 B_SPLINE_CURVE_WITH_KNOTS ( ( 3, 2, 2, 2, 3 ),
 ( 0.03571428571428342941, 0.04761904761904767192, 0.07142857142857139685, 0.09523809523809523281, 0.1071428559815845449 ),
 .UNSPECIFIED. ) 
 CURVE ( )  GEOMETRIC_REPRESENTATION_ITEM ( )  RATIONAL_B_SPLINE_CURVE ( ( 0.9330127018922194093, 0.9330127018922063087, 1.000000000000000000, 0.8660254037844387076, 1.000000000000000000, 0.8660254037844387076, 1.000000000000000000, 0.9330127084266226500, 0.9330127018922200755 ) ) 
 REPRESENTATION_ITEM ( '' )  );
#17209 = AXIS2_PLACEMENT_3D ( 'NONE', #17848, #30331, #22927 ) ;
#17210 = CARTESIAN_POINT ( 'NONE',  ( -41.52623485060432529, 12.58989991563029953, 57.04930799450051637 ) ) ;
#17211 = CARTESIAN_POINT ( 'NONE',  ( -9.987729244453721122, -5.936379232154282981, -13.33170860045786910 ) ) ;
#17212 = CARTESIAN_POINT ( 'NONE',  ( 47.20547626766766314, 25.38791119454915801, 44.97710074790751378 ) ) ;
#17213 = EDGE_CURVE ( 'NONE', #9336, #2302, #25883, .T. ) ;
#17214 = ORIENTED_EDGE ( 'NONE', *, *, #2591, .T. ) ;
#17215 = ORIENTED_EDGE ( 'NONE', *, *, #25644, .F. ) ;
#17216 = DIRECTION ( 'NONE',  ( -0.000000000000000000, 1.000000000000000000, -0.000000000000000000 ) ) ;
#17217 = EDGE_CURVE ( 'NONE', #1073, #3554, #2261, .T. ) ;
#17218 = EDGE_LOOP ( 'NONE', ( #12983, #5728, #15531, #28000 ) ) ;
#17219 = TOROIDAL_SURFACE ( 'NONE', #987, 12.61792373059899752, 0.1250000000000005274 ) ;
#17220 = LINE ( 'NONE', #22465, #16587 ) ;
#17221 = FACE_OUTER_BOUND ( 'NONE', #11495, .T. ) ;
#17222 = CARTESIAN_POINT ( 'NONE',  ( -40.69114442294517175, 6.794816359673570894, 34.71217099316726973 ) ) ;
#17223 = CARTESIAN_POINT ( 'NONE',  ( 48.14727188781975542, 22.86454579224779948, 49.10650501410607660 ) ) ;
#17224 = CARTESIAN_POINT ( 'NONE',  ( 48.18662509608405742, 26.49624452788248519, 49.18364984542562013 ) ) ;
#17225 = VERTEX_POINT ( 'NONE', #5214 ) ;
#17226 = ORIENTED_EDGE ( 'NONE', *, *, #10655, .F. ) ;
#17227 = DIRECTION ( 'NONE',  ( -1.000000000000000000, 0.000000000000000000, 0.000000000000000000 ) ) ;
#17228 = LINE ( 'NONE', #24296, #21390 ) ;
#17229 = DIRECTION ( 'NONE',  ( 0.1949050434465281201, -0.6797146636928673713, 0.7071067811865470176 ) ) ;
#17230 = VERTEX_POINT ( 'NONE', #2749 ) ;
#17231 = CARTESIAN_POINT ( 'NONE',  ( 46.00908685603033632, 29.03284706826092076, 44.91496614357595263 ) ) ;
#17232 = CARTESIAN_POINT ( 'NONE',  ( 24.90860134598590037, -13.74047052604243824, 105.2732083934160983 ) ) ;
#17233 = VERTEX_POINT ( 'NONE', #923 ) ;
#17234 = CARTESIAN_POINT ( 'NONE',  ( -43.37834615508418068, 1.121909970995877304, 39.54930799450052348 ) ) ;
#17235 = DIRECTION ( 'NONE',  ( -0.000000000000000000, -1.000000000000000000, 0.000000000000000000 ) ) ;
#17236 = EDGE_CURVE ( 'NONE', #20563, #5070, #31120, .T. ) ;
#17237 = CIRCLE ( 'NONE', #3601, 0.9031915329475500576 ) ;
#17238 = AXIS2_PLACEMENT_3D ( 'NONE', #14107, #9947, #1787 ) ;
#17239 = CARTESIAN_POINT ( 'NONE',  ( 8.698509210239553369, 28.59164230456639544, 47.04930799450051637 ) ) ;
#17240 = AXIS2_PLACEMENT_3D ( 'NONE', #23620, #16221, #23299 ) ;
#17241 = CIRCLE ( 'NONE', #28275, 12.62506659569710266 ) ;
#17242 = ORIENTED_EDGE ( 'NONE', *, *, #15481, .T. ) ;
#17243 = AXIS2_PLACEMENT_3D ( 'NONE', #10348, #20343, #7891 ) ;
#17244 = VERTEX_POINT ( 'NONE', #18316 ) ;
#17245 = EDGE_CURVE ( 'NONE', #25249, #26367, #13097, .T. ) ;
#17246 = CARTESIAN_POINT ( 'NONE',  ( -38.34716389643126178, -5.918128512222508242, 15.86828009547534890 ) ) ;
#17247 = CARTESIAN_POINT ( 'NONE',  ( 21.09785597605720753, 14.36454579224779948, 47.04930799450052348 ) ) ;
#17248 = CARTESIAN_POINT ( 'NONE',  ( 21.09992658989239089, 28.71664230456639899, 47.04930799450051637 ) ) ;
#17249 = EDGE_CURVE ( 'NONE', #24454, #20832, #21660, .T. ) ;
#17250 = VERTEX_POINT ( 'NONE', #23415 ) ;
#17251 = CYLINDRICAL_SURFACE ( 'NONE', #25909, 12.36707279061065101 ) ;
#17252 = DIRECTION ( 'NONE',  ( 0.000000000000000000, 0.000000000000000000, -1.000000000000000000 ) ) ;
#17253 = AXIS2_PLACEMENT_3D ( 'NONE', #1881, #23879, #11255 ) ;
#17254 = EDGE_CURVE ( 'NONE', #8280, #30637, #17840, .T. ) ;
#17255 = DIRECTION ( 'NONE',  ( -0.000000000000000000, -1.000000000000000000, 0.000000000000000000 ) ) ;
#17256 = EDGE_CURVE ( 'NONE', #15396, #6997, #24290, .T. ) ;
#17257 = DIRECTION ( 'NONE',  ( 0.9612616959383205595, 0.2756373558169932236, -1.660411357259282445E-16 ) ) ;
#17258 = CARTESIAN_POINT ( 'NONE',  ( 34.59963999142011204, -5.098646251524523443, 47.04930799450052348 ) ) ;
#17259 = PLANE ( 'NONE',  #25750 ) ;
#17260 = DIRECTION ( 'NONE',  ( -0.9612616959383206705, -0.2756373558169931681, 1.660411357259282445E-16 ) ) ;
#17261 = CARTESIAN_POINT ( 'NONE',  ( 21.09785597605719332, 24.86454579224779948, 70.54930799450050927 ) ) ;
#17262 = CARTESIAN_POINT ( 'NONE',  ( -43.29662792673757110, 1.063067023446604864, 60.44930799450051495 ) ) ;
#17263 = EDGE_LOOP ( 'NONE', ( #11467, #21305, #32084, #27154 ) ) ;
#17264 = ORIENTED_EDGE ( 'NONE', *, *, #22238, .F. ) ;
#17265 = DIRECTION ( 'NONE',  ( 0.000000000000000000, -0.000000000000000000, -1.000000000000000000 ) ) ;
#17266 = CARTESIAN_POINT ( 'NONE',  ( 48.28214861297873739, 24.78954579807170333, 49.37090702980594159 ) ) ;
#17267 = CYLINDRICAL_SURFACE ( 'NONE', #31845, 12.62506659569710266 ) ;
#17268 = CIRCLE ( 'NONE', #28800, 13.31487396812510937 ) ;
#17269 = AXIS2_PLACEMENT_3D ( 'NONE', #2024, #10239, #20235 ) ;
#17270 = DIRECTION ( 'NONE',  ( -1.000000000000000000, 0.000000000000000000, 0.000000000000000000 ) ) ;
#17271 = ORIENTED_EDGE ( 'NONE', *, *, #4813, .T. ) ;
#17272 = CARTESIAN_POINT ( 'NONE',  ( 21.09785597605720397, -15.72540370141337007, -24.25069200549945947 ) ) ;
#17273 = DIRECTION ( 'NONE',  ( -0.000000000000000000, -1.000000000000000000, 0.000000000000000000 ) ) ;
#17274 = DIRECTION ( 'NONE',  ( -1.101824276508909887E-16, 1.000000000000000000, -0.000000000000000000 ) ) ;
#17275 = ORIENTED_EDGE ( 'NONE', *, *, #14454, .F. ) ;
#17276 = ORIENTED_EDGE ( 'NONE', *, *, #21922, .T. ) ;
#17277 = CARTESIAN_POINT ( 'NONE',  ( -40.10917099319649282, 6.845611892227015716, 39.49480556904257611 ) ) ;
#17278 = CARTESIAN_POINT ( 'NONE',  ( 48.18662509608405031, 29.38284706826092574, 49.18364984542562013 ) ) ;
#17279 = CARTESIAN_POINT ( 'NONE',  ( -63.90214402394282445, 11.92558985988973497, 26.63511333407100778 ) ) ;
#17280 = LINE ( 'NONE', #10078, #20111 ) ;
#17281 = CARTESIAN_POINT ( 'NONE',  ( 7.096071960694297687, 16.03967147762300982, 47.04930799450052348 ) ) ;
#17282 = EDGE_LOOP ( 'NONE', ( #27584, #7002, #31493, #5090 ) ) ;
#17283 = AXIS2_PLACEMENT_3D ( 'NONE', #32087, #14526, #22720 ) ;
#17284 = AXIS2_PLACEMENT_3D ( 'NONE', #11528, #31560, #1030 ) ;
#17285 = EDGE_LOOP ( 'NONE', ( #4871, #16854 ) ) ;
#17286 = EDGE_CURVE ( 'NONE', #12709, #11810, #11201, .T. ) ;
#17287 = DIRECTION ( 'NONE',  ( 0.000000000000000000, 1.000000000000000000, -0.000000000000000000 ) ) ;
#17288 = AXIS2_PLACEMENT_3D ( 'NONE', #18032, #5571, #3089 ) ;
#17289 = AXIS2_PLACEMENT_3D ( 'NONE', #5923, #20686, #25772 ) ;
#17290 = EDGE_CURVE ( 'NONE', #23918, #24672, #17986, .T. ) ;
#17291 = VERTEX_POINT ( 'NONE', #5696 ) ;
#17292 = CIRCLE ( 'NONE', #30414, 13.31487396812510937 ) ;
#17293 = DIRECTION ( 'NONE',  ( 0.8746197071393925215, -0.4848096202463429982, -8.676864087101708112E-18 ) ) ;
#17294 = DIRECTION ( 'NONE',  ( -1.101824276508909887E-16, 1.000000000000000000, -0.000000000000000000 ) ) ;
#17295 = AXIS2_PLACEMENT_3D ( 'NONE', #30493, #15221, #12773 ) ;
#17296 = VECTOR ( 'NONE', #20388, 1000.000000000000000 ) ;
#17297 = EDGE_CURVE ( 'NONE', #22668, #2021, #26919, .T. ) ;
#17298 = VERTEX_POINT ( 'NONE', #20788 ) ;
#17299 = CARTESIAN_POINT ( 'NONE',  ( -40.86270455615213848, 8.492915053331742570, 34.63740864294511823 ) ) ;
#17300 = ORIENTED_EDGE ( 'NONE', *, *, #23632, .T. ) ;
#17301 = CARTESIAN_POINT ( 'NONE',  ( 21.09992658989239089, 29.59164230456639899, 47.04930799450051637 ) ) ;
#17302 = DIRECTION ( 'NONE',  ( -2.779292025043186357E-18, 1.288349127009862211E-17, -1.000000000000000000 ) ) ;
#17303 = CARTESIAN_POINT ( 'NONE',  ( 71.88636670473840695, 11.19016079752308634, 71.26986100341954966 ) ) ;
#17304 = ORIENTED_EDGE ( 'NONE', *, *, #161, .T. ) ;
#17305 = CYLINDRICAL_SURFACE ( 'NONE', #6563, 12.36707279061065279 ) ;
#17306 = DIRECTION ( 'NONE',  ( -1.000000000000000000, 0.000000000000000000, 0.000000000000000000 ) ) ;
#17307 = CARTESIAN_POINT ( 'NONE',  ( -9.982381823936176346, -5.936602078651308290, -13.54035057917421270 ) ) ;
#17308 = VECTOR ( 'NONE', #23997, 999.9999999999998863 ) ;
#17309 = CARTESIAN_POINT ( 'NONE',  ( -40.02540636251513462, 2.839176264122873050, 37.04930799450052348 ) ) ;
#17310 = ORIENTED_EDGE ( 'NONE', *, *, #2623, .F. ) ;
#17311 = FACE_OUTER_BOUND ( 'NONE', #31857, .T. ) ;
#17312 = FACE_OUTER_BOUND ( 'NONE', #17537, .T. ) ;
#17313 = ORIENTED_EDGE ( 'NONE', *, *, #15165, .F. ) ;
#17314 = DIRECTION ( 'NONE',  ( -1.101824276508909887E-16, 1.000000000000000000, -0.000000000000000000 ) ) ;
#17315 = AXIS2_PLACEMENT_3D ( 'NONE', #9117, #1402, #16335 ) ;
#17316 = FACE_OUTER_BOUND ( 'NONE', #5325, .T. ) ;
#17317 = ORIENTED_EDGE ( 'NONE', *, *, #25011, .F. ) ;
#17318 = AXIS2_PLACEMENT_3D ( 'NONE', #19849, #12969, #7712 ) ;
#17319 = EDGE_LOOP ( 'NONE', ( #8878, #15085, #9860, #21654, #17509 ) ) ;
#17320 = AXIS2_PLACEMENT_3D ( 'NONE', #3544, #21097, #13568 ) ;
#17321 = AXIS2_PLACEMENT_3D ( 'NONE', #24464, #1979, #6744 ) ;
#17322 = AXIS2_PLACEMENT_3D ( 'NONE', #3303, #8831, #5775 ) ;
#17323 = VERTEX_POINT ( 'NONE', #25721 ) ;
#17324 = DIRECTION ( 'NONE',  ( 0.000000000000000000, -1.000000000000000000, 0.000000000000000000 ) ) ;
#17325 = ADVANCED_FACE ( 'NONE', ( #18156 ), #15541, .F. ) ;
#17326 = AXIS2_PLACEMENT_3D ( 'NONE', #11904, #2222, #22391 ) ;
#17327 = EDGE_LOOP ( 'NONE', ( #20496, #27633, #16872, #1407 ) ) ;
#17328 = ORIENTED_EDGE ( 'NONE', *, *, #26081, .T. ) ;
#17329 = CARTESIAN_POINT ( 'NONE',  ( 21.09992658989239089, 27.59164230456639544, 47.04930799450051637 ) ) ;
#17330 = ADVANCED_FACE ( 'NONE', ( #10948 ), #30070, .T. ) ;
#17331 = EDGE_CURVE ( 'NONE', #20581, #28135, #28508, .T. ) ;
#17332 = CYLINDRICAL_SURFACE ( 'NONE', #14647, 12.62506659569710266 ) ;
#17333 = ADVANCED_FACE ( 'NONE', ( #30494 ), #10157, .T. ) ;
#17334 = CIRCLE ( 'NONE', #10547, 32.50000000000000000 ) ;
#17335 = FACE_OUTER_BOUND ( 'NONE', #10693, .T. ) ;
#17336 = CARTESIAN_POINT ( 'NONE',  ( -40.28779227465695101, 2.984619150196775816, 37.04930799450052348 ) ) ;
#17337 = VECTOR ( 'NONE', #20534, 999.9999999999998863 ) ;
#17338 = DIRECTION ( 'NONE',  ( 0.000000000000000000, -0.7071067811865426878, -0.7071067811865524577 ) ) ;
#17339 = VECTOR ( 'NONE', #28337, 1000.000000000000000 ) ;
#17340 = ORIENTED_EDGE ( 'NONE', *, *, #14912, .F. ) ;
#17342 = ADVANCED_FACE ( 'NONE', ( #8485 ), #31630, .T. ) ;
#17341 = LINE ( 'NONE', #12109, #10751 ) ;
#17343 = ORIENTED_EDGE ( 'NONE', *, *, #30539, .F. ) ;
#17344 = CARTESIAN_POINT ( 'NONE',  ( -10.80400125034478087, -5.721341737285083440, -11.23070561388631816 ) ) ;
#17345 = CARTESIAN_POINT ( 'NONE',  ( -40.02540636251513462, 2.839176264122873050, 37.04930799450052348 ) ) ;
#17346 = VECTOR ( 'NONE', #10270, 1000.000000000000000 ) ;
#17347 = VERTEX_POINT ( 'NONE', #6022 ) ;
#17348 = CARTESIAN_POINT ( 'NONE',  ( 21.09992658989238734, 31.59143805560860585, 47.04930799450051637 ) ) ;
#17349 = DIRECTION ( 'NONE',  ( -0.5442436726714897643, -6.721291001053910056E-17, 0.8389271868029121171 ) ) ;
#17350 = CARTESIAN_POINT ( 'NONE',  ( 48.52450352821730917, 22.84434098701873594, 45.44469437819130775 ) ) ;
#17351 = LINE ( 'NONE', #4723, #14846 ) ;
#17352 = CARTESIAN_POINT ( 'NONE',  ( 44.70507715278255745, 29.76291119454914380, 46.92503878583764987 ) ) ;
#17353 = DIRECTION ( 'NONE',  ( -1.000000000000000000, 0.000000000000000000, -1.110223024625155594E-14 ) ) ;
#17354 = ORIENTED_EDGE ( 'NONE', *, *, #31432, .T. ) ;
#17355 = DIRECTION ( 'NONE',  ( -1.000000000000000000, 0.000000000000000000, 0.000000000000000000 ) ) ;
#17356 = DIRECTION ( 'NONE',  ( 1.234978253042719660E-16, -1.000000000000000000, -1.109335647967047851E-31 ) ) ;
#17357 = VERTEX_POINT ( 'NONE', #18001 ) ;
#17358 = VECTOR ( 'NONE', #19748, 999.9999999999998863 ) ;
#17359 = CARTESIAN_POINT ( 'NONE',  ( 8.482002859293798380, 31.21664230456641675, 47.04930799450051637 ) ) ;
#17360 = CARTESIAN_POINT ( 'NONE',  ( 21.09785597605719332, 48.06454579224779877, 47.04930799450051637 ) ) ;
#17361 = VERTEX_POINT ( 'NONE', #16023 ) ;
#17362 = ORIENTED_EDGE ( 'NONE', *, *, #18608, .F. ) ;
#17363 = DIRECTION ( 'NONE',  ( 0.000000000000000000, -1.000000000000000000, 0.000000000000000000 ) ) ;
#17364 = VERTEX_POINT ( 'NONE', #11115 ) ;
#17365 = CIRCLE ( 'NONE', #3210, 85.00000000000001421 ) ;
#17366 = TOROIDAL_SURFACE ( 'NONE', #18394, 55.59552431147871232, 0.3000000000000000444 ) ;
#17367 = CIRCLE ( 'NONE', #3659, 0.1249999999999966416 ) ;
#17368 = ORIENTED_EDGE ( 'NONE', *, *, #28610, .T. ) ;
#17369 = CARTESIAN_POINT ( 'NONE',  ( 46.65195039438923885, 23.10527865767145173, 47.43093233858343893 ) ) ;
#17370 = CARTESIAN_POINT ( 'NONE',  ( 52.07598125402753197, -5.935454207809698346, -13.48459002699794063 ) ) ;
#17371 = B_SPLINE_CURVE_WITH_KNOTS ( 'NONE', 3,
 ( #30093, #12370, #32059, #2014, #19406, #22357, #25155, #12030, #6943, #27615, #15147, #9897, #29930, #7600, #17601, #22027, #2672, #7106, #30738, #15790, #7929, #13339, #23496, #2826, #13012, #15945, #28112, #690, #5944, #849, #20224, #30575, #10225, #27780, #10717, #30249 ),
 .UNSPECIFIED., .F., .F.,
 ( 4, 2, 2, 2, 2, 2, 2, 2, 2, 2, 2, 2, 2, 2, 2, 2, 2, 4 ),
 ( 0.000000000000000000, 0.0006656200208596437786, 0.001331240041719287557, 0.002662480083438588125, 0.003993720125157888476, 0.004659340146017538868, 0.005324960166877188393, 0.005990580187736837051, 0.006656200208596487443, 0.007987440250315787360, 0.009318680292035086410, 0.01064992033375438546, 0.01331240041719299570, 0.01464364045891230169, 0.01597488050063160941, 0.01863736058407022139, 0.01996860062578953085, 0.02129984066750884725 ),
 .UNSPECIFIED. ) ;
#17372 = AXIS2_PLACEMENT_3D ( 'NONE', #28689, #6205, #28860 ) ;
#17373 = ORIENTED_EDGE ( 'NONE', *, *, #31790, .T. ) ;
#17374 = ADVANCED_FACE ( 'NONE', ( #26029 ), #1747, .T. ) ;
#17375 = EDGE_CURVE ( 'NONE', #21481, #14836, #20100, .T. ) ;
#17376 = LINE ( 'NONE', #8032, #4660 ) ;
#17377 = ADVANCED_FACE ( 'NONE', ( #31135 ), #23241, .T. ) ;
#17378 = DIRECTION ( 'NONE',  ( -1.000000000000000000, 0.000000000000000000, -1.224646799147353207E-16 ) ) ;
#17379 = DIRECTION ( 'NONE',  ( 0.000000000000000000, 0.000000000000000000, -1.000000000000000000 ) ) ;
#17380 = ADVANCED_FACE ( 'NONE', ( #26191 ), #10683, .F. ) ;
#17381 = CARTESIAN_POINT ( 'NONE',  ( 45.24946171279598417, 27.02124452788248732, 47.99220971130007030 ) ) ;
#17382 = ORIENTED_EDGE ( 'NONE', *, *, #29875, .F. ) ;
#17383 = ORIENTED_EDGE ( 'NONE', *, *, #12914, .T. ) ;
#17384 = DIRECTION ( 'NONE',  ( -1.000000000000000000, -1.101824276508909887E-16, 0.000000000000000000 ) ) ;
#17385 = EDGE_LOOP ( 'NONE', ( #18698, #5103, #20975, #23061 ) ) ;
#17386 = DIRECTION ( 'NONE',  ( -1.101824276508909887E-16, 1.000000000000000000, -0.000000000000000000 ) ) ;
#17387 = AXIS2_PLACEMENT_3D ( 'NONE', #22229, #22725, #29795 ) ;
#17388 = CARTESIAN_POINT ( 'NONE',  ( -40.15225626691278649, 6.735663658092487793, 60.54930799450051637 ) ) ;
#17389 = DIRECTION ( 'NONE',  ( -1.101824276508909887E-16, 1.000000000000000000, -0.000000000000000000 ) ) ;
#17390 = AXIS2_PLACEMENT_3D ( 'NONE', #19792, #22583, #4704 ) ;
#17391 = TOROIDAL_SURFACE ( 'NONE', #32088, 1.142135311067127068, 0.1000000000000000056 ) ;
#17392 = FACE_OUTER_BOUND ( 'NONE', #3857, .T. ) ;
#17393 = CARTESIAN_POINT ( 'NONE',  ( 45.35708200440645044, 26.90457786121582018, 45.92000246470680480 ) ) ;
#17394 = PRODUCT_CONTEXT ( 'NONE', #10786, 'mechanical' ) ;
#17395 = EDGE_LOOP ( 'NONE', ( #12455, #17452, #15103, #2779 ) ) ;
#17396 = ORIENTED_EDGE ( 'NONE', *, *, #3931, .T. ) ;
#17397 = DIRECTION ( 'NONE',  ( 0.3597811455230787714, -0.7883456110718085608, -0.4990678559373643575 ) ) ;
#17398 = DIRECTION ( 'NONE',  ( -1.101824276508909887E-16, 1.000000000000000000, -0.000000000000000000 ) ) ;
#17399 = DIRECTION ( 'NONE',  ( -0.2530443915477366690, 0.8824706660164322036, 0.3965022818682769623 ) ) ;
#17400 = ORIENTED_EDGE ( 'NONE', *, *, #2031, .T. ) ;
#17401 = CARTESIAN_POINT ( 'NONE',  ( 47.20547626766765603, 28.97451373492759430, 44.97710074790751378 ) ) ;
#17402 = ORIENTED_EDGE ( 'NONE', *, *, #10231, .T. ) ;
#17403 = CARTESIAN_POINT ( 'NONE',  ( 21.09785597605719332, 17.16451738380053627, 47.04930799450051637 ) ) ;
#17404 = CARTESIAN_POINT ( 'NONE',  ( 21.09785597605720753, 14.86454579224779948, 47.04930799450052348 ) ) ;
#17405 = CARTESIAN_POINT ( 'NONE',  ( 21.09785597605719687, 30.56454579224779522, 78.34930799450049221 ) ) ;
#17406 = CIRCLE ( 'NONE', #633, 12.62506659569710443 ) ;
#17407 = EDGE_CURVE ( 'NONE', #18982, #5510, #4196, .T. ) ;
#17408 = EDGE_CURVE ( 'NONE', #10801, #30753, #24217, .T. ) ;
#17409 = AXIS2_PLACEMENT_3D ( 'NONE', #28537, #3739, #1119 ) ;
#17410 = ORIENTED_EDGE ( 'NONE', *, *, #21424, .F. ) ;
#17411 = AXIS2_PLACEMENT_3D ( 'NONE', #25325, #1284, #13615 ) ;
#17412 =( BOUNDED_CURVE ( )  B_SPLINE_CURVE ( 3, ( #3539, #13413, #10632, #13730 ),
 .UNSPECIFIED., .F., .F. ) 
 B_SPLINE_CURVE_WITH_KNOTS ( ( 4, 4 ),
 ( 5.062864179022701805, 5.184122060454622982 ),
 .UNSPECIFIED. ) 
 CURVE ( )  GEOMETRIC_REPRESENTATION_ITEM ( )  RATIONAL_B_SPLINE_CURVE ( ( 1.000000000000000000, 0.9987750858034806223, 0.9987750858034806223, 1.000000000000000000 ) ) 
 REPRESENTATION_ITEM ( '' )  );
#17413 = ORIENTED_EDGE ( 'NONE', *, *, #9667, .T. ) ;
#17414 = CARTESIAN_POINT ( 'NONE',  ( 21.09992658989239089, 25.59164230456639899, 47.04930799450051637 ) ) ;
#17415 = CARTESIAN_POINT ( 'NONE',  ( 21.09785597605720753, -13.98292989133646103, 105.7214871010043709 ) ) ;
#17416 = CARTESIAN_POINT ( 'NONE',  ( 45.79384627280941089, 26.46618040159426144, 49.05938063676249072 ) ) ;
#17417 = ORIENTED_EDGE ( 'NONE', *, *, #10814, .F. ) ;
#17418 = DIRECTION ( 'NONE',  ( -1.000000000000000000, 0.000000000000000000, -1.224646799147353207E-16 ) ) ;
#17419 = FACE_OUTER_BOUND ( 'NONE', #22278, .T. ) ;
#17420 = EDGE_CURVE ( 'NONE', #13945, #2441, #7000, .T. ) ;
#17421 = CYLINDRICAL_SURFACE ( 'NONE', #30465, 54.29999999999999716 ) ;
#17422 = FACE_OUTER_BOUND ( 'NONE', #30589, .T. ) ;
#17423 = DIRECTION ( 'NONE',  ( -1.000000000000000000, 0.000000000000000000, 0.000000000000000000 ) ) ;
#17424 = CARTESIAN_POINT ( 'NONE',  ( -40.50726676055796105, 7.559560307024983494, 60.29072935073781991 ) ) ;
#17425 = CARTESIAN_POINT ( 'NONE',  ( 21.09992658989239089, 26.09164230456639899, 47.04930799450051637 ) ) ;
#17426 = CARTESIAN_POINT ( 'NONE',  ( 45.84097905237065618, 19.96454579224779380, 48.98672734302541443 ) ) ;
#17427 = DIRECTION ( 'NONE',  ( -0.000000000000000000, 1.000000000000000000, -0.000000000000000000 ) ) ;
#17428 = AXIS2_PLACEMENT_3D ( 'NONE', #7049, #24940, #27562 ) ;
#17429 = CARTESIAN_POINT ( 'NONE',  ( -40.60086716196818202, 6.831234436378517572, 39.54151698899572409 ) ) ;
#17430 =( LENGTH_UNIT ( ) NAMED_UNIT ( * ) SI_UNIT ( .MILLI., .METRE. ) );
#17431 = VERTEX_POINT ( 'NONE', #28659 ) ;
#17432 = ORIENTED_EDGE ( 'NONE', *, *, #31145, .T. ) ;
#17433 = DIRECTION ( 'NONE',  ( -1.000000000000000000, 0.000000000000000000, 0.000000000000000000 ) ) ;
#17434 = DIRECTION ( 'NONE',  ( -1.000000000000000000, 0.000000000000000000, 0.000000000000000000 ) ) ;
#17435 = CIRCLE ( 'NONE', #3280, 0.1000000000000007272 ) ;
#17436 = DIRECTION ( 'NONE',  ( -1.101824276508909887E-16, 1.000000000000000000, -0.000000000000000000 ) ) ;
#17437 = CARTESIAN_POINT ( 'NONE',  ( 71.48501281440437083, 9.702389020015065313, 73.75010705023585444 ) ) ;
#17438 = ORIENTED_EDGE ( 'NONE', *, *, #18599, .T. ) ;
#17439 = VECTOR ( 'NONE', #13902, 1000.000000000000114 ) ;
#17440 = CARTESIAN_POINT ( 'NONE',  ( -40.18454328187963398, 7.548069831825862330, 53.64930799450051779 ) ) ;
#17441 = DIRECTION ( 'NONE',  ( -0.000000000000000000, -1.000000000000000000, -0.000000000000000000 ) ) ;
#17442 = ADVANCED_FACE ( 'NONE', ( #23732 ), #28824, .F. ) ;
#17443 = ORIENTED_EDGE ( 'NONE', *, *, #2605, .T. ) ;
#17444 = ORIENTED_EDGE ( 'NONE', *, *, #19585, .T. ) ;
#17445 = CARTESIAN_POINT ( 'NONE',  ( -42.50084779003665147, 14.56798984196178637, 37.04930799450052348 ) ) ;
#17446 = DIRECTION ( 'NONE',  ( -0.2756373558169938898, 0.9612616959383203374, 4.550099067471054416E-15 ) ) ;
#17447 = B_SPLINE_CURVE_WITH_KNOTS ( 'NONE', 3,
 ( #388, #13046, #2855, #30444, #3338, #20738, #22721, #30923, #3493, #874 ),
 .UNSPECIFIED., .F., .F.,
 ( 4, 2, 2, 2, 4 ),
 ( 0.0006716755660530363079, 0.002413276598758840909, 0.004154877631464645726, 0.005896478664170449677, 0.007638079696876254494 ),
 .UNSPECIFIED. ) ;
#17448 = DIRECTION ( 'NONE',  ( -1.101824276508909887E-16, 1.000000000000000000, -0.000000000000000000 ) ) ;
#17449 = ADVANCED_FACE ( 'NONE', ( #11269 ), #4373, .T. ) ;
#17450 = DIRECTION ( 'NONE',  ( 1.000000000000000000, 0.000000000000000000, 0.000000000000000000 ) ) ;
#17451 = CARTESIAN_POINT ( 'NONE',  ( 46.48213017528662760, 29.40643497231507553, 49.22721246743694223 ) ) ;
#17452 = ORIENTED_EDGE ( 'NONE', *, *, #5127, .T. ) ;
#17453 = EDGE_CURVE ( 'NONE', #20511, #29530, #21140, .T. ) ;
#17454 = EDGE_CURVE ( 'NONE', #22296, #16912, #9610, .T. ) ;
#17455 = ORIENTED_EDGE ( 'NONE', *, *, #20567, .T. ) ;
#17456 = EDGE_CURVE ( 'NONE', #5065, #17073, #12242, .T. ) ;
#17457 = AXIS2_PLACEMENT_3D ( 'NONE', #21452, #19316, #14255 ) ;
#17458 = AXIS2_PLACEMENT_3D ( 'NONE', #21441, #11140, #28682 ) ;
#17459 = CYLINDRICAL_SURFACE ( 'NONE', #22435, 12.62506659569710443 ) ;
#17460 = EDGE_LOOP ( 'NONE', ( #26966, #30418, #2444, #4702 ) ) ;
#17461 = VECTOR ( 'NONE', #4330, 999.9999999999998863 ) ;
#17462 = AXIS2_PLACEMENT_3D ( 'NONE', #23766, #10833, #20824 ) ;
#17463 = DIRECTION ( 'NONE',  ( 0.2756373558169954996, -0.9612616959383200044, 2.463803012461673974E-31 ) ) ;
#17464 = LINE ( 'NONE', #5155, #18221 ) ;
#17465 = EDGE_CURVE ( 'NONE', #16982, #5110, #3319, .T. ) ;
#17466 = EDGE_LOOP ( 'NONE', ( #19149, #13877, #22768, #29439 ) ) ;
#17467 = DIRECTION ( 'NONE',  ( -1.000000000000000000, -1.101824276508909887E-16, 0.000000000000000000 ) ) ;
#17468 = ORIENTED_EDGE ( 'NONE', *, *, #19142, .T. ) ;
#17469 = DIRECTION ( 'NONE',  ( -1.101824276508909887E-16, 1.000000000000000000, -0.000000000000000000 ) ) ;
#17470 = DIRECTION ( 'NONE',  ( -1.224646799147353207E-16, -1.349345573449484691E-32, 1.000000000000000000 ) ) ;
#17471 = DIRECTION ( 'NONE',  ( -1.101824276508909887E-16, 1.000000000000000000, -0.000000000000000000 ) ) ;
#17472 = CARTESIAN_POINT ( 'NONE',  ( 8.732853799281734553, 38.56284415653841791, 47.04930799450051637 ) ) ;
#17473 = ORIENTED_EDGE ( 'NONE', *, *, #5822, .T. ) ;
#17474 = CARTESIAN_POINT ( 'NONE',  ( 21.09992658989239089, 26.22145308207318593, 47.04930799450051637 ) ) ;
#17475 = CARTESIAN_POINT ( 'NONE',  ( 8.474859994195286461, 30.34184655352422411, 47.04930799450051637 ) ) ;
#17476 = CARTESIAN_POINT ( 'NONE',  ( 21.09785597605719332, 25.56454579224779877, 21.04930799450051282 ) ) ;
#17477 = DIRECTION ( 'NONE',  ( 1.000000000000000000, 0.000000000000000000, 0.000000000000000000 ) ) ;
#17478 = AXIS2_PLACEMENT_3D ( 'NONE', #31290, #24048, #11747 ) ;
#17479 = CARTESIAN_POINT ( 'NONE',  ( 74.51022843571014675, 1.102830191788943592, 79.80751175580223844 ) ) ;
#17480 = ORIENTED_EDGE ( 'NONE', *, *, #6155, .F. ) ;
#17481 = CARTESIAN_POINT ( 'NONE',  ( -42.38351229602917414, 14.72295342448899191, 58.95959122802360497 ) ) ;
#17482 = DIRECTION ( 'NONE',  ( 0.9612616959383221138, 0.2756373558169876170, 0.000000000000000000 ) ) ;
#17483 = AXIS2_PLACEMENT_3D ( 'NONE', #2080, #12105, #22095 ) ;
#17484 = ADVANCED_FACE ( 'NONE', ( #1729 ), #702, .T. ) ;
#17485 = ORIENTED_EDGE ( 'NONE', *, *, #8743, .F. ) ;
#17486 = DIRECTION ( 'NONE',  ( -1.224646799147353207E-16, -1.349345573449484691E-32, 1.000000000000000000 ) ) ;
#17487 =( REPRESENTATION_RELATIONSHIP ('NONE','NONE', #20382, #14743 ) REPRESENTATION_RELATIONSHIP_WITH_TRANSFORMATION ( #20983 )SHAPE_REPRESENTATION_RELATIONSHIP( ) );
#17488 = EDGE_CURVE ( 'NONE', #8205, #26804, #16435, .T. ) ;
#17489 = CARTESIAN_POINT ( 'NONE',  ( -40.65093765668705572, 9.567768634527945792, 38.44930799450052916 ) ) ;
#17490 = VECTOR ( 'NONE', #5985, 1000.000000000000000 ) ;
#17491 = ORIENTED_EDGE ( 'NONE', *, *, #15279, .T. ) ;
#17492 = AXIS2_PLACEMENT_3D ( 'NONE', #4121, #16431, #19373 ) ;
#17493 = DIRECTION ( 'NONE',  ( 0.000000000000000000, 0.000000000000000000, 1.000000000000000000 ) ) ;
#17494 = CIRCLE ( 'NONE', #20632, 12.62506659569710266 ) ;
#17495 = ORIENTED_EDGE ( 'NONE', *, *, #6146, .F. ) ;
#17496 = ADVANCED_FACE ( 'NONE', ( #26354 ), #13893, .T. ) ;
#17497 = EDGE_LOOP ( 'NONE', ( #8049, #29611, #20387, #22812 ) ) ;
#17498 = B_SPLINE_CURVE_WITH_KNOTS ( 'NONE', 3,
 ( #11739, #17132, #26836, #29630, #6975, #17303, #14696, #2047, #11899, #24863 ),
 .UNSPECIFIED., .F., .F.,
 ( 4, 2, 2, 2, 4 ),
 ( 0.0006731324393516282178, 0.002417216000136556808, 0.004161299560921485723, 0.005905383121706414204, 0.007649466682491342685 ),
 .UNSPECIFIED. ) ;
#17499 = B_SPLINE_CURVE_WITH_KNOTS ( 'NONE', 3,
 ( #11150, #16215, #10986, #3748, #18827, #23131, #21132, #8683, #13773, #28866, #18354, #1273 ),
 .UNSPECIFIED., .F., .F.,
 ( 4, 2, 2, 2, 2, 4 ),
 ( 0.0003422370341462293653, 0.002080102550335782494, 0.003817968066525336598, 0.005555833582714891569, 0.006424766340809668838, 0.007293699098904446107 ),
 .UNSPECIFIED. ) ;
#17500 = CARTESIAN_POINT ( 'NONE',  ( 8.482002859293784169, 30.21664230456641675, 47.04930799450051637 ) ) ;
#17501 = EDGE_LOOP ( 'NONE', ( #25264, #27855, #17271, #16990 ) ) ;
#17502 = ORIENTED_EDGE ( 'NONE', *, *, #19488, .F. ) ;
#17503 = FACE_OUTER_BOUND ( 'NONE', #15178, .T. ) ;
#17504 = CIRCLE ( 'NONE', #23752, 1.499999999999994449 ) ;
#17505 = CARTESIAN_POINT ( 'NONE',  ( -44.30175744945091054, -5.935454207752202116, 53.91104711115070813 ) ) ;
#17506 = DIRECTION ( 'NONE',  ( 0.000000000000000000, 1.000000000000000000, -0.000000000000000000 ) ) ;
#17507 = CARTESIAN_POINT ( 'NONE',  ( 21.09785597605720753, 14.86454579224779948, 47.04930799450052348 ) ) ;
#17508 = CARTESIAN_POINT ( 'NONE',  ( 48.23388214087538017, 25.42822093266651606, 49.27628903457465270 ) ) ;
#17509 = ORIENTED_EDGE ( 'NONE', *, *, #4945, .T. ) ;
#17510 = FACE_OUTER_BOUND ( 'NONE', #20316, .T. ) ;
#17511 = ORIENTED_EDGE ( 'NONE', *, *, #3804, .F. ) ;
#17512 = CARTESIAN_POINT ( 'NONE',  ( -33.48165330108982118, -1.516555287492495463, 13.41764155437908457 ) ) ;
#17513 = CARTESIAN_POINT ( 'NONE',  ( 33.46699938050304013, 38.56284415653841791, 47.04930799450051637 ) ) ;
#17514 = ORIENTED_EDGE ( 'NONE', *, *, #1851, .F. ) ;
#17515 = DIRECTION ( 'NONE',  ( 0.000000000000000000, 0.000000000000000000, -1.000000000000000000 ) ) ;
#17516 = DIRECTION ( 'NONE',  ( -0.8746197071393805311, 0.4848096202463645921, 8.676864087101954631E-18 ) ) ;
#17517 = DIRECTION ( 'NONE',  ( -0.000000000000000000, -1.000000000000000000, -0.000000000000000000 ) ) ;
#17518 = DIRECTION ( 'NONE',  ( -1.101824276508909887E-16, 1.000000000000000000, -0.000000000000000000 ) ) ;
#17519 = DIRECTION ( 'NONE',  ( -1.101824276508909887E-16, 1.000000000000000000, -0.000000000000000000 ) ) ;
#17520 = CARTESIAN_POINT ( 'NONE',  ( 46.00908685603034343, 27.54624452788248590, 44.91496614357595263 ) ) ;
#17521 = CARTESIAN_POINT ( 'NONE',  ( -40.02540636251514172, 2.839176264122877047, 55.84930799450052064 ) ) ;
#17522 = DIRECTION ( 'NONE',  ( 0.8746197071393926326, -0.4848096202463430537, -8.676864087101709653E-18 ) ) ;
#17523 = EDGE_LOOP ( 'NONE', ( #16787, #10151, #3790, #14140 ) ) ;
#17524 = CARTESIAN_POINT ( 'NONE',  ( 8.698509210239588896, 32.59164230456639899, 47.04930799450051637 ) ) ;
#17525 = DIRECTION ( 'NONE',  ( -1.101824276508909887E-16, 1.000000000000000000, -0.000000000000000000 ) ) ;
#17526 = ORIENTED_EDGE ( 'NONE', *, *, #17533, .F. ) ;
#17527 = CARTESIAN_POINT ( 'NONE',  ( 47.63716429968715005, 28.31960992152947298, 49.58068632438585155 ) ) ;
#17528 = ORIENTED_EDGE ( 'NONE', *, *, #9078, .T. ) ;
#17529 = VECTOR ( 'NONE', #31557, 1000.000000000000114 ) ;
#17530 = ORIENTED_EDGE ( 'NONE', *, *, #16284, .F. ) ;
#17531 = CARTESIAN_POINT ( 'NONE',  ( -40.59758774925371938, 7.567737757495683226, 38.19144330556764544 ) ) ;
#17532 = TOROIDAL_SURFACE ( 'NONE', #6003, 12.61792373059894246, 0.1249999999999989730 ) ;
#17533 = EDGE_CURVE ( 'NONE', #26331, #7154, #1225, .T. ) ;
#17534 = VECTOR ( 'NONE', #15122, 1000.000000000000114 ) ;
#17535 = ORIENTED_EDGE ( 'NONE', *, *, #16887, .T. ) ;
#17536 = B_SPLINE_CURVE_WITH_KNOTS ( 'NONE', 3,
 ( #2508, #32386, #32230, #19734, #27464, #14994, #10072, #20069, #15151, #25160 ),
 .UNSPECIFIED., .F., .F.,
 ( 4, 2, 2, 2, 4 ),
 ( 0.0006731324393514880305, 0.002417216000136414994, 0.004161299560921341741, 0.005905383121706269355, 0.007649466682491196101 ),
 .UNSPECIFIED. ) ;
#17537 = EDGE_LOOP ( 'NONE', ( #19166, #9176, #4361, #18165 ) ) ;
#17538 = CARTESIAN_POINT ( 'NONE',  ( 46.17891025898683921, 22.93807716476589675, 48.46582155994513386 ) ) ;
#17539 = EDGE_LOOP ( 'NONE', ( #14115, #32438, #1608, #23758 ) ) ;
#17540 = CIRCLE ( 'NONE', #24352, 0.1000000000000018235 ) ;
#17541 = CYLINDRICAL_SURFACE ( 'NONE', #25124, 27.49999999999999289 ) ;
#17542 = DIRECTION ( 'NONE',  ( -1.101824276508909887E-16, 1.000000000000000000, -0.000000000000000000 ) ) ;
#17543 = CARTESIAN_POINT ( 'NONE',  ( 21.09785597605720042, -14.04221034894631615, 47.04930799450051637 ) ) ;
#17544 = PRODUCT_DEFINITION ( 'UNKNOWN', '', #11884, #3557 ) ;
#17545 = AXIS2_PLACEMENT_3D ( 'NONE', #22676, #24653, #2815 ) ;
#17546 = CARTESIAN_POINT ( 'NONE',  ( 46.99023568444673060, 25.73791119454915588, 49.12151524109405898 ) ) ;
#17547 = EDGE_LOOP ( 'NONE', ( #14387, #29489, #5788, #11006 ) ) ;
#17548 = ORIENTED_EDGE ( 'NONE', *, *, #9944, .F. ) ;
#17550 = DIRECTION ( 'NONE',  ( -1.000000000000000000, 0.000000000000000000, 2.775557561562888984E-15 ) ) ;
#17549 = CIRCLE ( 'NONE', #30147, 27.99999999999999645 ) ;
#17551 = CIRCLE ( 'NONE', #10752, 20.13652856819611969 ) ;
#17552 = ORIENTED_EDGE ( 'NONE', *, *, #8614, .F. ) ;
#17553 = CARTESIAN_POINT ( 'NONE',  ( -41.94956971822180947, 3.905757428664830222, 49.04930799450051637 ) ) ;
#17554 = DIRECTION ( 'NONE',  ( 1.000000000000000000, 0.000000000000000000, -1.224646799147353207E-16 ) ) ;
#17555 = CARTESIAN_POINT ( 'NONE',  ( 21.09785597605720753, 14.86454579224779948, 47.04930799450052348 ) ) ;
#17556 = DIRECTION ( 'NONE',  ( -0.000000000000000000, -1.000000000000000000, 0.000000000000000000 ) ) ;
#17557 = ITEM_DEFINED_TRANSFORMATION ( 'NONE', 'NONE', #29670,  #8172 ) ;
#17558 = ORIENTED_EDGE ( 'NONE', *, *, #7379, .F. ) ;
#17559 = ORIENTED_EDGE ( 'NONE', *, *, #32405, .T. ) ;
#17560 = CARTESIAN_POINT ( 'NONE',  ( 45.00053793792376666, 28.75920399681022488, 45.68869892245983522 ) ) ;
#17561 = CARTESIAN_POINT ( 'NONE',  ( -63.90214402394282445, -5.935454207752205669, 40.04930799450050216 ) ) ;
#17562 = ORIENTED_EDGE ( 'NONE', *, *, #16699, .T. ) ;
#17563 = CARTESIAN_POINT ( 'NONE',  ( 52.09557426805990588, -5.936215030417558935, 107.4832098830738829 ) ) ;
#17564 = VERTEX_POINT ( 'NONE', #18098 ) ;
#17565 = DIRECTION ( 'NONE',  ( -1.000000000000000000, 0.000000000000000000, 0.000000000000000000 ) ) ;
#17566 = CARTESIAN_POINT ( 'NONE',  ( 21.09785597605720042, -13.68834655544033652, 47.04930799450051637 ) ) ;
#17567 = DIRECTION ( 'NONE',  ( 0.7141240004913198547, -0.3958453973320100738, 0.5773502691896283956 ) ) ;
#17568 = EDGE_CURVE ( 'NONE', #21227, #13584, #26404, .T. ) ;
#17569 = CIRCLE ( 'NONE', #6558, 1.499999999999997780 ) ;
#17570 = EDGE_CURVE ( 'NONE', #8138, #21967, #12259, .T. ) ;
#17571 = EDGE_CURVE ( 'NONE', #19822, #9936, #20646, .T. ) ;
#17572 = TOROIDAL_SURFACE ( 'NONE', #12810, 1.299999999999999822, 0.1000000000000000056 ) ;
#17573 = EDGE_CURVE ( 'NONE', #14283, #593, #5441, .T. ) ;
#17574 = AXIS2_PLACEMENT_3D ( 'NONE', #10939, #26346, #5862 ) ;
#17575 = AXIS2_PLACEMENT_3D ( 'NONE', #20739, #237, #20580 ) ;
#17576 = AXIS2_PLACEMENT_3D ( 'NONE', #13878, #26993, #21397 ) ;
#17577 = ORIENTED_EDGE ( 'NONE', *, *, #20572, .F. ) ;
#17578 = ORIENTED_EDGE ( 'NONE', *, *, #12133, .T. ) ;
#17579 = CARTESIAN_POINT ( 'NONE',  ( 46.99023568444673060, 27.22451373492759785, 49.12151524109405898 ) ) ;
#17580 = ORIENTED_EDGE ( 'NONE', *, *, #20490, .T. ) ;
#17581 = FACE_OUTER_BOUND ( 'NONE', #32032, .T. ) ;
#17582 = CARTESIAN_POINT ( 'NONE',  ( -42.50976151518963064, 14.59907569580870046, 38.09144330556765112 ) ) ;
#17583 = CARTESIAN_POINT ( 'NONE',  ( 8.698509210239571132, 30.84164230456639544, 47.04930799450051637 ) ) ;
#17584 = DIRECTION ( 'NONE',  ( -1.000000000000000000, 0.000000000000000000, 0.000000000000000000 ) ) ;
#17585 = CARTESIAN_POINT ( 'NONE',  ( 44.87087493598345134, 27.47587066347689344, 48.18533415931919706 ) ) ;
#17586 = LINE ( 'NONE', #22504, #23839 ) ;
#17587 = FACE_OUTER_BOUND ( 'NONE', #29291, .T. ) ;
#17588 = CARTESIAN_POINT ( 'NONE',  ( 21.09785597605719332, 30.56454579224779522, 47.04930799450051637 ) ) ;
#17589 = DIRECTION ( 'NONE',  ( 0.000000000000000000, 1.000000000000000000, -0.000000000000000000 ) ) ;
#17590 = CARTESIAN_POINT ( 'NONE',  ( -40.21210701746133509, 7.644196001419694575, 53.54930799450051637 ) ) ;
#17591 =( NAMED_UNIT ( * ) SI_UNIT ( $, .STERADIAN. ) SOLID_ANGLE_UNIT ( ) );
#17592 = ORIENTED_EDGE ( 'NONE', *, *, #27757, .T. ) ;
#17593 = ORIENTED_EDGE ( 'NONE', *, *, #14761, .T. ) ;
#17594 = ADVANCED_FACE ( 'NONE', ( #23511 ), #21193, .T. ) ;
#17595 = DIRECTION ( 'NONE',  ( 0.000000000000000000, 0.000000000000000000, -1.000000000000000000 ) ) ;
#17596 = AXIS2_PLACEMENT_3D ( 'NONE', #21363, #31728, #11707 ) ;
#17597 = EDGE_CURVE ( 'NONE', #4270, #27697, #19582, .T. ) ;
#17598 = VECTOR ( 'NONE', #27975, 1000.000000000000000 ) ;
#17599 = CARTESIAN_POINT ( 'NONE',  ( 49.13615439483240976, 25.02317097547241076, 45.53350292621570361 ) ) ;
#17600 = CARTESIAN_POINT ( 'NONE',  ( -32.01200205328026982, -0.4574755010172156799, 13.68185562056011406 ) ) ;
#17601 = CARTESIAN_POINT ( 'NONE',  ( 54.82962069436126029, -2.844921901652548879, 101.4917363106557247 ) ) ;
#17602 = ORIENTED_EDGE ( 'NONE', *, *, #9764, .T. ) ;
#17603 = DIRECTION ( 'NONE',  ( 1.344306794811909313E-16, -1.000000000000000000, -1.759793992609926301E-18 ) ) ;
#17604 = PLANE ( 'NONE',  #22088 ) ;
#17605 = LINE ( 'NONE', #7110, #23581 ) ;
#17606 = ORIENTED_EDGE ( 'NONE', *, *, #23307, .T. ) ;
#17607 = VERTEX_POINT ( 'NONE', #13353 ) ;
#17608 = CARTESIAN_POINT ( 'NONE',  ( 21.09785597605720753, 14.81645899701909563, 47.04930799450052348 ) ) ;
#17609 = CARTESIAN_POINT ( 'NONE',  ( 46.00908685603034343, 26.23284706826093071, 44.91496614357595263 ) ) ;
#17610 = CARTESIAN_POINT ( 'NONE',  ( 21.09992658989238734, 32.59164230456639899, 47.04930799450051637 ) ) ;
#17611 = VECTOR ( 'NONE', #13957, 1000.000000000000000 ) ;
#17612 = DIRECTION ( 'NONE',  ( -1.101824276508909887E-16, 1.000000000000000000, -0.000000000000000000 ) ) ;
#17613 = LINE ( 'NONE', #27629, #17103 ) ;
#17614 = EDGE_CURVE ( 'NONE', #25964, #13560, #26132, .T. ) ;
#17615 = ORIENTED_EDGE ( 'NONE', *, *, #13439, .T. ) ;
#17616 = AXIS2_PLACEMENT_3D ( 'NONE', #2142, #10024, #27416 ) ;
#17617 = EDGE_LOOP ( 'NONE', ( #5700, #2764, #15638, #17823 ) ) ;
#17618 = EDGE_CURVE ( 'NONE', #12345, #14664, #2298, .T. ) ;
#17619 = CARTESIAN_POINT ( 'NONE',  ( -39.64148344771002286, 7.657122216028890982, 32.04930799450052348 ) ) ;
#17620 = CARTESIAN_POINT ( 'NONE',  ( 21.09992658989238734, 38.56284415653841791, 47.04930799450051637 ) ) ;
#17621 = EDGE_CURVE ( 'NONE', #27142, #27524, #3645, .T. ) ;
#17622 = AXIS2_PLACEMENT_3D ( 'NONE', #4997, #2525, #12551 ) ;
#17623 = ORIENTED_EDGE ( 'NONE', *, *, #5126, .T. ) ;
#17624 = DIRECTION ( 'NONE',  ( -1.101824276508909887E-16, 1.000000000000000000, -0.000000000000000000 ) ) ;
#17625 = ORIENTED_EDGE ( 'NONE', *, *, #14535, .T. ) ;
#17626 = CARTESIAN_POINT ( 'NONE',  ( 79.93903702853120308, -5.822320178461996676, 78.65606980742406051 ) ) ;
#17627 = DIRECTION ( 'NONE',  ( -1.101824276508909887E-16, 1.000000000000000000, -0.000000000000000000 ) ) ;
#17628 = DIRECTION ( 'NONE',  ( -0.8746197071393858602, 0.4848096202463547666, 0.000000000000000000 ) ) ;
#17629 = CARTESIAN_POINT ( 'NONE',  ( 21.09992658989238734, 38.56284415653841791, 47.04930799450051637 ) ) ;
#17630 = ORIENTED_EDGE ( 'NONE', *, *, #22036, .F. ) ;
#17631 = ADVANCED_FACE ( 'NONE', ( #27961 ), #5479, .F. ) ;
#17632 = CARTESIAN_POINT ( 'NONE',  ( 33.37634396954521776, 29.59164230456639899, 47.04930799450051637 ) ) ;
#17633 = DIRECTION ( 'NONE',  ( -1.000000000000000000, 0.000000000000000000, 0.000000000000000000 ) ) ;
#17634 = EDGE_CURVE ( 'NONE', #13719, #24589, #30470, .T. ) ;
#17635 = CARTESIAN_POINT ( 'NONE',  ( 81.68227850725321559, -5.935454207752203004, 77.87546120947916961 ) ) ;
#17636 = DIRECTION ( 'NONE',  ( -0.1949050434465251780, 0.6797146636928671493, -0.7071067811865480168 ) ) ;
#17637 = FACE_OUTER_BOUND ( 'NONE', #21971, .T. ) ;
#17638 = ORIENTED_EDGE ( 'NONE', *, *, #27993, .F. ) ;
#17639 = DIRECTION ( 'NONE',  ( -1.000000000000000000, 0.000000000000000000, 0.000000000000000000 ) ) ;
#17640 = DIRECTION ( 'NONE',  ( 0.000000000000000000, 0.000000000000000000, 1.000000000000000000 ) ) ;
#17641 = ORIENTED_EDGE ( 'NONE', *, *, #9635, .F. ) ;
#17642 = DIRECTION ( 'NONE',  ( 0.1949050434465268156, -0.6797146636928667052, 0.7071067811865480168 ) ) ;
#17643 = DIRECTION ( 'NONE',  ( 0.2756373558169974980, -0.9612616959383193382, -1.315048337272770589E-17 ) ) ;
#17644 = AXIS2_PLACEMENT_3D ( 'NONE', #5256, #165, #10186 ) ;
#17645 = CARTESIAN_POINT ( 'NONE',  ( 33.50134396954519644, 31.09164230456639544, 47.04930799450051637 ) ) ;
#17646 = ORIENTED_EDGE ( 'NONE', *, *, #14856, .F. ) ;
#17647 = DIRECTION ( 'NONE',  ( -0.000000000000000000, 1.000000000000000000, -0.000000000000000000 ) ) ;
#17648 = ORIENTED_EDGE ( 'NONE', *, *, #20844, .T. ) ;
#17649 = EDGE_CURVE ( 'NONE', #10403, #25889, #11050, .T. ) ;
#17650 = CIRCLE ( 'NONE', #5073, 28.00000000000000000 ) ;
#17651 = EDGE_LOOP ( 'NONE', ( #27430, #103, #15401, #17511 ) ) ;
#17652 = EDGE_CURVE ( 'NONE', #32242, #29171, #14444, .T. ) ;
#17653 = CARTESIAN_POINT ( 'NONE',  ( -40.36282785745800794, 8.169822035811970196, 57.04930799450051637 ) ) ;
#17654 = CARTESIAN_POINT ( 'NONE',  ( 44.21498992391908445, 25.89488759933319173, 46.89958605635244027 ) ) ;
#17655 = VECTOR ( 'NONE', #24173, 999.9999999999998863 ) ;
#17656 = EDGE_CURVE ( 'NONE', #14836, #21481, #17049, .T. ) ;
#17657 = ORIENTED_EDGE ( 'NONE', *, *, #18558, .F. ) ;
#17658 = VERTEX_POINT ( 'NONE', #6110 ) ;
#17659 = CARTESIAN_POINT ( 'NONE',  ( -44.15922173408817031, -5.483165097835474455, 52.77548294416367725 ) ) ;
#17660 = DIRECTION ( 'NONE',  ( 0.000000000000000000, 0.000000000000000000, 1.000000000000000000 ) ) ;
#17661 = DIRECTION ( 'NONE',  ( -1.000000000000000000, -1.101824276508909887E-16, 0.000000000000000000 ) ) ;
#17662 = CARTESIAN_POINT ( 'NONE',  ( 21.09785597605719332, 25.56454579224779167, 47.04930799450051637 ) ) ;
#17663 = VERTEX_POINT ( 'NONE', #23021 ) ;
#17664 = CARTESIAN_POINT ( 'NONE',  ( 5.864109918520784781, 14.46497581658974063, 47.04930799450052348 ) ) ;
#17665 = VERTEX_POINT ( 'NONE', #540 ) ;
#17666 = CARTESIAN_POINT ( 'NONE',  ( -32.37019670470567689, 0.9468387599394830767, 14.21691100150221132 ) ) ;
#17667 = CARTESIAN_POINT ( 'NONE',  ( -25.30045392157957096, 13.78442380691147839, 47.04930799450052348 ) ) ;
#17668 = EDGE_CURVE ( 'NONE', #22338, #5664, #9189, .T. ) ;
#17669 = ORIENTED_EDGE ( 'NONE', *, *, #221, .T. ) ;
#17670 = DIRECTION ( 'NONE',  ( -1.101824276508909887E-16, 1.000000000000000000, -0.000000000000000000 ) ) ;
#17671 = DIRECTION ( 'NONE',  ( -0.9612616959383221138, -0.2756373558169876170, 0.000000000000000000 ) ) ;
#17672 = CARTESIAN_POINT ( 'NONE',  ( 21.09785597605720042, -14.54791319078308653, 47.04930799450051637 ) ) ;
#17673 = CARTESIAN_POINT ( 'NONE',  ( -40.21091586930921125, 6.838981405724006812, 39.54930799450052348 ) ) ;
#17674 = DIRECTION ( 'NONE',  ( -1.101824276508909887E-16, 1.000000000000000000, -0.000000000000000000 ) ) ;
#17675 = EDGE_CURVE ( 'NONE', #22149, #10005, #18613, .T. ) ;
#17676 = CARTESIAN_POINT ( 'NONE',  ( 49.49063479933183629, 27.31291119454915517, 47.17357720316391578 ) ) ;
#17677 = CARTESIAN_POINT ( 'NONE',  ( 21.09785597605720753, 16.03967147762300982, 47.04930799450052348 ) ) ;
#17678 = CARTESIAN_POINT ( 'NONE',  ( 21.09992658989238734, 32.54735957529758394, 47.04930799450051637 ) ) ;
#17679 = VERTEX_POINT ( 'NONE', #30593 ) ;
#17680 = LINE ( 'NONE', #27699, #30303 ) ;
#17681 = ORIENTED_EDGE ( 'NONE', *, *, #13798, .F. ) ;
#17682 = AXIS2_PLACEMENT_3D ( 'NONE', #994, #25939, #3454 ) ;
#17683 = CARTESIAN_POINT ( 'NONE',  ( 44.21498992391908445, 28.11753733014355916, 46.89958605635242606 ) ) ;
#17684 = ORIENTED_EDGE ( 'NONE', *, *, #2806, .F. ) ;
#17685 = AXIS2_PLACEMENT_3D ( 'NONE', #29079, #26293, #29408 ) ;
#17686 = VERTEX_POINT ( 'NONE', #14365 ) ;
#17687 = FACE_OUTER_BOUND ( 'NONE', #8419, .T. ) ;
#17688 = VECTOR ( 'NONE', #22694, 1000.000000000000000 ) ;
#17689 = ORIENTED_EDGE ( 'NONE', *, *, #12171, .F. ) ;
#17690 = AXIS2_PLACEMENT_3D ( 'NONE', #14176, #24170, #4807 ) ;
#17691 = VECTOR ( 'NONE', #25014, 1000.000000000000000 ) ;
#17692 = VERTEX_POINT ( 'NONE', #6646 ) ;
#17693 = ADVANCED_FACE ( 'NONE', ( #29463, #26828 ), #24361, .T. ) ;
#17694 = CARTESIAN_POINT ( 'NONE',  ( 45.39590889550878927, 22.93328494799376571, 47.28470721838063184 ) ) ;
#17695 = EDGE_LOOP ( 'NONE', ( #16038, #8330, #932, #26025 ) ) ;
#17696 = PRESENTATION_STYLE_ASSIGNMENT (( #2772 ) ) ;
#17697 = CARTESIAN_POINT ( 'NONE',  ( 33.46699938050304013, 24.72145308207319303, 47.04930799450050927 ) ) ;
#17698 = DIRECTION ( 'NONE',  ( -1.000000000000000000, 0.000000000000000000, 0.000000000000000000 ) ) ;
#17699 = CARTESIAN_POINT ( 'NONE',  ( 47.20547626766766314, 26.08791119454915730, 44.97710074790751378 ) ) ;
#17700 = ORIENTED_EDGE ( 'NONE', *, *, #30428, .F. ) ;
#17701 = AXIS2_PLACEMENT_3D ( 'NONE', #26565, #29035, #6386 ) ;
#17702 = ORIENTED_EDGE ( 'NONE', *, *, #21702, .F. ) ;
#17703 = CARTESIAN_POINT ( 'NONE',  ( 8.732853799281738105, 28.71183152705961206, 47.04930799450051637 ) ) ;
#17704 = AXIS2_PLACEMENT_3D ( 'NONE', #2239, #12423, #102 ) ;
#17705 = EDGE_CURVE ( 'NONE', #17230, #12393, #12339, .T. ) ;
#17706 = ORIENTED_EDGE ( 'NONE', *, *, #15474, .T. ) ;
#17707 = CARTESIAN_POINT ( 'NONE',  ( 33.50134396954519644, 31.34164230456639544, 47.04930799450051637 ) ) ;
#17708 = CARTESIAN_POINT ( 'NONE',  ( 21.09785597605720042, -13.64309448858209528, -11.84046438077000118 ) ) ;
#17709 = ADVANCED_FACE ( 'NONE', ( #22057 ), #24522, .F. ) ;
#17710 = CIRCLE ( 'NONE', #3560, 0.1000000000000028644 ) ;
#17711 = DIRECTION ( 'NONE',  ( -0.2756373558169946114, 0.9612616959383201154, 2.956675082362952627E-15 ) ) ;
#17712 = DIRECTION ( 'NONE',  ( 0.000000000000000000, 0.000000000000000000, -1.000000000000000000 ) ) ;
#17713 = ITEM_DEFINED_TRANSFORMATION ( 'NONE', 'NONE', #21268,  #8172 ) ;
#17714 = EDGE_LOOP ( 'NONE', ( #29822, #18099, #17854, #21248, #12878 ) ) ;
#17715 = EDGE_LOOP ( 'NONE', ( #13809, #1058, #15617, #26428 ) ) ;
#17716 = DIRECTION ( 'NONE',  ( -0.000000000000000000, -1.000000000000000000, 0.000000000000000000 ) ) ;
#17717 = LINE ( 'NONE', #8051, #9896 ) ;
#17718 = AXIS2_PLACEMENT_3D ( 'NONE', #4132, #11855, #14157 ) ;
#17719 = CARTESIAN_POINT ( 'NONE',  ( 21.09785597605720753, 13.86454579224779948, 47.04930799450052348 ) ) ;
#17720 = EDGE_LOOP ( 'NONE', ( #30262, #21128 ) ) ;
#17721 = CARTESIAN_POINT ( 'NONE',  ( 48.94625023931840246, 28.15784706826092787, 46.10640627770149536 ) ) ;
#17722 = ORIENTED_EDGE ( 'NONE', *, *, #8573, .F. ) ;
#17723 = DIRECTION ( 'NONE',  ( -1.000000000000000000, 0.000000000000000000, 0.000000000000000000 ) ) ;
#17724 = LINE ( 'NONE', #10689, #30335 ) ;
#17725 = CARTESIAN_POINT ( 'NONE',  ( 46.09785597605720397, 14.86454579224779948, 47.04930799450052348 ) ) ;
#17726 = CIRCLE ( 'NONE', #2528, 0.1250000000000001110 ) ;
#17727 = AXIS2_PLACEMENT_3D ( 'NONE', #8704, #5925, #18694 ) ;
#17728 = AXIS2_PLACEMENT_3D ( 'NONE', #28395, #23306, #31505 ) ;
#17729 = ORIENTED_EDGE ( 'NONE', *, *, #4782, .T. ) ;
#17730 = TOROIDAL_SURFACE ( 'NONE', #16133, 38.50000000000000000, 1.499999999999997780 ) ;
#17731 = TOROIDAL_SURFACE ( 'NONE', #14604, 12.40141737965287838, 0.1249999999999998335 ) ;
#17732 = VERTEX_POINT ( 'NONE', #32085 ) ;
#17733 = DIRECTION ( 'NONE',  ( -0.8746197071393858602, 0.4848096202463547666, 0.000000000000000000 ) ) ;
#17734 = DIRECTION ( 'NONE',  ( -1.101824276508909887E-16, 1.000000000000000000, -0.000000000000000000 ) ) ;
#17735 = CARTESIAN_POINT ( 'NONE',  ( 45.79384627280941089, 25.06618040159426641, 49.05938063676249072 ) ) ;
#17736 = AXIS2_PLACEMENT_3D ( 'NONE', #7758, #28265, #23007 ) ;
#17737 = ORIENTED_EDGE ( 'NONE', *, *, #24979, .F. ) ;
#17738 = CARTESIAN_POINT ( 'NONE',  ( -38.65545646816406133, -5.935454207752198563, 77.87546120947918382 ) ) ;
#17739 = CARTESIAN_POINT ( 'NONE',  ( 21.09785597605719332, 7.881678200673685630, 47.04930799450051637 ) ) ;
#17740 = DIRECTION ( 'NONE',  ( 0.4544104193609900810, 0.000000000000000000, 0.8907924397839089847 ) ) ;
#17741 = CARTESIAN_POINT ( 'NONE',  ( 46.96819297411687444, 26.19253733014356200, 49.54594323136014822 ) ) ;
#17742 = ADVANCED_FACE ( 'NONE', ( #14205 ), #12889, .T. ) ;
#17743 = FACE_OUTER_BOUND ( 'NONE', #32397, .T. ) ;
#17744 = CARTESIAN_POINT ( 'NONE',  ( -43.90780810587784089, -0.03953120679776488122, 61.94930799450052206 ) ) ;
#17745 = DIRECTION ( 'NONE',  ( -0.9612616959383194493, -0.2756373558169974980, -8.795445018804946186E-19 ) ) ;
#17746 = ADVANCED_FACE ( 'NONE', ( #4348 ), #7135, .T. ) ;
#17747 = CARTESIAN_POINT ( 'NONE',  ( 45.38329851326696485, 22.91413368675619111, 47.60724751575505564 ) ) ;
#17749 = EDGE_CURVE ( 'NONE', #6225, #11078, #8146, .T. ) ;
#17748 = FACE_OUTER_BOUND ( 'NONE', #3022, .T. ) ;
#17750 = EDGE_CURVE ( 'NONE', #8773, #1340, #29106, .T. ) ;
#17751 = EDGE_CURVE ( 'NONE', #25197, #5223, #3967, .T. ) ;
#17752 = CARTESIAN_POINT ( 'NONE',  ( 45.32239087082389517, 11.18855628041951711, 97.83690911057082928 ) ) ;
#17753 = CARTESIAN_POINT ( 'NONE',  ( 45.73035263060504718, 29.33954579807170404, 44.36855633853329550 ) ) ;
#17754 = ORIENTED_EDGE ( 'NONE', *, *, #19375, .F. ) ;
#17755 = ORIENTED_EDGE ( 'NONE', *, *, #6594, .F. ) ;
#17756 = CARTESIAN_POINT ( 'NONE',  ( 8.482002859293444885, 28.71664230456639899, 47.04930799450051637 ) ) ;
#17757 = CIRCLE ( 'NONE', #24056, 4.100000000000001421 ) ;
#17758 = CARTESIAN_POINT ( 'NONE',  ( 49.31977745283734293, 25.00299017030662441, 45.79416704315556075 ) ) ;
#17759 = CARTESIAN_POINT ( 'NONE',  ( 33.71785032049135822, 26.46664230456639899, 47.04930799450051637 ) ) ;
#17760 = CIRCLE ( 'NONE', #3077, 55.69429210806286079 ) ;
#17761 = VECTOR ( 'NONE', #21172, 1000.000000000000000 ) ;
#17762 = LINE ( 'NONE', #18081, #22464 ) ;
#17763 = ORIENTED_EDGE ( 'NONE', *, *, #714, .F. ) ;
#17764 = CARTESIAN_POINT ( 'NONE',  ( -42.38687957179149635, 4.148162238788000167, 38.24930799450051921 ) ) ;
#17765 = CARTESIAN_POINT ( 'NONE',  ( -40.50726676055796105, 7.559560307024983494, 60.24930799450051211 ) ) ;
#17766 = CARTESIAN_POINT ( 'NONE',  ( 8.474859994195281132, 38.56284415653841791, 47.04930799450051637 ) ) ;
#17767 = VERTEX_POINT ( 'NONE', #31920 ) ;
#17768 = ORIENTED_EDGE ( 'NONE', *, *, #7462, .T. ) ;
#17769 = DIRECTION ( 'NONE',  ( -0.000000000000000000, -1.000000000000000000, -0.000000000000000000 ) ) ;
#17770 = CARTESIAN_POINT ( 'NONE',  ( 48.94625023931840246, 28.15784706826092787, 46.10640627770150246 ) ) ;
#17771 = CARTESIAN_POINT ( 'NONE',  ( -10.96598430569368432, -5.983766253076982622, -3.351769630585352377 ) ) ;
#17772 = CIRCLE ( 'NONE', #1017, 0.1999999999999987899 ) ;
#17773 = CARTESIAN_POINT ( 'NONE',  ( -42.66751614955961003, 15.14923148629343785, 38.44930799450052916 ) ) ;
#17774 = DIRECTION ( 'NONE',  ( -1.101824276508909887E-16, 1.000000000000000000, -0.000000000000000000 ) ) ;
#17775 = ORIENTED_EDGE ( 'NONE', *, *, #13391, .F. ) ;
#17776 = ADVANCED_FACE ( 'NONE', ( #16967 ), #16810, .T. ) ;
#17777 = AXIS2_PLACEMENT_3D ( 'NONE', #19629, #19958, #29825 ) ;
#17778 = TOROIDAL_SURFACE ( 'NONE', #25140, 12.61792373059861028, 0.1250000000000006106 ) ;
#17779 = EDGE_LOOP ( 'NONE', ( #11218, #14037, #14801, #15964, #21685, #1167 ) ) ;
#17780 = CARTESIAN_POINT ( 'NONE',  ( 21.09785597605719332, -15.93545420775219945, -29.66074251183834676 ) ) ;
#17781 = DIRECTION ( 'NONE',  ( -0.000000000000000000, -1.000000000000000000, -0.000000000000000000 ) ) ;
#17782 = EDGE_LOOP ( 'NONE', ( #1430, #9958, #20399, #18028 ) ) ;
#17783 = TOROIDAL_SURFACE ( 'NONE', #9922, 12.40141737965288726, 0.1250000000000003331 ) ;
#17784 = DIRECTION ( 'NONE',  ( -1.000000000000000000, 0.000000000000000000, 0.000000000000000000 ) ) ;
#17785 = ORIENTED_EDGE ( 'NONE', *, *, #594, .F. ) ;
#17786 = EDGE_CURVE ( 'NONE', #21045, #16795, #8680, .T. ) ;
#17787 = DIRECTION ( 'NONE',  ( -1.101824276508909887E-16, 1.000000000000000000, -0.000000000000000000 ) ) ;
#17788 = CARTESIAN_POINT ( 'NONE',  ( -4.902144023942810236, 25.56454579224779167, 49.54930799450042400 ) ) ;
#17789 = ADVANCED_FACE ( 'NONE', ( #18937 ), #12750, .F. ) ;
#17790 = CIRCLE ( 'NONE', #15713, 31.50000000000000711 ) ;
#17791 = CARTESIAN_POINT ( 'NONE',  ( 47.09785597605719687, 25.16454579224780019, 47.04930799450078638 ) ) ;
#17792 = EDGE_CURVE ( 'NONE', #32191, #11333, #19128, .T. ) ;
#17793 = CARTESIAN_POINT ( 'NONE',  ( -40.69454725800886763, 6.788012290873795429, 39.45785194957959874 ) ) ;
#17794 = EDGE_LOOP ( 'NONE', ( #8593, #26005, #29785, #15589 ) ) ;
#17795 = DIRECTION ( 'NONE',  ( -1.000000000000000000, 0.000000000000000000, 0.000000000000000000 ) ) ;
#17796 = DIRECTION ( 'NONE',  ( 1.000000000000000000, 0.000000000000000000, 0.000000000000000000 ) ) ;
#17797 = CARTESIAN_POINT ( 'NONE',  ( 81.58134094568082162, -5.936631694656539615, 77.91225944795358771 ) ) ;
#17798 = LINE ( 'NONE', #7643, #16113 ) ;
#17799 = DIRECTION ( 'NONE',  ( -0.8746197071393790878, 0.4848096202463673676, 1.277302113040196197E-17 ) ) ;
#17800 = VERTEX_POINT ( 'NONE', #31599 ) ;
#17801 = CARTESIAN_POINT ( 'NONE',  ( 33.72499318558949710, 24.34143805560860940, 47.04930799450051637 ) ) ;
#17802 = CARTESIAN_POINT ( 'NONE',  ( 21.09785597605719332, -8.874820941924726370, -20.33845821050190494 ) ) ;
#17803 = ORIENTED_EDGE ( 'NONE', *, *, #9238, .T. ) ;
#17804 = CYLINDRICAL_SURFACE ( 'NONE', #29348, 0.1000000000000008243 ) ;
#17805 = CARTESIAN_POINT ( 'NONE',  ( 21.09785597605719332, -15.93545420775219945, 47.04930799450051637 ) ) ;
#17806 = CIRCLE ( 'NONE', #15205, 2.000000000000001776 ) ;
#17807 = TOROIDAL_SURFACE ( 'NONE', #3646, 12.40141737965286062, 0.1249999999999998196 ) ;
#17808 = DIRECTION ( 'NONE',  ( -1.224646799147353207E-16, -1.349345573449484691E-32, 1.000000000000000000 ) ) ;
#17809 = ORIENTED_EDGE ( 'NONE', *, *, #27201, .F. ) ;
#17810 = CARTESIAN_POINT ( 'NONE',  ( 21.09992658989239089, 29.22145308207318237, 47.04930799450051637 ) ) ;
#17811 = ORIENTED_EDGE ( 'NONE', *, *, #16661, .F. ) ;
#17812 = AXIS2_PLACEMENT_3D ( 'NONE', #1367, #11383, #21868 ) ;
#17813 = AXIS2_PLACEMENT_3D ( 'NONE', #18448, #21067, #23703 ) ;
#17814 = ORIENTED_EDGE ( 'NONE', *, *, #2395, .T. ) ;
#17815 = AXIS2_PLACEMENT_3D ( 'NONE', #5609, #511, #10549 ) ;
#17816 = AXIS2_PLACEMENT_3D ( 'NONE', #26485, #21710, #11232 ) ;
#17817 = EDGE_CURVE ( 'NONE', #28526, #7845, #21235, .T. ) ;
#17818 = EDGE_CURVE ( 'NONE', #15519, #29185, #3941, .T. ) ;
#17819 = DIRECTION ( 'NONE',  ( -0.1949050434465252335, 0.6797146636928682595, 0.7071067811865469066 ) ) ;
#17820 = CARTESIAN_POINT ( 'NONE',  ( 48.83059987400640978, 26.85948166895303402, 48.97189179988552610 ) ) ;
#17821 = AXIS2_PLACEMENT_3D ( 'NONE', #3656, #24164, #16769 ) ;
#17822 = VERTEX_POINT ( 'NONE', #19262 ) ;
#17823 = ORIENTED_EDGE ( 'NONE', *, *, #7218, .F. ) ;
#17824 = CARTESIAN_POINT ( 'NONE',  ( -43.62245103011230185, -4.418230934988281788, 52.10459351193185285 ) ) ;
#17825 = CARTESIAN_POINT ( 'NONE',  ( -39.64148344771002286, 7.657122216028890982, 32.04930799450052348 ) ) ;
#17826 = FACE_OUTER_BOUND ( 'NONE', #6482, .T. ) ;
#17827 = FACE_OUTER_BOUND ( 'NONE', #25618, .T. ) ;
#17828 = EDGE_CURVE ( 'NONE', #18298, #31962, #20197, .T. ) ;
#17829 = ORIENTED_EDGE ( 'NONE', *, *, #29432, .T. ) ;
#17830 = CYLINDRICAL_SURFACE ( 'NONE', #2861, 2.499999999999997335 ) ;
#17831 = ORIENTED_EDGE ( 'NONE', *, *, #2598, .T. ) ;
#17832 = CARTESIAN_POINT ( 'NONE',  ( 21.09785597605720753, 15.23758267881771111, 47.04930799450052348 ) ) ;
#17833 = CARTESIAN_POINT ( 'NONE',  ( 80.35715816181534876, -5.900224301042253927, 15.64986376169293791 ) ) ;
#17834 = VERTEX_POINT ( 'NONE', #22874 ) ;
#17835 = DIRECTION ( 'NONE',  ( 0.4848096202463636484, 0.8746197071393810862, 0.000000000000000000 ) ) ;
#17836 = CONICAL_SURFACE ( 'NONE', #23059, 85.00000000000001421, 0.7853981633974621568 ) ;
#17837 = CIRCLE ( 'NONE', #22538, 78.50000000000000000 ) ;
#17838 = CARTESIAN_POINT ( 'NONE',  ( -35.51959509086647415, 11.47739873925888077, 52.78069526241495879 ) ) ;
#17839 = PLANE ( 'NONE',  #27858 ) ;
#17840 = LINE ( 'NONE', #27863, #19547 ) ;
#17841 = CARTESIAN_POINT ( 'NONE',  ( 48.40186567930498285, 29.52957786121581307, 45.03923535223908203 ) ) ;
#17842 = AXIS2_PLACEMENT_3D ( 'NONE', #21491, #13970, #23961 ) ;
#17843 = DIRECTION ( 'NONE',  ( -1.101824276508909887E-16, 1.000000000000000000, -0.000000000000000000 ) ) ;
#17844 = DIRECTION ( 'NONE',  ( 1.234978253042719660E-16, -1.000000000000000000, -1.109335647967047851E-31 ) ) ;
#17845 = EDGE_LOOP ( 'NONE', ( #24202, #25484, #5298, #8580 ) ) ;
#17846 = AXIS2_PLACEMENT_3D ( 'NONE', #11417, #16501, #8956 ) ;
#17847 = AXIS2_PLACEMENT_3D ( 'NONE', #27624, #5310, #13189 ) ;
#17848 = CARTESIAN_POINT ( 'NONE',  ( 100.3079064823960493, 25.56454579224780232, 47.04930799450134771 ) ) ;
#17849 = ORIENTED_EDGE ( 'NONE', *, *, #26931, .T. ) ;
#17850 = AXIS2_PLACEMENT_3D ( 'NONE', #29303, #11749, #26356 ) ;
#17851 = DIRECTION ( 'NONE',  ( 1.000000000000000000, 0.000000000000000000, -1.110223024625154963E-14 ) ) ;
#17852 = ORIENTED_EDGE ( 'NONE', *, *, #27579, .F. ) ;
#17853 = EDGE_CURVE ( 'NONE', #15550, #8613, #22717, .T. ) ;
#17854 = ORIENTED_EDGE ( 'NONE', *, *, #10861, .F. ) ;
#17855 = DIRECTION ( 'NONE',  ( 0.2756373558169932236, -0.9612616959383204485, 1.479773560108267395E-16 ) ) ;
#17856 = AXIS2_PLACEMENT_3D ( 'NONE', #29837, #2425, #12441 ) ;
#17857 = EDGE_CURVE ( 'NONE', #7622, #460, #31228, .T. ) ;
#17858 = ORIENTED_EDGE ( 'NONE', *, *, #2524, .F. ) ;
#17859 = EDGE_CURVE ( 'NONE', #22591, #1546, #25016, .T. ) ;
#17860 = EDGE_CURVE ( 'NONE', #12816, #10473, #22285, .T. ) ;
#17861 = AXIS2_PLACEMENT_3D ( 'NONE', #17139, #16976, #9934 ) ;
#17862 = EDGE_CURVE ( 'NONE', #2614, #2467, #30439, .T. ) ;
#17863 = AXIS2_PLACEMENT_3D ( 'NONE', #16180, #20633, #10640 ) ;
#17864 = ORIENTED_EDGE ( 'NONE', *, *, #12198, .F. ) ;
#17865 = AXIS2_PLACEMENT_3D ( 'NONE', #4134, #19551, #27272 ) ;
#17866 = AXIS2_PLACEMENT_3D ( 'NONE', #6012, #3374, #13408 ) ;
#17867 = CARTESIAN_POINT ( 'NONE',  ( -41.02687597405218156, 7.220473278338834788, 60.54930799450051637 ) ) ;
#17868 = CIRCLE ( 'NONE', #1095, 0.9999999999999974465 ) ;
#17869 = EDGE_LOOP ( 'NONE', ( #17083, #8117, #2354, #4043 ) ) ;
#17870 = FACE_OUTER_BOUND ( 'NONE', #10377, .T. ) ;
#17871 = CARTESIAN_POINT ( 'NONE',  ( 48.97837830602554021, 29.34785002538245990, 45.68769290308407705 ) ) ;
#17872 = FACE_OUTER_BOUND ( 'NONE', #23497, .T. ) ;
#17873 = CARTESIAN_POINT ( 'NONE',  ( 48.80717017713595141, 29.37622849631043209, 48.15820438821415195 ) ) ;
#17874 = EDGE_CURVE ( 'NONE', #2041, #9758, #11819, .T. ) ;
#17875 = EDGE_LOOP ( 'NONE', ( #22980, #22557, #32294, #19724 ) ) ;
#17876 = ORIENTED_EDGE ( 'NONE', *, *, #31517, .T. ) ;
#17877 = DIRECTION ( 'NONE',  ( -1.000000000000000000, -1.101824276508909887E-16, 0.000000000000000000 ) ) ;
#17878 = VECTOR ( 'NONE', #17349, 1000.000000000000227 ) ;
#17879 = VERTEX_POINT ( 'NONE', #17949 ) ;
#17880 = CYLINDRICAL_SURFACE ( 'NONE', #15219, 0.1000000000000028644 ) ;
#17881 = CARTESIAN_POINT ( 'NONE',  ( 21.09992658989239089, 26.21183152705960140, 47.04930799450051637 ) ) ;
#17882 = CARTESIAN_POINT ( 'NONE',  ( 21.09785597605719332, 40.06454579224778456, 47.04930799450051637 ) ) ;
#17883 = DIRECTION ( 'NONE',  ( -1.000000000000000000, 0.000000000000000000, 0.000000000000000000 ) ) ;
#17884 = LINE ( 'NONE', #27900, #19011 ) ;
#17885 = APPLICATION_PROTOCOL_DEFINITION ( 'draft international standard', 'automotive_design', 1998, #8664 ) ;
#17886 = EDGE_LOOP ( 'NONE', ( #22413, #21797, #23759, #24840 ) ) ;
#17887 = CYLINDRICAL_SURFACE ( 'NONE', #1907, 85.00000000000001421 ) ;
#17888 = DIRECTION ( 'NONE',  ( 0.000000000000000000, 0.000000000000000000, -1.000000000000000000 ) ) ;
#17889 = CARTESIAN_POINT ( 'NONE',  ( 52.13393605659406660, -5.936921830459686689, 107.4316605894145624 ) ) ;
#17890 = CIRCLE ( 'NONE', #21035, 18.86195243859455672 ) ;
#17891 = EDGE_CURVE ( 'NONE', #19940, #28859, #383, .T. ) ;
#17892 = ORIENTED_EDGE ( 'NONE', *, *, #26249, .F. ) ;
#17893 = CARTESIAN_POINT ( 'NONE',  ( 21.09785597605719332, 25.56454579224779877, 47.04930799450051637 ) ) ;
#17894 = FACE_OUTER_BOUND ( 'NONE', #8821, .T. ) ;
#17895 = AXIS2_PLACEMENT_3D ( 'NONE', #18155, #25874, #10794 ) ;
#17896 = EDGE_CURVE ( 'NONE', #19042, #20793, #4670, .T. ) ;
#17897 = CARTESIAN_POINT ( 'NONE',  ( -30.60166825031904025, 11.23651971625239021, 22.94476225488443433 ) ) ;
#17898 =( BOUNDED_CURVE ( )  B_SPLINE_CURVE ( 3, ( #12132, #6708, #16706, #7197 ),
 .UNSPECIFIED., .F., .F. ) 
 B_SPLINE_CURVE_WITH_KNOTS ( ( 4, 4 ),
 ( 0.4372979894901917186, 1.133349320028354423 ),
 .UNSPECIFIED. ) 
 CURVE ( )  GEOMETRIC_REPRESENTATION_ITEM ( )  RATIONAL_B_SPLINE_CURVE ( ( 1.000000000000000000, 0.9600319177481759780, 0.9600319177481759780, 1.000000000000000000 ) ) 
 REPRESENTATION_ITEM ( '' )  );
#17899 = VECTOR ( 'NONE', #2203, 999.9999999999998863 ) ;
#17900 = EDGE_CURVE ( 'NONE', #1639, #21428, #27796, .T. ) ;
#17901 = VERTEX_POINT ( 'NONE', #20089 ) ;
#17902 = VERTEX_POINT ( 'NONE', #4838 ) ;
#17903 = DIRECTION ( 'NONE',  ( -0.000000000000000000, -1.000000000000000000, -0.000000000000000000 ) ) ;
#17904 = FACE_OUTER_BOUND ( 'NONE', #27420, .T. ) ;
#17905 = FACE_OUTER_BOUND ( 'NONE', #4844, .T. ) ;
#17906 = ORIENTED_EDGE ( 'NONE', *, *, #2850, .T. ) ;
#17907 = AXIS2_PLACEMENT_3D ( 'NONE', #20097, #4678, #7640 ) ;
#17908 = CARTESIAN_POINT ( 'NONE',  ( -41.24971778908466291, 11.62557032131817358, 57.04930799450051637 ) ) ;
#17909 = DIRECTION ( 'NONE',  ( -0.9612616959383221138, -0.2756373558169876170, 0.000000000000000000 ) ) ;
#17910 = CARTESIAN_POINT ( 'NONE',  ( 47.09785597605719687, 24.76454579224779806, 47.04930799450078638 ) ) ;
#17911 = CARTESIAN_POINT ( 'NONE',  ( 45.96182992765471909, 25.90087065737812466, 44.82232689504102296 ) ) ;
#17912 = CARTESIAN_POINT ( 'NONE',  ( 21.09785597605719332, -16.43545420775217281, 47.04930799450051637 ) ) ;
#17913 = FACE_OUTER_BOUND ( 'NONE', #4487, .T. ) ;
#17914 = CARTESIAN_POINT ( 'NONE',  ( -4.902144023942810236, 25.56454579224779167, 47.04930799450042400 ) ) ;
#17915 = DIRECTION ( 'NONE',  ( -1.000000000000000000, 0.000000000000000000, 0.000000000000000000 ) ) ;
#17916 = CARTESIAN_POINT ( 'NONE',  ( 21.09992658989239089, 27.09164230456639899, 47.04930799450051637 ) ) ;
#17917 = DIRECTION ( 'NONE',  ( -1.101824276508909887E-16, 1.000000000000000000, -0.000000000000000000 ) ) ;
#17918 = CARTESIAN_POINT ( 'NONE',  ( 21.09785597605719332, 12.26495659406217342, 47.04930799450051637 ) ) ;
#17919 = VERTEX_POINT ( 'NONE', #5330 ) ;
#17920 = ORIENTED_EDGE ( 'NONE', *, *, #256, .F. ) ;
#17921 = DIRECTION ( 'NONE',  ( -0.000000000000000000, -1.000000000000000000, -0.000000000000000000 ) ) ;
#17922 = CIRCLE ( 'NONE', #16856, 0.09999999999999700795 ) ;
#17923 = DIRECTION ( 'NONE',  ( -1.101824276508909887E-16, 1.000000000000000000, -0.000000000000000000 ) ) ;
#17924 = CARTESIAN_POINT ( 'NONE',  ( -32.94875189376105595, -2.247009719175835141, 13.30861947577388271 ) ) ;
#17925 = DIRECTION ( 'NONE',  ( -1.000000000000000000, -1.101824276508909887E-16, 0.000000000000000000 ) ) ;
#17926 = EDGE_LOOP ( 'NONE', ( #2563, #31953, #6963, #16630 ) ) ;
#17927 = DIRECTION ( 'NONE',  ( -0.000000000000000000, -1.000000000000000000, -0.000000000000000000 ) ) ;
#17928 = CARTESIAN_POINT ( 'NONE',  ( 21.09785597605719332, 12.11061942510878886, -8.482108500610603841 ) ) ;
#17929 = CARTESIAN_POINT ( 'NONE',  ( 48.83059987400640267, 28.25948166895303260, 48.97189179988551899 ) ) ;
#17930 = ORIENTED_EDGE ( 'NONE', *, *, #9993, .T. ) ;
#17931 = VERTEX_POINT ( 'NONE', #24857 ) ;
#17932 = CARTESIAN_POINT ( 'NONE',  ( -40.70217169293940884, 9.596168124565080504, 35.54930799450051637 ) ) ;
#17933 = CARTESIAN_POINT ( 'NONE',  ( 46.99023568444673060, 26.52451373492759856, 49.12151524109405898 ) ) ;
#17934 = CARTESIAN_POINT ( 'NONE',  ( 46.99023568444673060, 29.23791119454914877, 49.12151524109405898 ) ) ;
#17935 = CARTESIAN_POINT ( 'NONE',  ( -39.40299142976220281, -5.935884043940212962, 77.96317429586483172 ) ) ;
#17936 = CARTESIAN_POINT ( 'NONE',  ( 21.09785597605720042, -16.93545420775220478, -31.35069200549948221 ) ) ;
#17937 = VECTOR ( 'NONE', #32062, 1000.000000000000000 ) ;
#17938 = EDGE_CURVE ( 'NONE', #4682, #25773, #15494, .T. ) ;
#17939 = EDGE_LOOP ( 'NONE', ( #23939, #28005, #28076, #8661, #11307, #16073, #3318, #5930, #9436, #30205, #2999, #24425 ) ) ;
#17940 = ADVANCED_FACE ( 'NONE', ( #30116 ), #31733, .T. ) ;
#17941 = CARTESIAN_POINT ( 'NONE',  ( 21.09992658989239089, 26.59164230456639899, 47.04930799450051637 ) ) ;
#17942 = DIRECTION ( 'NONE',  ( 0.000000000000000000, 1.000000000000000000, -0.000000000000000000 ) ) ;
#17943 = ORIENTED_EDGE ( 'NONE', *, *, #11046, .T. ) ;
#17944 = CIRCLE ( 'NONE', #23193, 0.1250000000000001110 ) ;
#17945 = LINE ( 'NONE', #15961, #1797 ) ;
#17946 = FACE_OUTER_BOUND ( 'NONE', #22473, .T. ) ;
#17947 = CIRCLE ( 'NONE', #20573, 1.300000000000002487 ) ;
#17948 = ORIENTED_EDGE ( 'NONE', *, *, #16734, .T. ) ;
#17949 = CARTESIAN_POINT ( 'NONE',  ( 8.732853799281732776, 31.72145308207317171, 47.04930799450051637 ) ) ;
#17950 = CARTESIAN_POINT ( 'NONE',  ( 33.46699938050304013, 26.96183152705960495, 47.04930799450051637 ) ) ;
#17951 = DIRECTION ( 'NONE',  ( 0.8746197071393926326, -0.4848096202463430537, -8.676864087101709653E-18 ) ) ;
#17952 = VECTOR ( 'NONE', #15548, 1000.000000000000000 ) ;
#17953 = DIRECTION ( 'NONE',  ( 0.000000000000000000, 0.000000000000000000, 1.000000000000000000 ) ) ;
#17954 = CARTESIAN_POINT ( 'NONE',  ( 21.09785597605719332, -6.659195188345857552, -20.12191896776992905 ) ) ;
#17955 = ORIENTED_EDGE ( 'NONE', *, *, #17286, .F. ) ;
#17956 = DIRECTION ( 'NONE',  ( -1.101824276508909887E-16, 1.000000000000000000, -0.000000000000000000 ) ) ;
#17957 = CARTESIAN_POINT ( 'NONE',  ( -40.11286833322908052, 2.887657226147511302, 57.04930799450051637 ) ) ;
#17958 = DIRECTION ( 'NONE',  ( 0.4544104193609990738, 0.000000000000000000, 0.8907924397839043218 ) ) ;
#17959 = CARTESIAN_POINT ( 'NONE',  ( -43.35833523721898075, -3.935454207752190126, 42.04930799450051637 ) ) ;
#17960 = DIRECTION ( 'NONE',  ( -1.101824276508909887E-16, 1.000000000000000000, -0.000000000000000000 ) ) ;
#17961 = ORIENTED_EDGE ( 'NONE', *, *, #22025, .F. ) ;
#17962 = CARTESIAN_POINT ( 'NONE',  ( -42.50976151518963064, 14.59907569580870046, 37.04930799450052348 ) ) ;
#17963 = DIRECTION ( 'NONE',  ( -0.000000000000000000, -1.000000000000000000, -0.000000000000000000 ) ) ;
#17964 = EDGE_LOOP ( 'NONE', ( #6876, #13827, #7438, #4041 ) ) ;
#17965 = DIRECTION ( 'NONE',  ( -1.000000000000000000, 0.000000000000000000, 0.000000000000000000 ) ) ;
#17966 = CARTESIAN_POINT ( 'NONE',  ( 21.09785597605720042, 12.06852548259731961, 102.7275235127243320 ) ) ;
#17967 = CARTESIAN_POINT ( 'NONE',  ( 49.00477282619483788, 29.13168691486794515, 45.28585184200404967 ) ) ;
#17968 = DIRECTION ( 'NONE',  ( 0.000000000000000000, 1.000000000000000000, -0.000000000000000000 ) ) ;
#17969 = AXIS2_PLACEMENT_3D ( 'NONE', #477, #8045, #18034 ) ;
#17970 = ORIENTED_EDGE ( 'NONE', *, *, #8532, .T. ) ;
#17971 = CARTESIAN_POINT ( 'NONE',  ( -40.44300931641782171, 7.361061430353638357, 60.31640775708849844 ) ) ;
#17972 = ORIENTED_EDGE ( 'NONE', *, *, #22450, .T. ) ;
#17973 = AXIS2_PLACEMENT_3D ( 'NONE', #6085, #15600, #28414 ) ;
#17974 = ORIENTED_EDGE ( 'NONE', *, *, #7856, .T. ) ;
#17975 = ADVANCED_FACE ( 'NONE', ( #32412 ), #27482, .F. ) ;
#17976 = EDGE_CURVE ( 'NONE', #2645, #29624, #804, .T. ) ;
#17977 = EDGE_CURVE ( 'NONE', #21227, #3106, #24925, .T. ) ;
#17978 = VECTOR ( 'NONE', #6507, 1000.000000000000000 ) ;
#17979 = CIRCLE ( 'NONE', #22712, 0.09999999999999945044 ) ;
#17980 = EDGE_CURVE ( 'NONE', #17663, #12804, #10741, .T. ) ;
#17981 = CARTESIAN_POINT ( 'NONE',  ( 52.04314975454045111, -5.936463391119990440, -13.39944846985862981 ) ) ;
#17982 = DIRECTION ( 'NONE',  ( 0.000000000000000000, 1.000000000000000000, 0.000000000000000000 ) ) ;
#17983 = CARTESIAN_POINT ( 'NONE',  ( 81.72575882806418690, -5.935454207752202116, 16.07118271501079576 ) ) ;
#17984 = ORIENTED_EDGE ( 'NONE', *, *, #23669, .T. ) ;
#17985 = ORIENTED_EDGE ( 'NONE', *, *, #3999, .F. ) ;
#17986 = CIRCLE ( 'NONE', #29554, 13.00178401536290806 ) ;
#17987 = DIRECTION ( 'NONE',  ( -1.000000000000000000, 0.000000000000000000, 0.000000000000000000 ) ) ;
#17988 = CARTESIAN_POINT ( 'NONE',  ( -40.50720532202722524, 7.584939507552747706, 60.08350751967648762 ) ) ;
#17989 = CARTESIAN_POINT ( 'NONE',  ( -32.97738962991574851, -0.5062580946980150820, 80.43174492715770896 ) ) ;
#17990 = VECTOR ( 'NONE', #8191, 1000.000000000000000 ) ;
#17991 = CARTESIAN_POINT ( 'NONE',  ( 21.09992658989239089, 29.09184655352418858, 47.04930799450051637 ) ) ;
#17992 = ORIENTED_EDGE ( 'NONE', *, *, #6408, .T. ) ;
#17993 = DIRECTION ( 'NONE',  ( -1.000000000000000000, 0.000000000000000000, 0.000000000000000000 ) ) ;
#17994 = ORIENTED_EDGE ( 'NONE', *, *, #29204, .F. ) ;
#17995 = DIRECTION ( 'NONE',  ( 0.000000000000000000, 0.000000000000000000, 1.000000000000000000 ) ) ;
#17996 = FACE_OUTER_BOUND ( 'NONE', #1299, .T. ) ;
#17997 = EDGE_LOOP ( 'NONE', ( #7196, #26345, #22441, #5914 ) ) ;
#17998 = DIRECTION ( 'NONE',  ( 0.000000000000000000, 1.000000000000000000, -0.000000000000000000 ) ) ;
#17999 = CARTESIAN_POINT ( 'NONE',  ( 81.65768700022189819, -5.935454207752202116, 16.07118271501079931 ) ) ;
#18000 = CARTESIAN_POINT ( 'NONE',  ( 46.04327488119035650, 22.93807716476589675, 48.37782978030396208 ) ) ;
#18001 = CARTESIAN_POINT ( 'NONE',  ( -40.46271621608484281, 3.081581074246047436, 45.54930799450051637 ) ) ;
#18002 = B_SPLINE_CURVE_WITH_KNOTS ( 'NONE', 3,
 ( #23706, #3841, #31422, #6472, #16473, #16627, #21719, #19248, #17451, #26816, #32395, #24846, #21877, #20076, #4332, #2516, #2365, #2198, #19909, #15003, #17118, #4496, #14675, #25006, #29448, #11881, #27137, #24680, #27473, #12382, #4655, #14843 ),
 .UNSPECIFIED., .F., .F.,
 ( 4, 2, 2, 2, 2, 2, 2, 2, 2, 2, 2, 2, 2, 2, 2, 4 ),
 ( 0.003975046523139969153, 0.004428463406335606325, 0.004881880289531242631, 0.005335297172726879804, 0.005788714055922516109, 0.006242130939118153282, 0.006695547822313789588, 0.007148964705509426761, 0.007602381588705063933, 0.008509215355096317462, 0.008962632238291936421, 0.009416049121487553644, 0.009869466004683170868, 0.01032288288787878809, 0.01077629977107440531, 0.01122971665427002254 ),
 .UNSPECIFIED. ) ;
#18003 = CIRCLE ( 'NONE', #2280, 19.99999999999999645 ) ;
#18004 = DIRECTION ( 'NONE',  ( -1.101824276508909887E-16, 1.000000000000000000, -0.000000000000000000 ) ) ;
#18005 = VECTOR ( 'NONE', #8999, 1000.000000000000000 ) ;
#18006 = DIRECTION ( 'NONE',  ( -1.101824276508909887E-16, 1.000000000000000000, -0.000000000000000000 ) ) ;
#18007 = DIRECTION ( 'NONE',  ( -1.101824276508909887E-16, 1.000000000000000000, -0.000000000000000000 ) ) ;
#18008 = ORIENTED_EDGE ( 'NONE', *, *, #32352, .T. ) ;
#18010 = ADVANCED_FACE ( 'NONE', ( #26139 ), #7632, .T. ) ;
#18009 = DIRECTION ( 'NONE',  ( 0.4544104193609903586, 0.000000000000000000, 0.8907924397839087627 ) ) ;
#18011 = EDGE_CURVE ( 'NONE', #1187, #13517, #15646, .T. ) ;
#18012 = CARTESIAN_POINT ( 'NONE',  ( 21.09785597605720042, -16.73545420775220194, 47.04930799450051637 ) ) ;
#18013 = ORIENTED_EDGE ( 'NONE', *, *, #23351, .T. ) ;
#18014 = ORIENTED_EDGE ( 'NONE', *, *, #19552, .T. ) ;
#18015 = DIRECTION ( 'NONE',  ( -1.101824276508909887E-16, 1.000000000000000000, -0.000000000000000000 ) ) ;
#18016 = VERTEX_POINT ( 'NONE', #18579 ) ;
#18017 = AXIS2_PLACEMENT_3D ( 'NONE', #18417, #864, #11205 ) ;
#18018 = EDGE_CURVE ( 'NONE', #21770, #30824, #28594, .T. ) ;
#18019 = CONICAL_SURFACE ( 'NONE', #27992, 67.17122696227043832, 1.291543646476234874 ) ;
#18020 = ORIENTED_EDGE ( 'NONE', *, *, #6523, .T. ) ;
#18021 = DIRECTION ( 'NONE',  ( -0.000000000000000000, 1.000000000000000000, -0.000000000000000000 ) ) ;
#18022 = ORIENTED_EDGE ( 'NONE', *, *, #31628, .F. ) ;
#18023 =( LENGTH_UNIT ( ) NAMED_UNIT ( * ) SI_UNIT ( .MILLI., .METRE. ) );
#18024 = CARTESIAN_POINT ( 'NONE',  ( 47.32773967697124817, 29.57151323798673914, 44.96316438875158639 ) ) ;
#18025 = ADVANCED_FACE ( 'NONE', ( #5972 ), #23520, .F. ) ;
#18026 = CARTESIAN_POINT ( 'NONE',  ( 47.20353132263855400, 27.50956182964376140, 45.01455027646040463 ) ) ;
#18027 = ORIENTED_EDGE ( 'NONE', *, *, #28504, .F. ) ;
#18028 = ORIENTED_EDGE ( 'NONE', *, *, #370, .F. ) ;
#18029 = LINE ( 'NONE', #28055, #6399 ) ;
#18030 = ORIENTED_EDGE ( 'NONE', *, *, #15450, .F. ) ;
#18031 = EDGE_CURVE ( 'NONE', #7358, #15249, #1111, .T. ) ;
#18032 = CARTESIAN_POINT ( 'NONE',  ( 8.482002859293428898, 27.21664230456639899, 47.04930799450051637 ) ) ;
#18033 = CARTESIAN_POINT ( 'NONE',  ( 48.43849231507899589, 9.162376348828955130, 98.41682639182559456 ) ) ;
#18034 = DIRECTION ( 'NONE',  ( -1.000000000000000000, 0.000000000000000000, 0.000000000000000000 ) ) ;
#18035 = VECTOR ( 'NONE', #21850, 1000.000000000000000 ) ;
#18036 = DIRECTION ( 'NONE',  ( -1.000000000000000000, 0.000000000000000000, 0.000000000000000000 ) ) ;
#18037 = ITEM_DEFINED_TRANSFORMATION ( 'NONE', 'NONE', #30734,  #8172 ) ;
#18038 = ORIENTED_EDGE ( 'NONE', *, *, #4536, .F. ) ;
#18039 = CARTESIAN_POINT ( 'NONE',  ( 34.59963999142011204, 17.16474120167318063, 47.04930799450052348 ) ) ;
#18040 = EDGE_CURVE ( 'NONE', #15519, #7154, #8101, .T. ) ;
#18041 = CIRCLE ( 'NONE', #31684, 12.62506659569710266 ) ;
#18042 = DIRECTION ( 'NONE',  ( -1.101824276508909887E-16, 1.000000000000000000, -0.000000000000000000 ) ) ;
#18043 = EDGE_CURVE ( 'NONE', #29979, #22618, #32200, .T. ) ;
#18044 = AXIS2_PLACEMENT_3D ( 'NONE', #7577, #14806, #24967 ) ;
#18045 = EDGE_CURVE ( 'NONE', #5045, #8696, #25661, .T. ) ;
#18046 = DIRECTION ( 'NONE',  ( 0.2756373558169962767, -0.9612616959383197823, 1.479773560108262218E-16 ) ) ;
#18047 = DIRECTION ( 'NONE',  ( -1.000000000000000000, 0.000000000000000000, 0.000000000000000000 ) ) ;
#18048 = EDGE_LOOP ( 'NONE', ( #19955, #2274, #5850, #2084, #9310, #7016, #31758, #8149 ) ) ;
#18049 = CARTESIAN_POINT ( 'NONE',  ( 21.09992658989238734, 30.72145308207317882, 47.04930799450051637 ) ) ;
#18050 = LINE ( 'NONE', #7892, #2013 ) ;
#18051 = FACE_OUTER_BOUND ( 'NONE', #25560, .T. ) ;
#18052 = ORIENTED_EDGE ( 'NONE', *, *, #22476, .F. ) ;
#18053 = ADVANCED_FACE ( 'NONE', ( #27971 ), #4430, .F. ) ;
#18054 = VERTEX_POINT ( 'NONE', #13518 ) ;
#18055 = AXIS2_PLACEMENT_3D ( 'NONE', #18537, #30717, #15448 ) ;
#18056 = VERTEX_POINT ( 'NONE', #13683 ) ;
#18057 = AXIS2_PLACEMENT_3D ( 'NONE', #27029, #4542, #2079 ) ;
#18058 = FACE_BOUND ( 'NONE', #9179, .T. ) ;
#18059 = CARTESIAN_POINT ( 'NONE',  ( 21.09992658989238734, 32.21183152705962272, 47.04930799450051637 ) ) ;
#18061 = FACE_OUTER_BOUND ( 'NONE', #1191, .T. ) ;
#18060 = VECTOR ( 'NONE', #763, 1000.000000000000000 ) ;
#18062 = AXIS2_PLACEMENT_3D ( 'NONE', #17239, #2157, #24468 ) ;
#18063 = ORIENTED_EDGE ( 'NONE', *, *, #201, .T. ) ;
#18064 = DIRECTION ( 'NONE',  ( 1.000000000000000000, 0.000000000000000000, 0.000000000000000000 ) ) ;
#18065 = DIRECTION ( 'NONE',  ( -1.000000000000000000, 0.000000000000000000, 0.000000000000000000 ) ) ;
#18066 = ADVANCED_FACE ( 'NONE', ( #23685 ), #15493, .T. ) ;
#18067 = CARTESIAN_POINT ( 'NONE',  ( 21.09785597605720753, 13.86454579224779948, 47.04930799450052348 ) ) ;
#18068 = EDGE_CURVE ( 'NONE', #28859, #16068, #26904, .T. ) ;
#18069 = CARTESIAN_POINT ( 'NONE',  ( 21.09785597605720753, 14.86454579224779948, 47.04930799450052348 ) ) ;
#18070 = DIRECTION ( 'NONE',  ( -1.188208965918165239E-16, -1.880121038077813132E-16, -1.000000000000000000 ) ) ;
#18071 = CARTESIAN_POINT ( 'NONE',  ( -39.58809650894544774, 2.596771453999702661, 45.14930799450051779 ) ) ;
#18072 = CARTESIAN_POINT ( 'NONE',  ( 52.09785597605720397, 13.86454579224779948, 47.04930799450051637 ) ) ;
#18073 = CARTESIAN_POINT ( 'NONE',  ( 21.09992658989239089, 27.97145308207318237, 47.04930799450051637 ) ) ;
#18074 = DIRECTION ( 'NONE',  ( -0.9761574614375593262, 0.2110602665713100234, -0.05069688703093822718 ) ) ;
#18075 = SHAPE_REPRESENTATION_RELATIONSHIP ( 'NONE' , 'NONE' ,  #11371, #4182 ) ;
#18076 = VERTEX_POINT ( 'NONE', #30601 ) ;
#18077 = VERTEX_POINT ( 'NONE', #3333 ) ;
#18078 = DIRECTION ( 'NONE',  ( 0.9612616959383205595, 0.2756373558169932236, -1.660411357259282445E-16 ) ) ;
#18079 = ADVANCED_FACE ( 'NONE', ( #23362 ), #10895, .T. ) ;
#18080 = EDGE_CURVE ( 'NONE', #21342, #30851, #3816, .T. ) ;
#18081 = CARTESIAN_POINT ( 'NONE',  ( 21.09785597605719332, 42.30003263981368633, 17.04930799450051637 ) ) ;
#18082 = VECTOR ( 'NONE', #9677, 999.9999999999998863 ) ;
#18083 = ORIENTED_EDGE ( 'NONE', *, *, #3109, .F. ) ;
#18084 =( BOUNDED_CURVE ( )  B_SPLINE_CURVE ( 3, ( #20641, #28193, #30665, #10810 ),
 .UNSPECIFIED., .F., .F. ) 
 B_SPLINE_CURVE_WITH_KNOTS ( ( 4, 4 ),
 ( 1.570796326794906994, 2.992702705980325284 ),
 .UNSPECIFIED. ) 
 CURVE ( )  GEOMETRIC_REPRESENTATION_ITEM ( )  RATIONAL_B_SPLINE_CURVE ( ( 1.000000000000000000, 0.8384934736035529745, 0.8384934736035529745, 1.000000000000000000 ) ) 
 REPRESENTATION_ITEM ( '' )  );
#18085 = CARTESIAN_POINT ( 'NONE',  ( 33.46699938050303302, 38.56284415653841791, 47.04930799450051637 ) ) ;
#18086 = CARTESIAN_POINT ( 'NONE',  ( 48.66895200406656841, 28.46155426599985105, 44.62753372671560470 ) ) ;
#18087 = ORIENTED_EDGE ( 'NONE', *, *, #16987, .T. ) ;
#18088 = ORIENTED_EDGE ( 'NONE', *, *, #20403, .F. ) ;
#18090 = VECTOR ( 'NONE', #15605, 1000.000000000000227 ) ;
#18089 = DIRECTION ( 'NONE',  ( 0.9612616959383205595, 0.2756373558169931681, -1.660411357259282445E-16 ) ) ;
#18091 = CARTESIAN_POINT ( 'NONE',  ( 48.83862994770794330, 25.24118040159427068, 48.17861352429476796 ) ) ;
#18092 = CIRCLE ( 'NONE', #12337, 0.9999999999999974465 ) ;
#18093 = CIRCLE ( 'NONE', #29103, 2.499999999999998668 ) ;
#18094 = CARTESIAN_POINT ( 'NONE',  ( -39.45284321493671342, -5.935743718174008698, 77.88873351080283669 ) ) ;
#18095 = AXIS2_PLACEMENT_3D ( 'NONE', #1719, #11735, #21731 ) ;
#18096 = EDGE_LOOP ( 'NONE', ( #8110, #19584, #23115, #1597 ) ) ;
#18097 = FACE_OUTER_BOUND ( 'NONE', #15212, .T. ) ;
#18098 = CARTESIAN_POINT ( 'NONE',  ( 8.823575513742486720, 34.59164230456639899, 46.72789464899623368 ) ) ;
#18099 = ORIENTED_EDGE ( 'NONE', *, *, #7846, .T. ) ;
#18100 = AXIS2_PLACEMENT_3D ( 'NONE', #11442, #21440, #8983 ) ;
#18101 = LINE ( 'NONE', #10405, #28543 ) ;
#18102 = LINE ( 'NONE', #26301, #21903 ) ;
#18103 = AXIS2_PLACEMENT_3D ( 'NONE', #20328, #8201, #31007 ) ;
#18104 = CIRCLE ( 'NONE', #22299, 0.1249999999999983763 ) ;
#18105 = DIRECTION ( 'NONE',  ( -1.000000000000000000, 0.000000000000000000, 0.000000000000000000 ) ) ;
#18106 = ORIENTED_EDGE ( 'NONE', *, *, #18853, .T. ) ;
#18107 = CARTESIAN_POINT ( 'NONE',  ( -41.93344242462055149, 13.82826554927148166, 54.56265170360538264 ) ) ;
#18108 = AXIS2_PLACEMENT_3D ( 'NONE', #26505, #1547, #21566 ) ;
#18109 = CARTESIAN_POINT ( 'NONE',  ( 79.67628629021933762, -5.773219817368594242, 78.78228565784779391 ) ) ;
#18110 = FACE_OUTER_BOUND ( 'NONE', #27833, .T. ) ;
#18111 = CARTESIAN_POINT ( 'NONE',  ( 21.09992658989239089, 26.09164230456639899, 47.04930799450051637 ) ) ;
#18112 = FACE_BOUND ( 'NONE', #18453, .T. ) ;
#18113 = ORIENTED_EDGE ( 'NONE', *, *, #11095, .T. ) ;
#18114 = FACE_OUTER_BOUND ( 'NONE', #27800, .T. ) ;
#18115 = DIRECTION ( 'NONE',  ( -2.779292025043186357E-18, 1.288349127009862211E-17, -1.000000000000000000 ) ) ;
#18116 = EDGE_CURVE ( 'NONE', #9970, #24538, #8173, .T. ) ;
#18117 = DIRECTION ( 'NONE',  ( -1.101824276508909887E-16, 1.000000000000000000, -0.000000000000000000 ) ) ;
#18118 = VECTOR ( 'NONE', #31114, 1000.000000000000000 ) ;
#18119 = EDGE_CURVE ( 'NONE', #9364, #5905, #6514, .T. ) ;
#18120 = EDGE_CURVE ( 'NONE', #29942, #26412, #26499, .T. ) ;
#18121 = CARTESIAN_POINT ( 'NONE',  ( 49.19517401419062708, 26.18655426599985958, 48.40991706654173754 ) ) ;
#18122 = ORIENTED_EDGE ( 'NONE', *, *, #7421, .F. ) ;
#18123 = CARTESIAN_POINT ( 'NONE',  ( -38.36853489569023168, 7.065850718397948427, 61.94930799450052206 ) ) ;
#18124 = CARTESIAN_POINT ( 'NONE',  ( 49.70752207505586284, 24.90576773639369179, 46.59986279770737383 ) ) ;
#18125 = CARTESIAN_POINT ( 'NONE',  ( -40.62123369608615775, 7.650200974017423050, 34.54930799450052348 ) ) ;
#18126 = ORIENTED_EDGE ( 'NONE', *, *, #16552, .T. ) ;
#18127 = CARTESIAN_POINT ( 'NONE',  ( -10.58731244131463178, -5.819500620027731941, -11.73843591528525110 ) ) ;
#18128 = LINE ( 'NONE', #3185, #12575 ) ;
#18129 = CARTESIAN_POINT ( 'NONE',  ( 49.98072202819531640, 29.04488759933318676, 47.19902993264913960 ) ) ;
#18130 = CARTESIAN_POINT ( 'NONE',  ( 54.82722624670270051, -2.181906231262848106, -7.903189434301322258 ) ) ;
#18131 = ORIENTED_EDGE ( 'NONE', *, *, #20888, .T. ) ;
#18132 = DIRECTION ( 'NONE',  ( 0.000000000000000000, 0.000000000000000000, -1.000000000000000000 ) ) ;
#18133 = VERTEX_POINT ( 'NONE', #29420 ) ;
#18134 = CIRCLE ( 'NONE', #7128, 12.36707279061065101 ) ;
#18135 = ORIENTED_EDGE ( 'NONE', *, *, #6814, .T. ) ;
#18136 = FACE_OUTER_BOUND ( 'NONE', #4696, .T. ) ;
#18137 = DIRECTION ( 'NONE',  ( 0.000000000000000000, 0.000000000000000000, 1.000000000000000000 ) ) ;
#18138 = CARTESIAN_POINT ( 'NONE',  ( 100.3079064823960493, 25.56454579224780232, 47.04930799450134771 ) ) ;
#18139 = ORIENTED_EDGE ( 'NONE', *, *, #17649, .T. ) ;
#18140 = DIRECTION ( 'NONE',  ( -0.000000000000000000, -1.000000000000000000, -0.000000000000000000 ) ) ;
#18141 = EDGE_LOOP ( 'NONE', ( #13317, #10282, #9044, #7476 ) ) ;
#18142 = DIRECTION ( 'NONE',  ( 0.000000000000000000, 0.000000000000000000, -1.000000000000000000 ) ) ;
#18143 = LINE ( 'NONE', #10624, #20150 ) ;
#18144 = CARTESIAN_POINT ( 'NONE',  ( -32.18821136934754179, 1.455588635105943274, 79.63912307355188602 ) ) ;
#18145 = LINE ( 'NONE', #8309, #24140 ) ;
#18146 = ORIENTED_EDGE ( 'NONE', *, *, #3822, .F. ) ;
#18147 = CARTESIAN_POINT ( 'NONE',  ( -11.39532592801639410, -5.321843574075690420, 103.8276984696742034 ) ) ;
#18148 = ORIENTED_EDGE ( 'NONE', *, *, #27282, .F. ) ;
#18149 = DIRECTION ( 'NONE',  ( -0.000000000000000000, 1.000000000000000000, -0.000000000000000000 ) ) ;
#18150 = PRODUCT_DEFINITION_FORMATION_WITH_SPECIFIED_SOURCE ( 'ANY', '', #13281, .NOT_KNOWN. ) ;
#18151 = ORIENTED_EDGE ( 'NONE', *, *, #11527, .T. ) ;
#18152 = DIRECTION ( 'NONE',  ( -0.1651779284337324960, 0.9862637841664575467, -1.082442759285643960E-14 ) ) ;
#18153 = EDGE_CURVE ( 'NONE', #5962, #8855, #7579, .T. ) ;
#18154 = CARTESIAN_POINT ( 'NONE',  ( -35.76183559804942291, 11.10708444000149342, 52.41472866846790168 ) ) ;
#18155 = CARTESIAN_POINT ( 'NONE',  ( 21.09992658989239089, 27.59164230456639544, 47.04930799450051637 ) ) ;
#18156 = FACE_OUTER_BOUND ( 'NONE', #4814, .T. ) ;
#18157 = EDGE_CURVE ( 'NONE', #28443, #31932, #18041, .T. ) ;
#18158 = EDGE_CURVE ( 'NONE', #13775, #8613, #14986, .T. ) ;
#18159 = CARTESIAN_POINT ( 'NONE',  ( 45.35708200440645044, 25.50457786121582515, 45.92000246470679770 ) ) ;
#18160 = ADVANCED_FACE ( 'NONE', ( #19221 ), #9233, .F. ) ;
#18161 = CARTESIAN_POINT ( 'NONE',  ( 21.09992658989238734, 38.56284415653841791, 47.04930799450051637 ) ) ;
#18162 = CARTESIAN_POINT ( 'NONE',  ( -40.70484894842233103, 8.274204744976163539, 59.64930799450051779 ) ) ;
#18163 = ADVANCED_FACE ( 'NONE', ( #24320 ), #13858, .T. ) ;
#18164 = ADVANCED_FACE ( 'NONE', ( #14000 ), #17532, .T. ) ;
#18165 = ORIENTED_EDGE ( 'NONE', *, *, #17597, .T. ) ;
#18166 = DIRECTION ( 'NONE',  ( -1.000000000000000000, 0.000000000000000000, 0.000000000000000000 ) ) ;
#18167 = VECTOR ( 'NONE', #19383, 1000.000000000000114 ) ;
#18168 = DIRECTION ( 'NONE',  ( -1.000000000000000000, 0.000000000000000000, 0.000000000000000000 ) ) ;
#18169 = ORIENTED_EDGE ( 'NONE', *, *, #747, .F. ) ;
#18170 = VERTEX_POINT ( 'NONE', #8901 ) ;
#18171 = CARTESIAN_POINT ( 'NONE',  ( -11.98039162717269868, 0.3723237022605148661, 100.7399880312177345 ) ) ;
#18172 = ORIENTED_EDGE ( 'NONE', *, *, #19982, .T. ) ;
#18173 = VECTOR ( 'NONE', #20588, 1000.000000000000000 ) ;
#18174 = ORIENTED_EDGE ( 'NONE', *, *, #30320, .F. ) ;
#18175 = DIRECTION ( 'NONE',  ( -1.000000000000000000, 0.000000000000000000, 0.000000000000000000 ) ) ;
#18176 = ADVANCED_FACE ( 'NONE', ( #23995 ), #16930, .T. ) ;
#18177 = ORIENTED_EDGE ( 'NONE', *, *, #10951, .T. ) ;
#18178 = CARTESIAN_POINT ( 'NONE',  ( 47.86511985000206693, 22.93807716476589320, 48.55339511290479493 ) ) ;
#18179 = LINE ( 'NONE', #5724, #16510 ) ;
#18180 = DIRECTION ( 'NONE',  ( -1.000000000000000000, -1.101824276508909887E-16, 0.000000000000000000 ) ) ;
#18181 = CARTESIAN_POINT ( 'NONE',  ( 45.81741271322955100, 28.50122849631042499, 49.02305402274571122 ) ) ;
#18182 = ORIENTED_EDGE ( 'NONE', *, *, #7039, .T. ) ;
#18183 = ORIENTED_EDGE ( 'NONE', *, *, #11893, .F. ) ;
#18184 = FILL_AREA_STYLE_COLOUR ( '', #4316 ) ;
#18185 = ORIENTED_EDGE ( 'NONE', *, *, #3404, .F. ) ;
#18186 = CARTESIAN_POINT ( 'NONE',  ( 41.51205063648687599, 11.92558985988973497, 99.90211174246701376 ) ) ;
#18187 = CARTESIAN_POINT ( 'NONE',  ( 51.51172421616634978, 5.323792735596120096, 99.13876058871011310 ) ) ;
#18188 = DIRECTION ( 'NONE',  ( 0.8746197071393925215, -0.4848096202463429982, -8.676864087101708112E-18 ) ) ;
#18189 = EDGE_CURVE ( 'NONE', #3078, #21280, #19060, .T. ) ;
#18190 = CARTESIAN_POINT ( 'NONE',  ( 33.72499318558949710, 24.59184655352419213, 47.04930799450051637 ) ) ;
#18191 = CARTESIAN_POINT ( 'NONE',  ( -40.11286833322907341, 2.887657226147507306, 37.04930799450052348 ) ) ;
#18192 = EDGE_CURVE ( 'NONE', #20793, #21089, #2176, .T. ) ;
#18193 = ORIENTED_EDGE ( 'NONE', *, *, #4412, .F. ) ;
#18194 = CARTESIAN_POINT ( 'NONE',  ( 21.09992658989239089, 28.71664230456639899, 47.04930799450051637 ) ) ;
#18195 = AXIS2_PLACEMENT_3D ( 'NONE', #23661, #20711, #26284 ) ;
#18196 = DIRECTION ( 'NONE',  ( -0.000000000000000000, -1.000000000000000000, 0.000000000000000000 ) ) ;
#18197 = CARTESIAN_POINT ( 'NONE',  ( 21.09785597605719332, 13.06454579224779877, 47.04930799450051637 ) ) ;
#18198 = CARTESIAN_POINT ( 'NONE',  ( 48.94625023931840246, 26.75784706826093284, 46.10640627770148825 ) ) ;
#18199 = CIRCLE ( 'NONE', #20831, 40.00000000000000000 ) ;
#18200 = ORIENTED_EDGE ( 'NONE', *, *, #23422, .F. ) ;
#18201 = CARTESIAN_POINT ( 'NONE',  ( -41.93344242462055149, 13.82826554927147988, 59.53596428539564300 ) ) ;
#18202 = CARTESIAN_POINT ( 'NONE',  ( 21.09992658989238734, 38.56284415653841791, 47.04930799450051637 ) ) ;
#18203 = ORIENTED_EDGE ( 'NONE', *, *, #7573, .F. ) ;
#18204 = EDGE_CURVE ( 'NONE', #22382, #5329, #18566, .T. ) ;
#18205 = VERTEX_POINT ( 'NONE', #21692 ) ;
#18206 = VERTEX_POINT ( 'NONE', #31719 ) ;
#18207 = DIRECTION ( 'NONE',  ( -1.224646799147353207E-16, -1.349345573449484691E-32, 1.000000000000000000 ) ) ;
#18208 = ADVANCED_FACE ( 'NONE', ( #29246, #4466 ), #22833, .T. ) ;
#18209 = CIRCLE ( 'NONE', #22947, 2.500000000000002220 ) ;
#18210 = CARTESIAN_POINT ( 'NONE',  ( 21.09785597605719332, 25.56454579224779877, 6.862164259567697933 ) ) ;
#18211 = DIRECTION ( 'NONE',  ( 0.000000000000000000, 0.000000000000000000, 1.000000000000000000 ) ) ;
#18212 = EDGE_CURVE ( 'NONE', #19026, #23509, #9215, .T. ) ;
#18213 = AXIS2_PLACEMENT_3D ( 'NONE', #12127, #31661, #14099 ) ;
#18214 = ORIENTED_EDGE ( 'NONE', *, *, #4492, .T. ) ;
#18215 = DIRECTION ( 'NONE',  ( -1.101824276508909887E-16, 1.000000000000000000, -0.000000000000000000 ) ) ;
#18216 = AXIS2_PLACEMENT_3D ( 'NONE', #8687, #28697, #1279 ) ;
#18217 = DIRECTION ( 'NONE',  ( -1.101824276508909887E-16, 1.000000000000000000, -0.000000000000000000 ) ) ;
#18218 = CARTESIAN_POINT ( 'NONE',  ( 33.50134396954522487, 28.59164230456639544, 47.04930799450051637 ) ) ;
#18219 = CYLINDRICAL_SURFACE ( 'NONE', #25405, 2.500000000000002220 ) ;
#18220 = DIRECTION ( 'NONE',  ( -1.101824276508909887E-16, 1.000000000000000000, -0.000000000000000000 ) ) ;
#18221 = VECTOR ( 'NONE', #10252, 1000.000000000000000 ) ;
#18222 = CARTESIAN_POINT ( 'NONE',  ( -41.01929587258828747, 9.401204285752060130, 39.44930799450052206 ) ) ;
#18223 = CARTESIAN_POINT ( 'NONE',  ( -40.59758774925371938, 7.567737757495682338, 35.64930799450052490 ) ) ;
#18224 = B_SPLINE_SURFACE_WITH_KNOTS ( 'NONE', 3, 1, ( 
 ( #3209, #6009 ),
 ( #10623, #15686 ),
 ( #595, #426 ),
 ( #28008, #13080 ),
 ( #23400, #8470 ),
 ( #13405, #10782 ) ),
 .UNSPECIFIED., .F., .F., .F.,
 ( 4, 1, 1, 4 ),
 ( 2, 2 ),
 ( 0.1800733115436725096, 0.3950736110976382220, 0.6810807126490734387, 1.000000000000000000 ),
 ( 0.000000000000000000, 1.000000000000000000 ),
 .UNSPECIFIED. ) ;
#18225 = CARTESIAN_POINT ( 'NONE',  ( 46.31735793284625657, 25.18224532316113340, 44.64096519649219630 ) ) ;
#18226 = DIRECTION ( 'NONE',  ( 0.9612616959383221138, 0.2756373558169876170, 0.000000000000000000 ) ) ;
#18227 = EDGE_CURVE ( 'NONE', #24923, #23976, #24936, .T. ) ;
#18228 = ORIENTED_EDGE ( 'NONE', *, *, #12660, .F. ) ;
#18229 = ORIENTED_EDGE ( 'NONE', *, *, #26893, .T. ) ;
#18230 = CARTESIAN_POINT ( 'NONE',  ( 21.09992658989239089, 26.84164230456639899, 47.04930799450051637 ) ) ;
#18231 = CARTESIAN_POINT ( 'NONE',  ( 8.823575513742486720, 34.59164230456639899, 46.72789464899623368 ) ) ;
#18232 = FACE_OUTER_BOUND ( 'NONE', #19929, .T. ) ;
#18233 = VERTEX_POINT ( 'NONE', #15133 ) ;
#18234 = FACE_OUTER_BOUND ( 'NONE', #15552, .T. ) ;
#18235 = CARTESIAN_POINT ( 'NONE',  ( -40.23847961986563604, 6.935107571023907624, 39.46426056150422568 ) ) ;
#18236 = ORIENTED_EDGE ( 'NONE', *, *, #29391, .T. ) ;
#18237 = DIRECTION ( 'NONE',  ( 0.000000000000000000, 0.000000000000000000, -1.000000000000000000 ) ) ;
#18238 = CARTESIAN_POINT ( 'NONE',  ( 48.18662509608405031, 28.68284706826092290, 49.18364984542562013 ) ) ;
#18239 = CARTESIAN_POINT ( 'NONE',  ( 47.20547626766766314, 28.88791119454915091, 44.97710074790751378 ) ) ;
#18240 = CONICAL_SURFACE ( 'NONE', #5672, 12.00000000000000355, 0.7853981633974466137 ) ;
#18241 = CARTESIAN_POINT ( 'NONE',  ( -35.36827084435264368, 10.42249571538224906, 52.09578328476275288 ) ) ;
#18242 = AXIS2_PLACEMENT_3D ( 'NONE', #5495, #23212, #728 ) ;
#18243 = VECTOR ( 'NONE', #24714, 1000.000000000000000 ) ;
#18244 = ADVANCED_FACE ( 'NONE', ( #25141 ), #30636, .T. ) ;
#18245 = EDGE_CURVE ( 'NONE', #11490, #30019, #10806, .T. ) ;
#18246 = CIRCLE ( 'NONE', #21380, 2.500000000000002220 ) ;
#18247 = EDGE_LOOP ( 'NONE', ( #12965, #18063, #20271, #19964 ) ) ;
#18248 = DIRECTION ( 'NONE',  ( -1.000000000000000000, 0.000000000000000000, 0.000000000000000000 ) ) ;
#18249 = CARTESIAN_POINT ( 'NONE',  ( 8.698509210239528500, 26.34164230456639899, 47.04930799450051637 ) ) ;
#18250 = ADVANCED_FACE ( 'NONE', ( #24817 ), #27765, .T. ) ;
#18251 = ORIENTED_EDGE ( 'NONE', *, *, #9164, .T. ) ;
#18252 = ADVANCED_FACE ( 'NONE', ( #17422 ), #2656, .T. ) ;
#18253 = CARTESIAN_POINT ( 'NONE',  ( -43.64647580959332629, 1.256990871545142774, 60.44930799450051495 ) ) ;
#18254 = FACE_OUTER_BOUND ( 'NONE', #20674, .T. ) ;
#18255 = CARTESIAN_POINT ( 'NONE',  ( 8.474859994195282908, 38.56284415653841791, 47.04930799450051637 ) ) ;
#18256 = TOROIDAL_SURFACE ( 'NONE', #13038, 54.10000000000000142, 0.1999999999999993727 ) ;
#18257 = TOROIDAL_SURFACE ( 'NONE', #4120, 55.59552431147871232, 0.3000000000000000444 ) ;
#18258 = EDGE_LOOP ( 'NONE', ( #3724, #24989 ) ) ;
#18259 = CARTESIAN_POINT ( 'NONE',  ( -41.08785830660042393, 9.277514380576530328, 38.60788663826321709 ) ) ;
#18260 = AXIS2_PLACEMENT_3D ( 'NONE', #11030, #3628, #30891 ) ;
#18261 = CARTESIAN_POINT ( 'NONE',  ( 8.732853799281734553, 38.56284415653841791, 47.04930799450051637 ) ) ;
#18262 = FACE_OUTER_BOUND ( 'NONE', #18972, .T. ) ;
#18263 =( BOUNDED_CURVE ( )  B_SPLINE_CURVE ( 2, ( #18722, #28928, #6757, #11204, #26131, #8895, #16439, #23827, #9057 ),
 .UNSPECIFIED., .F., .F. ) 
 B_SPLINE_CURVE_WITH_KNOTS ( ( 3, 2, 2, 2, 3 ),
 ( 0.1785714297327012090, 0.1904761904761904656, 0.2142857142857142738, 0.2380952380952380820, 0.2500000011612727446 ),
 .UNSPECIFIED. ) 
 CURVE ( )  GEOMETRIC_REPRESENTATION_ITEM ( )  RATIONAL_B_SPLINE_CURVE ( ( 0.9330127018922200755, 0.9330127084266228721, 1.000000000000000000, 0.8660254037844388186, 1.000000000000000000, 0.8660254037844388186, 1.000000000000000000, 0.9330126953578155025, 0.9330127018922200755 ) ) 
 REPRESENTATION_ITEM ( '' )  );
#18264 = AXIS2_PLACEMENT_3D ( 'NONE', #19611, #17314, #31937 ) ;
#18265 = CARTESIAN_POINT ( 'NONE',  ( -0.6890700258440008996, 11.83483724345209787, -4.439927286363037240 ) ) ;
#18266 =( LENGTH_UNIT ( ) NAMED_UNIT ( * ) SI_UNIT ( .MILLI., .METRE. ) );
#18267 = VERTEX_POINT ( 'NONE', #10212 ) ;
#18268 = CARTESIAN_POINT ( 'NONE',  ( 21.09992658989239089, 25.47145308207319303, 47.04930799450051637 ) ) ;
#18269 = FACE_OUTER_BOUND ( 'NONE', #12244, .T. ) ;
#18270 = DIRECTION ( 'NONE',  ( 0.000000000000000000, -0.000000000000000000, -1.000000000000000000 ) ) ;
#18271 = DIRECTION ( 'NONE',  ( -1.000000000000000000, 0.000000000000000000, 0.000000000000000000 ) ) ;
#18272 = AXIS2_PLACEMENT_3D ( 'NONE', #3788, #31370, #28585 ) ;
#18273 = FACE_OUTER_BOUND ( 'NONE', #32298, .T. ) ;
#18274 = VERTEX_POINT ( 'NONE', #22503 ) ;
#18275 = CARTESIAN_POINT ( 'NONE',  ( 47.34970371437788828, 29.61382036679943752, 45.01289284012537451 ) ) ;
#18276 = CARTESIAN_POINT ( 'NONE',  ( 21.09992658989239089, 24.59164230456639544, 47.04930799450051637 ) ) ;
#18277 = DIRECTION ( 'NONE',  ( 1.188208965918164993E-16, 1.880121038077812639E-16, 1.000000000000000000 ) ) ;
#18278 = ORIENTED_EDGE ( 'NONE', *, *, #24308, .T. ) ;
#18279 = DIRECTION ( 'NONE',  ( 0.9996573249755574819, 1.344306794811909066E-16, 0.02617694830786587365 ) ) ;
#18280 = PLANE ( 'NONE',  #6795 ) ;
#18281 = DIRECTION ( 'NONE',  ( 0.000000000000000000, -0.000000000000000000, -1.000000000000000000 ) ) ;
#18282 = CARTESIAN_POINT ( 'NONE',  ( 53.85605973735868446, 1.102830191789100578, -6.363064465152523219 ) ) ;
#18283 = ORIENTED_EDGE ( 'NONE', *, *, #15631, .T. ) ;
#18284 = FACE_OUTER_BOUND ( 'NONE', #23199, .T. ) ;
#18285 = ORIENTED_EDGE ( 'NONE', *, *, #11572, .F. ) ;
#18286 = ADVANCED_FACE ( 'NONE', ( #12687 ), #28551, .T. ) ;
#18287 = AXIS2_PLACEMENT_3D ( 'NONE', #17207, #27225, #13961 ) ;
#18288 = VECTOR ( 'NONE', #26000, 1000.000000000000000 ) ;
#18289 = EDGE_CURVE ( 'NONE', #3113, #10702, #12294, .T. ) ;
#18290 = EDGE_LOOP ( 'NONE', ( #5220, #7316, #6495, #11373 ) ) ;
#18291 = ADVANCED_FACE ( 'NONE', ( #2171 ), #30234, .F. ) ;
#18292 = AXIS2_PLACEMENT_3D ( 'NONE', #22963, #22648, #20185 ) ;
#18293 = ADVANCED_FACE ( 'NONE', ( #7744, #17743 ), #29744, .T. ) ;
#18294 = AXIS2_PLACEMENT_3D ( 'NONE', #29401, #19203, #29230 ) ;
#18295 = DIRECTION ( 'NONE',  ( -1.000000000000000000, 0.000000000000000000, 0.000000000000000000 ) ) ;
#18296 = CARTESIAN_POINT ( 'NONE',  ( -42.50084779003665147, 14.56798984196178637, 37.04930799450052348 ) ) ;
#18297 = CARTESIAN_POINT ( 'NONE',  ( 46.55854765242722948, 27.14696019071910982, 44.51792966461572831 ) ) ;
#18298 = VERTEX_POINT ( 'NONE', #29915 ) ;
#18299 = CARTESIAN_POINT ( 'NONE',  ( -40.54828680531408480, 6.846271790121642553, 34.54930799450052348 ) ) ;
#18300 = ORIENTED_EDGE ( 'NONE', *, *, #14028, .T. ) ;
#18301 = DIRECTION ( 'NONE',  ( 0.000000000000000000, 0.000000000000000000, -1.000000000000000000 ) ) ;
#18302 = CARTESIAN_POINT ( 'NONE',  ( 47.09785597605719687, 29.86454579224779948, 47.04930799450078638 ) ) ;
#18303 = CARTESIAN_POINT ( 'NONE',  ( -30.33793827003903232, 10.49391138527215084, 72.64809877684305661 ) ) ;
#18304 = LINE ( 'NONE', #10785, #17339 ) ;
#18305 = ORIENTED_EDGE ( 'NONE', *, *, #13469, .T. ) ;
#18306 = DIRECTION ( 'NONE',  ( -1.101824276508909887E-16, 1.000000000000000000, -0.000000000000000000 ) ) ;
#18307 = VERTEX_POINT ( 'NONE', #9724 ) ;
#18308 = DIRECTION ( 'NONE',  ( 0.000000000000000000, 0.000000000000000000, 1.000000000000000000 ) ) ;
#18309 = CARTESIAN_POINT ( 'NONE',  ( -40.60722745863126448, 9.415333058485025219, 39.40788663826321425 ) ) ;
#18310 = CIRCLE ( 'NONE', #9391, 0.09999999999999795164 ) ;
#18311 = ORIENTED_EDGE ( 'NONE', *, *, #18853, .F. ) ;
#18312 = CARTESIAN_POINT ( 'NONE',  ( 8.482002859293448438, 28.96664230456639899, 47.04930799450051637 ) ) ;
#18313 = CIRCLE ( 'NONE', #28792, 19.50000000000000000 ) ;
#18314 = CARTESIAN_POINT ( 'NONE',  ( -36.17180646779264919, 10.42241829745360526, 52.09577041703580846 ) ) ;
#18315 = CYLINDRICAL_SURFACE ( 'NONE', #1576, 0.1000000000000014905 ) ;
#18316 = CARTESIAN_POINT ( 'NONE',  ( 21.09785597605719332, 30.56454579224779522, 70.54930799450050927 ) ) ;
#18317 = CARTESIAN_POINT ( 'NONE',  ( -42.36153388572594736, 13.68895619636815653, 60.54930799450051637 ) ) ;
#18318 = ORIENTED_EDGE ( 'NONE', *, *, #22746, .T. ) ;
#18319 = CARTESIAN_POINT ( 'NONE',  ( -42.47434154250543514, 4.196643200812633978, 38.34930799450052064 ) ) ;
#18320 = CARTESIAN_POINT ( 'NONE',  ( -40.62190982259030392, 6.851786633711440366, 34.76984793051720857 ) ) ;
#18321 = ORIENTED_EDGE ( 'NONE', *, *, #2994, .F. ) ;
#18322 = DIRECTION ( 'NONE',  ( -1.224646799147353207E-16, -1.349345573449484691E-32, 1.000000000000000000 ) ) ;
#18323 = AXIS2_PLACEMENT_3D ( 'NONE', #21176, #31219, #26599 ) ;
#18324 = AXIS2_PLACEMENT_3D ( 'NONE', #9253, #21223, #24018 ) ;
#18325 = CARTESIAN_POINT ( 'NONE',  ( -9.880269303432738681, -5.935454207752202116, -13.32263710021335612 ) ) ;
#18326 = ORIENTED_EDGE ( 'NONE', *, *, #31424, .F. ) ;
#18327 = TOROIDAL_SURFACE ( 'NONE', #11511, 12.61792373059891226, 0.1250000000000024980 ) ;
#18328 = EDGE_LOOP ( 'NONE', ( #26944, #19399, #10650, #30819 ) ) ;
#18329 = CARTESIAN_POINT ( 'NONE',  ( 21.09992658989238734, 38.56284415653841791, 47.04930799450051637 ) ) ;
#18330 = AXIS2_PLACEMENT_3D ( 'NONE', #13384, #20909, #30457 ) ;
#18331 = ORIENTED_EDGE ( 'NONE', *, *, #19013, .T. ) ;
#18332 = AXIS2_PLACEMENT_3D ( 'NONE', #31601, #11404, #21245 ) ;
#18333 = AXIS2_PLACEMENT_3D ( 'NONE', #6120, #25818, #11059 ) ;
#18334 = ADVANCED_FACE ( 'NONE', ( #19717 ), #2491, .F. ) ;
#18335 = EDGE_CURVE ( 'NONE', #17767, #30606, #6769, .T. ) ;
#18336 = EDGE_CURVE ( 'NONE', #3463, #253, #6089, .T. ) ;
#18337 = ORIENTED_EDGE ( 'NONE', *, *, #11222, .F. ) ;
#18338 = FACE_OUTER_BOUND ( 'NONE', #12593, .T. ) ;
#18339 = CIRCLE ( 'NONE', #29895, 1.199999999999999734 ) ;
#18340 = VECTOR ( 'NONE', #28087, 1000.000000000000000 ) ;
#18341 = ORIENTED_EDGE ( 'NONE', *, *, #13179, .F. ) ;
#18342 = CARTESIAN_POINT ( 'NONE',  ( 47.09785597605719687, 23.12036939723557083, 47.04930799450080059 ) ) ;
#18343 = CIRCLE ( 'NONE', #3140, 0.1250000000000001110 ) ;
#18344 = CARTESIAN_POINT ( 'NONE',  ( 49.58529161108529593, 29.18166210836908547, 47.08701687824213167 ) ) ;
#18345 = DIRECTION ( 'NONE',  ( 0.000000000000000000, 0.000000000000000000, 1.000000000000000000 ) ) ;
#18346 = CARTESIAN_POINT ( 'NONE',  ( 45.81741271322955100, 26.40122849631043422, 49.02305402274571122 ) ) ;
#18347 = AXIS2_PLACEMENT_3D ( 'NONE', #27031, #14892, #10296 ) ;
#18348 = ORIENTED_EDGE ( 'NONE', *, *, #28913, .T. ) ;
#18349 = ORIENTED_EDGE ( 'NONE', *, *, #29393, .T. ) ;
#18350 = EDGE_LOOP ( 'NONE', ( #26357, #12426 ) ) ;
#18351 = DIRECTION ( 'NONE',  ( 0.8746197071393927436, -0.4848096202463423876, -1.277302113040827440E-17 ) ) ;
#18352 = LINE ( 'NONE', #805, #21757 ) ;
#18353 = CARTESIAN_POINT ( 'NONE',  ( 33.37634396954525329, 26.34164230456639899, 47.04930799450051637 ) ) ;
#18354 = CARTESIAN_POINT ( 'NONE',  ( 0.4108105365410483212, 11.92558985988973497, -5.698108176600966246 ) ) ;
#18355 = DIRECTION ( 'NONE',  ( -0.000000000000000000, 1.000000000000000000, -0.000000000000000000 ) ) ;
#18356 = ORIENTED_EDGE ( 'NONE', *, *, #27262, .T. ) ;
#18357 = CARTESIAN_POINT ( 'NONE',  ( 8.482002859293777064, 30.96664230456641675, 47.04930799450051637 ) ) ;
#18358 = DIRECTION ( 'NONE',  ( 0.000000000000000000, 0.000000000000000000, -1.000000000000000000 ) ) ;
#18359 = CARTESIAN_POINT ( 'NONE',  ( -9.847437802426064479, -5.936463391119989552, 107.4980644588596874 ) ) ;
#18360 = CARTESIAN_POINT ( 'NONE',  ( -40.23672901771082877, 7.760455916344221272, 39.54930799450052348 ) ) ;
#18361 = ORIENTED_EDGE ( 'NONE', *, *, #10158, .F. ) ;
#18362 = CARTESIAN_POINT ( 'NONE',  ( 8.823509210239542710, 27.59164230456639544, 47.04930799450051637 ) ) ;
#18363 = DIRECTION ( 'NONE',  ( -0.000000000000000000, -1.000000000000000000, 0.000000000000000000 ) ) ;
#18364 = EDGE_CURVE ( 'NONE', #6807, #22128, #10729, .T. ) ;
#18365 = CIRCLE ( 'NONE', #25716, 39.50000000000000000 ) ;
#18366 = ORIENTED_EDGE ( 'NONE', *, *, #14312, .T. ) ;
#18367 = AXIS2_PLACEMENT_3D ( 'NONE', #16570, #26590, #4100 ) ;
#18368 = AXIS2_PLACEMENT_3D ( 'NONE', #27850, #20932, #30964 ) ;
#18369 = AXIS2_PLACEMENT_3D ( 'NONE', #2948, #27585, #28072 ) ;
#18370 = VECTOR ( 'NONE', #8486, 1000.000000000000000 ) ;
#18371 = ORIENTED_EDGE ( 'NONE', *, *, #27675, .T. ) ;
#18372 = ADVANCED_FACE ( 'NONE', ( #677 ), #8552, .T. ) ;
#18373 = ADVANCED_FACE ( 'NONE', ( #30880 ), #14393, .T. ) ;
#18374 = EDGE_CURVE ( 'NONE', #28560, #22190, #20151, .T. ) ;
#18375 = VERTEX_POINT ( 'NONE', #506 ) ;
#18376 = EDGE_CURVE ( 'NONE', #14105, #13215, #4471, .T. ) ;
#18377 = CARTESIAN_POINT ( 'NONE',  ( 21.09785597605720042, -13.68834655544033652, -8.644984113562347972 ) ) ;
#18378 = DIRECTION ( 'NONE',  ( -1.000000000000000000, -1.101824276508909887E-16, 0.000000000000000000 ) ) ;
#18379 = DIRECTION ( 'NONE',  ( -1.188208965918165239E-16, -1.880121038077813132E-16, -1.000000000000000000 ) ) ;
#18380 = AXIS2_PLACEMENT_3D ( 'NONE', #7018, #11784, #17012 ) ;
#18381 = EDGE_LOOP ( 'NONE', ( #32134, #17171 ) ) ;
#18382 = CARTESIAN_POINT ( 'NONE',  ( -41.59479728461646175, 12.46621001045476973, 57.04930799450051637 ) ) ;
#18383 = CARTESIAN_POINT ( 'NONE',  ( 21.09785597605719687, 16.33322284159648063, 94.44875166441873660 ) ) ;
#18384 = DIRECTION ( 'NONE',  ( 0.000000000000000000, -1.000000000000000000, -0.000000000000000000 ) ) ;
#18385 = EDGE_LOOP ( 'NONE', ( #27998, #27064, #24776, #27903 ) ) ;
#18386 = FACE_OUTER_BOUND ( 'NONE', #13072, .T. ) ;
#18387 = ORIENTED_EDGE ( 'NONE', *, *, #16112, .F. ) ;
#18388 = CARTESIAN_POINT ( 'NONE',  ( -41.94323192092819852, 13.80701548633532560, 59.54475713566544215 ) ) ;
#18389 = FACE_OUTER_BOUND ( 'NONE', #25105, .T. ) ;
#18390 = CARTESIAN_POINT ( 'NONE',  ( 45.99457799031791438, 29.23661293962803143, 44.88652376508412090 ) ) ;
#18391 = CARTESIAN_POINT ( 'NONE',  ( 21.09992658989239089, 23.59164230456639544, 47.04930799450051637 ) ) ;
#18392 = CIRCLE ( 'NONE', #28368, 12.36707279061065101 ) ;
#18393 = CARTESIAN_POINT ( 'NONE',  ( -40.65487266620045403, 9.475231293617264683, 38.63717596014456035 ) ) ;
#18394 = AXIS2_PLACEMENT_3D ( 'NONE', #26997, #27645, #12232 ) ;
#18395 = ORIENTED_EDGE ( 'NONE', *, *, #7539, .F. ) ;
#18396 = ORIENTED_EDGE ( 'NONE', *, *, #30539, .T. ) ;
#18397 = CARTESIAN_POINT ( 'NONE',  ( 65.47508102033168598, -13.30632128221581212, 81.09457859485948461 ) ) ;
#18398 = AXIS2_PLACEMENT_3D ( 'NONE', #1363, #28778, #6620 ) ;
#18399 = DIRECTION ( 'NONE',  ( 0.8746197071393926326, -0.4848096202463430537, -8.676864087101709653E-18 ) ) ;
#18400 = B_SPLINE_CURVE_WITH_KNOTS ( 'NONE', 3,
 ( #10360, #12833, #5922, #828, #27755, #15593, #15924, #25929, #3446, #20354, #27921, #5438 ),
 .UNSPECIFIED., .F., .F.,
 ( 4, 2, 2, 2, 2, 4 ),
 ( 0.0002033792717032385539, 0.0008000624350769520434, 0.001396745598450665560, 0.001993428761824378968, 0.002291770343511237949, 0.002590111925198097364 ),
 .UNSPECIFIED. ) ;
#18401 = DIRECTION ( 'NONE',  ( -1.000000000000000000, 0.000000000000000000, 0.000000000000000000 ) ) ;
#18402 = ORIENTED_EDGE ( 'NONE', *, *, #1927, .T. ) ;
#18403 = DIRECTION ( 'NONE',  ( -1.000000000000000000, 0.000000000000000000, 0.000000000000000000 ) ) ;
#18404 = DIRECTION ( 'NONE',  ( -7.588956326749211550E-18, 4.206627182996911684E-18, -1.000000000000000000 ) ) ;
#18405 = VERTEX_POINT ( 'NONE', #27928 ) ;
#18406 = CARTESIAN_POINT ( 'NONE',  ( 49.28428300279882990, 29.04787913140503974, 48.46772541801551171 ) ) ;
#18407 = ADVANCED_FACE ( 'NONE', ( #8391 ), #30393, .F. ) ;
#18408 = AXIS2_PLACEMENT_3D ( 'NONE', #2970, #12521, #2336 ) ;
#18409 = EDGE_CURVE ( 'NONE', #28788, #14105, #5448, .T. ) ;
#18410 = CARTESIAN_POINT ( 'NONE',  ( 33.46699938050304723, 26.22145308207318593, 47.04930799450050927 ) ) ;
#18411 = ORIENTED_EDGE ( 'NONE', *, *, #27802, .T. ) ;
#18412 = CIRCLE ( 'NONE', #5853, 13.50178401536290984 ) ;
#18413 = VECTOR ( 'NONE', #13896, 1000.000000000000000 ) ;
#18414 = VECTOR ( 'NONE', #7436, 1000.000000000000000 ) ;
#18415 = EDGE_CURVE ( 'NONE', #32106, #2831, #21009, .T. ) ;
#18416 = DIRECTION ( 'NONE',  ( 0.4848096202463424431, 0.8746197071393927436, -2.220446049250312588E-16 ) ) ;
#18417 = CARTESIAN_POINT ( 'NONE',  ( -42.38687957179150345, 4.148162238788003719, 58.34930799450052064 ) ) ;
#18418 = EDGE_LOOP ( 'NONE', ( #21051, #29314, #30297, #12677 ) ) ;
#18419 = DIRECTION ( 'NONE',  ( 0.2756373558169932236, -0.9612616959383204485, 1.479773560108267395E-16 ) ) ;
#18420 = CARTESIAN_POINT ( 'NONE',  ( 48.34748475735720774, 24.70653309617948423, 49.49898713858203791 ) ) ;
#18421 = AXIS2_PLACEMENT_3D ( 'NONE', #24214, #3870, #1235 ) ;
#18422 = CARTESIAN_POINT ( 'NONE',  ( 72.97689775927815958, 2.854128177266946675, 15.17817617591508395 ) ) ;
#18423 = ORIENTED_EDGE ( 'NONE', *, *, #3933, .T. ) ;
#18424 = DIRECTION ( 'NONE',  ( -0.4441739386572048365, -0.2110602665713104675, -0.8707256032141199587 ) ) ;
#18425 = CARTESIAN_POINT ( 'NONE',  ( 46.86318297022563684, 10.39302479005550062, 97.56778208447272505 ) ) ;
#18426 = CARTESIAN_POINT ( 'NONE',  ( 33.72499318558949710, 25.34143805560860940, 47.04930799450051637 ) ) ;
#18427 = EDGE_CURVE ( 'NONE', #21045, #21064, #29074, .T. ) ;
#18428 = CARTESIAN_POINT ( 'NONE',  ( 0.4110235620567528891, 11.92558985988973497, -4.837558254760519816 ) ) ;
#18429 = ORIENTED_EDGE ( 'NONE', *, *, #19745, .T. ) ;
#18430 = CARTESIAN_POINT ( 'NONE',  ( 46.54440680854508372, 23.10527865767145173, 46.85395460512839350 ) ) ;
#18431 = DIRECTION ( 'NONE',  ( 0.8746197071393858602, -0.4848096202463547666, 0.000000000000000000 ) ) ;
#18432 = FACE_OUTER_BOUND ( 'NONE', #16366, .T. ) ;
#18433 = ADVANCED_FACE ( 'NONE', ( #16089 ), #16994, .T. ) ;
#18434 = CARTESIAN_POINT ( 'NONE',  ( 21.09992658989238734, 38.56284415653841791, 47.04930799450051637 ) ) ;
#18435 = AXIS2_PLACEMENT_3D ( 'NONE', #24952, #8047, #2464 ) ;
#18436 = DIRECTION ( 'NONE',  ( -1.000000000000000000, 0.000000000000000000, 0.000000000000000000 ) ) ;
#18437 = AXIS2_PLACEMENT_3D ( 'NONE', #26698, #14075, #24070 ) ;
#18438 = VERTEX_POINT ( 'NONE', #3619 ) ;
#18439 = CIRCLE ( 'NONE', #13748, 0.1999999999999987899 ) ;
#18440 = DIRECTION ( 'NONE',  ( -1.000000000000000000, 0.000000000000000000, 0.000000000000000000 ) ) ;
#18441 = DIRECTION ( 'NONE',  ( -1.101824276508909887E-16, 1.000000000000000000, -0.000000000000000000 ) ) ;
#18442 = LINE ( 'NONE', #20750, #22737 ) ;
#18443 = ORIENTED_EDGE ( 'NONE', *, *, #20720, .T. ) ;
#18444 = CYLINDRICAL_SURFACE ( 'NONE', #15230, 12.62506659569710266 ) ;
#18445 = DIRECTION ( 'NONE',  ( -1.101824276508909887E-16, 1.000000000000000000, -0.000000000000000000 ) ) ;
#18446 = EDGE_CURVE ( 'NONE', #4539, #24404, #19096, .T. ) ;
#18447 = EDGE_CURVE ( 'NONE', #14944, #31146, #3915, .T. ) ;
#18448 = CARTESIAN_POINT ( 'NONE',  ( 21.09785597605719332, 25.56454579224779167, 47.04930799450051637 ) ) ;
#18449 = DIRECTION ( 'NONE',  ( -0.000000000000000000, -1.000000000000000000, -0.000000000000000000 ) ) ;
#18450 = ADVANCED_FACE ( 'NONE', ( #20362 ), #8120, .F. ) ;
#18451 = EDGE_LOOP ( 'NONE', ( #25416, #31587, #29696, #29385 ) ) ;
#18452 = CARTESIAN_POINT ( 'NONE',  ( 8.474859994195259816, 23.84143805560861296, 47.04930799450051637 ) ) ;
#18453 = EDGE_LOOP ( 'NONE', ( #8453, #30088 ) ) ;
#18454 = AXIS2_PLACEMENT_3D ( 'NONE', #22726, #15503, #12897 ) ;
#18455 = VERTEX_POINT ( 'NONE', #30561 ) ;
#18456 = AXIS2_PLACEMENT_3D ( 'NONE', #24484, #1677, #31878 ) ;
#18457 = EDGE_CURVE ( 'NONE', #1878, #13269, #5829, .T. ) ;
#18458 = AXIS2_PLACEMENT_3D ( 'NONE', #13600, #640, #10672 ) ;
#18459 = AXIS2_PLACEMENT_3D ( 'NONE', #14913, #19989, #17851 ) ;
#18460 = CARTESIAN_POINT ( 'NONE',  ( 45.96182992765471909, 27.87822092656774231, 44.82232689504102296 ) ) ;
#18461 = DIRECTION ( 'NONE',  ( 1.000000000000000000, 0.000000000000000000, 1.900504084856170908E-16 ) ) ;
#18462 = DIRECTION ( 'NONE',  ( -1.000000000000000000, 0.000000000000000000, 0.000000000000000000 ) ) ;
#18463 = ORIENTED_EDGE ( 'NONE', *, *, #11202, .T. ) ;
#18464 = CARTESIAN_POINT ( 'NONE',  ( -42.59587854516874472, -0.7667456371672803916, 32.14930799450051779 ) ) ;
#18465 = ORIENTED_EDGE ( 'NONE', *, *, #7462, .F. ) ;
#18466 = CARTESIAN_POINT ( 'NONE',  ( 21.09785597605719332, 12.11061942510878886, 47.04930799450051637 ) ) ;
#18467 = DIRECTION ( 'NONE',  ( 0.4848096202463430537, 0.8746197071393926326, 1.323854077651070671E-16 ) ) ;
#18468 = CARTESIAN_POINT ( 'NONE',  ( -33.88509152296665405, -2.225152678231165027, 80.77477800364387406 ) ) ;
#18469 = EDGE_CURVE ( 'NONE', #17152, #3515, #7612, .T. ) ;
#18470 = CARTESIAN_POINT ( 'NONE',  ( 21.09785597605719332, -9.935454207752199451, 119.0493079945005093 ) ) ;
#18471 = EDGE_LOOP ( 'NONE', ( #29924, #22900, #21869, #23743 ) ) ;
#18472 = FACE_OUTER_BOUND ( 'NONE', #21614, .T. ) ;
#18473 = DIRECTION ( 'NONE',  ( -0.000000000000000000, 1.000000000000000000, -0.000000000000000000 ) ) ;
#18474 = DIRECTION ( 'NONE',  ( 0.000000000000000000, 0.000000000000000000, 1.000000000000000000 ) ) ;
#18475 = ORIENTED_EDGE ( 'NONE', *, *, #7124, .F. ) ;
#18476 = CARTESIAN_POINT ( 'NONE',  ( 46.74373320708509283, 22.98879437201065912, 45.62408745049495451 ) ) ;
#18477 = EDGE_CURVE ( 'NONE', #23177, #6352, #29605, .T. ) ;
#18478 = DIRECTION ( 'NONE',  ( -7.588956326749211550E-18, 4.206627182996912454E-18, -1.000000000000000000 ) ) ;
#18479 = DIRECTION ( 'NONE',  ( 0.9612616959383205595, 0.2756373558169932236, -1.660411357259282445E-16 ) ) ;
#18480 = CIRCLE ( 'NONE', #2750, 0.1250000000000001110 ) ;
#18481 = DIRECTION ( 'NONE',  ( -2.779292025043186357E-18, 1.288349127009862211E-17, -1.000000000000000000 ) ) ;
#18482 = ORIENTED_EDGE ( 'NONE', *, *, #16074, .F. ) ;
#18483 = CARTESIAN_POINT ( 'NONE',  ( 21.09785597605719332, 24.86454579224779948, 18.54930799450050927 ) ) ;
#18484 = CARTESIAN_POINT ( 'NONE',  ( -40.59758774925372649, 7.567737757495682338, 35.43807061034478778 ) ) ;
#18485 = AXIS2_PLACEMENT_3D ( 'NONE', #5766, #22989, #20533 ) ;
#18486 = VERTEX_POINT ( 'NONE', #2083 ) ;
#18487 = DIRECTION ( 'NONE',  ( -1.101824276508909887E-16, 1.000000000000000000, -0.000000000000000000 ) ) ;
#18488 = EDGE_CURVE ( 'NONE', #25031, #20784, #23317, .T. ) ;
#18489 = DIRECTION ( 'NONE',  ( -1.101824276508909887E-16, 1.000000000000000000, -0.000000000000000000 ) ) ;
#18490 = EDGE_CURVE ( 'NONE', #14332, #9808, #23647, .T. ) ;
#18491 = ORIENTED_EDGE ( 'NONE', *, *, #28279, .T. ) ;
#18492 = AXIS2_PLACEMENT_3D ( 'NONE', #11597, #9290, #19458 ) ;
#18493 = VERTEX_POINT ( 'NONE', #9481 ) ;
#18494 = DIRECTION ( 'NONE',  ( -1.101824276508909887E-16, 1.000000000000000000, -0.000000000000000000 ) ) ;
#18495 = ORIENTED_EDGE ( 'NONE', *, *, #16036, .F. ) ;
#18496 = VECTOR ( 'NONE', #13606, 1000.000000000000114 ) ;
#18497 = VERTEX_POINT ( 'NONE', #19145 ) ;
#18498 = AXIS2_PLACEMENT_3D ( 'NONE', #1427, #26219, #3735 ) ;
#18499 = CARTESIAN_POINT ( 'NONE',  ( -42.50976151518963064, 14.59907569580870046, 37.04930799450052348 ) ) ;
#18500 = ORIENTED_EDGE ( 'NONE', *, *, #27912, .T. ) ;
#18501 = CARTESIAN_POINT ( 'NONE',  ( 47.74276738922625896, 23.04411657098542321, 47.98391173131702914 ) ) ;
#18502 = AXIS2_PLACEMENT_3D ( 'NONE', #10279, #24718, #2229 ) ;
#18503 = CIRCLE ( 'NONE', #16396, 43.50000000000000000 ) ;
#18504 = DIRECTION ( 'NONE',  ( 1.000000000000000000, 0.000000000000000000, 0.000000000000000000 ) ) ;
#18505 = CARTESIAN_POINT ( 'NONE',  ( 8.474859994195281132, 38.56284415653841791, 47.04930799450051637 ) ) ;
#18506 = CARTESIAN_POINT ( 'NONE',  ( 45.28286642839709231, 25.64289516297710847, 47.97516931882780966 ) ) ;
#18507 = ORIENTED_EDGE ( 'NONE', *, *, #22444, .F. ) ;
#18508 = ORIENTED_EDGE ( 'NONE', *, *, #6896, .T. ) ;
#18509 = ORIENTED_EDGE ( 'NONE', *, *, #30868, .F. ) ;
#18510 = DIRECTION ( 'NONE',  ( -0.2756373558169932236, 0.9612616959383204485, -1.479773560108267395E-16 ) ) ;
#18511 = CARTESIAN_POINT ( 'NONE',  ( 53.12892922725793454, 2.565965067347319550, 99.95503537435618568 ) ) ;
#18512 = DIRECTION ( 'NONE',  ( 1.000000000000000000, 0.000000000000000000, 0.000000000000000000 ) ) ;
#18513 = CARTESIAN_POINT ( 'NONE',  ( -39.55402147699608406, 7.608641254004257171, 32.04930799450052348 ) ) ;
#18514 = ORIENTED_EDGE ( 'NONE', *, *, #8844, .T. ) ;
#18515 = DIRECTION ( 'NONE',  ( -1.224646799147353207E-16, -1.349345573449484691E-32, 1.000000000000000000 ) ) ;
#18516 = CARTESIAN_POINT ( 'NONE',  ( -36.75957860043340020, -5.923061377617729661, 15.81027635050077151 ) ) ;
#18517 = DIRECTION ( 'NONE',  ( 0.9612616959383193382, 0.2756373558169973870, 8.795445018804930779E-19 ) ) ;
#18518 = EDGE_CURVE ( 'NONE', #30739, #13675, #17341, .T. ) ;
#18519 = CARTESIAN_POINT ( 'NONE',  ( 47.75295489951383132, 23.09557481883486929, 46.71512938763805067 ) ) ;
#18520 = EDGE_CURVE ( 'NONE', #3113, #18497, #14932, .T. ) ;
#18521 = DIRECTION ( 'NONE',  ( 0.000000000000000000, 0.000000000000000000, -1.000000000000000000 ) ) ;
#18522 = CIRCLE ( 'NONE', #7533, 12.36707279061065101 ) ;
#18523 = EDGE_CURVE ( 'NONE', #30888, #18712, #17007, .T. ) ;
#18524 = DIRECTION ( 'NONE',  ( -0.9612616959383200044, -0.2756373558169954996, 1.660411357259285896E-16 ) ) ;
#18525 = ORIENTED_EDGE ( 'NONE', *, *, #30991, .T. ) ;
#18526 = CARTESIAN_POINT ( 'NONE',  ( 21.09992658989239089, 27.22145308207318593, 47.04930799450051637 ) ) ;
#18527 = DIRECTION ( 'NONE',  ( -0.1949050434465271764, 0.6797146636928685925, -0.7071067811865460184 ) ) ;
#18528 = AXIS2_PLACEMENT_3D ( 'NONE', #29971, #7484, #17482 ) ;
#18529 = EDGE_LOOP ( 'NONE', ( #15929, #95, #3472, #1378 ) ) ;
#18530 = CIRCLE ( 'NONE', #7007, 0.1999999999999918510 ) ;
#18531 = AXIS2_PLACEMENT_3D ( 'NONE', #19602, #29633, #14531 ) ;
#18532 = ORIENTED_EDGE ( 'NONE', *, *, #31832, .F. ) ;
#18533 = DIRECTION ( 'NONE',  ( 0.000000000000000000, -1.000000000000000000, 0.000000000000000000 ) ) ;
#18534 = CARTESIAN_POINT ( 'NONE',  ( 21.09785597605720042, -16.63545420775220407, -23.54971151909227700 ) ) ;
#18535 = EDGE_LOOP ( 'NONE', ( #30189, #24281, #12796, #2140 ) ) ;
#18536 = CARTESIAN_POINT ( 'NONE',  ( 17.44491328785236561, -13.30632128221581212, -8.763545028782028012 ) ) ;
#18537 = CARTESIAN_POINT ( 'NONE',  ( 21.09785597605719332, 11.92558985988973497, 47.04930799450051637 ) ) ;
#18538 = DIRECTION ( 'NONE',  ( -0.000000000000000000, -1.000000000000000000, -0.000000000000000000 ) ) ;
#18539 = ORIENTED_EDGE ( 'NONE', *, *, #22018, .F. ) ;
#18540 = DIRECTION ( 'NONE',  ( 0.1949050434465252335, -0.6797146636928682595, -0.7071067811865469066 ) ) ;
#18541 = VERTEX_POINT ( 'NONE', #4385 ) ;
#18542 = CARTESIAN_POINT ( 'NONE',  ( 21.09785597605719332, -15.93545420775219945, 47.04930799450051637 ) ) ;
#18543 = CARTESIAN_POINT ( 'NONE',  ( 21.09785597605719332, -15.43545420775221366, 47.04930799450051637 ) ) ;
#18544 = CARTESIAN_POINT ( 'NONE',  ( -45.06166779280744095, -5.721341737285086992, 40.94964444931001424 ) ) ;
#18545 = DIRECTION ( 'NONE',  ( -1.000000000000000000, 0.000000000000000000, 0.000000000000000000 ) ) ;
#18546 =( LENGTH_UNIT ( ) NAMED_UNIT ( * ) SI_UNIT ( .MILLI., .METRE. ) );
#18547 = ORIENTED_EDGE ( 'NONE', *, *, #4942, .F. ) ;
#18548 = ORIENTED_EDGE ( 'NONE', *, *, #29059, .F. ) ;
#18549 = DIRECTION ( 'NONE',  ( -1.224646799147353207E-16, -1.349345573449484691E-32, 1.000000000000000000 ) ) ;
#18550 = DIRECTION ( 'NONE',  ( -1.000000000000000000, 0.000000000000000000, 0.000000000000000000 ) ) ;
#18551 = EDGE_CURVE ( 'NONE', #32344, #14664, #19621, .T. ) ;
#18552 = DIRECTION ( 'NONE',  ( -1.101824276508909887E-16, 1.000000000000000000, -0.000000000000000000 ) ) ;
#18553 = ADVANCED_FACE ( 'NONE', ( #29331 ), #13373, .T. ) ;
#18554 = EDGE_CURVE ( 'NONE', #5318, #22757, #10237, .T. ) ;
#18555 = EDGE_LOOP ( 'NONE', ( #3765, #8558, #9413, #8142 ) ) ;
#18556 = CARTESIAN_POINT ( 'NONE',  ( -41.94956971822180947, 3.905757428664828890, 47.04930799450051637 ) ) ;
#18557 = CARTESIAN_POINT ( 'NONE',  ( 46.55854765242723659, 28.54696019071910840, 44.51792966461573542 ) ) ;
#18558 = EDGE_CURVE ( 'NONE', #18497, #15900, #28566, .T. ) ;
#18559 = ORIENTED_EDGE ( 'NONE', *, *, #5225, .T. ) ;
#18560 = DIRECTION ( 'NONE',  ( -0.2756373558169932236, 0.9612616959383204485, -1.479773560108267395E-16 ) ) ;
#18561 = EDGE_CURVE ( 'NONE', #17732, #2041, #26450, .T. ) ;
#18562 = CARTESIAN_POINT ( 'NONE',  ( 44.91142894931555674, 30.09787913140503335, 45.63089057098605394 ) ) ;
#18563 = FACE_OUTER_BOUND ( 'NONE', #23453, .T. ) ;
#18564 = TOROIDAL_SURFACE ( 'NONE', #3363, 0.8928932188134564019, 0.1000000000000000056 ) ;
#18565 = VECTOR ( 'NONE', #30156, 1000.000000000000227 ) ;
#18566 = CIRCLE ( 'NONE', #21714, 0.1250000000000001110 ) ;
#18567 = AXIS2_PLACEMENT_3D ( 'NONE', #19539, #14630, #7075 ) ;
#18568 = CIRCLE ( 'NONE', #1283, 2.000000000000001776 ) ;
#18569 = ORIENTED_EDGE ( 'NONE', *, *, #10821, .T. ) ;
#18570 = CARTESIAN_POINT ( 'NONE',  ( 52.07598125402753197, -5.935454207809698346, -13.48459002699794063 ) ) ;
#18571 = CARTESIAN_POINT ( 'NONE',  ( -40.59758774925371938, 7.567737757495682338, 35.43807061034478778 ) ) ;
#18572 = DIRECTION ( 'NONE',  ( 0.000000000000000000, 0.000000000000000000, -1.000000000000000000 ) ) ;
#18573 = ORIENTED_EDGE ( 'NONE', *, *, #1294, .F. ) ;
#18574 = CARTESIAN_POINT ( 'NONE',  ( 21.09785597605719332, 30.56454579224779522, 23.54930799450051282 ) ) ;
#18575 = CARTESIAN_POINT ( 'NONE',  ( 21.09785597605720753, 15.70210863493540288, 47.04930799450052348 ) ) ;
#18576 = EDGE_CURVE ( 'NONE', #18781, #13490, #17549, .T. ) ;
#18577 = DIRECTION ( 'NONE',  ( -1.101824276508909887E-16, 1.000000000000000000, -0.000000000000000000 ) ) ;
#18578 = VERTEX_POINT ( 'NONE', #24736 ) ;
#18579 = CARTESIAN_POINT ( 'NONE',  ( -42.48178708409979265, 14.60617548783703690, 58.99727659774876543 ) ) ;
#18580 = DIRECTION ( 'NONE',  ( 0.4848096202463637039, 0.8746197071393810862, 0.000000000000000000 ) ) ;
#18581 = FACE_OUTER_BOUND ( 'NONE', #13656, .T. ) ;
#18582 = VECTOR ( 'NONE', #11659, 1000.000000000000114 ) ;
#18583 = CARTESIAN_POINT ( 'NONE',  ( 0.6836613156275018754, 1.925589859889728972, 132.0493079945005377 ) ) ;
#18584 = AXIS2_PLACEMENT_3D ( 'NONE', #26917, #14456, #11180 ) ;
#18585 = SURFACE_STYLE_FILL_AREA ( #8592 ) ;
#18586 = EDGE_LOOP ( 'NONE', ( #13695, #12984, #21094, #12732 ) ) ;
#18587 = DIRECTION ( 'NONE',  ( -1.101824276508909887E-16, 1.000000000000000000, -0.000000000000000000 ) ) ;
#18588 = CARTESIAN_POINT ( 'NONE',  ( 8.474859994195286461, 24.09143805560860940, 47.04930799450051637 ) ) ;
#18589 = CIRCLE ( 'NONE', #10256, 2.500000000000002220 ) ;
#18590 = DIRECTION ( 'NONE',  ( -1.101824276508909887E-16, 1.000000000000000000, -0.000000000000000000 ) ) ;
#18591 = DIRECTION ( 'NONE',  ( -1.101824276508909887E-16, 1.000000000000000000, -0.000000000000000000 ) ) ;
#18592 = CARTESIAN_POINT ( 'NONE',  ( 0.5978559760572086379, 13.86454579224779948, 47.04930799450052348 ) ) ;
#18593 = ORIENTED_EDGE ( 'NONE', *, *, #14359, .T. ) ;
#18594 = DIRECTION ( 'NONE',  ( 0.000000000000000000, 0.000000000000000000, -1.000000000000000000 ) ) ;
#18595 = CARTESIAN_POINT ( 'NONE',  ( 49.68037673357003570, 24.91954977745023214, 46.56884725464978203 ) ) ;
#18596 = DIRECTION ( 'NONE',  ( -0.1949050434465282311, 0.6797146636928672603, -0.7071067811865469066 ) ) ;
#18597 = ORIENTED_EDGE ( 'NONE', *, *, #23459, .F. ) ;
#18598 = DIRECTION ( 'NONE',  ( 0.3213166889719795694, -0.7071067811865470176, 0.6298853748009115572 ) ) ;
#18599 = EDGE_CURVE ( 'NONE', #3050, #13764, #15979, .T. ) ;
#18600 = DIRECTION ( 'NONE',  ( -1.101824276508909887E-16, 1.000000000000000000, -0.000000000000000000 ) ) ;
#18601 = CARTESIAN_POINT ( 'NONE',  ( 33.46699938050304013, 24.46183152705960140, 47.04930799450051637 ) ) ;
#18602 = CARTESIAN_POINT ( 'NONE',  ( 48.43975086764982052, 9.161285963347379990, -4.318226157935770360 ) ) ;
#18603 = ORIENTED_EDGE ( 'NONE', *, *, #15756, .F. ) ;
#18604 = CARTESIAN_POINT ( 'NONE',  ( 73.95065972402376531, 11.92558985988973497, 26.63511333407101134 ) ) ;
#18605 = ORIENTED_EDGE ( 'NONE', *, *, #25304, .T. ) ;
#18606 = VERTEX_POINT ( 'NONE', #1916 ) ;
#18607 = AXIS2_PLACEMENT_3D ( 'NONE', #21606, #28681, #18504 ) ;
#18608 = EDGE_CURVE ( 'NONE', #3824, #1215, #2685, .T. ) ;
#18609 = AXIS2_PLACEMENT_3D ( 'NONE', #9847, #32174, #25108 ) ;
#18610 = CIRCLE ( 'NONE', #31193, 55.67821551822382276 ) ;
#18611 = VECTOR ( 'NONE', #32049, 1000.000000000000000 ) ;
#18612 = EDGE_CURVE ( 'NONE', #9970, #15217, #21728, .T. ) ;
#18613 = CIRCLE ( 'NONE', #4481, 0.2551199516247909527 ) ;
#18614 = DIRECTION ( 'NONE',  ( -0.4848096202463429982, -0.8746197071393925215, -9.920727850371698576E-18 ) ) ;
#18615 = CARTESIAN_POINT ( 'NONE',  ( -34.05102927978326477, -3.766592597147156773, 80.60727270474869499 ) ) ;
#18616 = CARTESIAN_POINT ( 'NONE',  ( 21.09992658989239089, 24.71664230456639899, 47.04930799450051637 ) ) ;
#18617 = EDGE_CURVE ( 'NONE', #16477, #10620, #15441, .T. ) ;
#18618 = EDGE_CURVE ( 'NONE', #16711, #7489, #22796, .T. ) ;
#18619 = CIRCLE ( 'NONE', #10812, 12.36707279061065279 ) ;
#18620 = ORIENTED_EDGE ( 'NONE', *, *, #12588, .T. ) ;
#18621 = DIRECTION ( 'NONE',  ( -1.101824276508909887E-16, 1.000000000000000000, -0.000000000000000000 ) ) ;
#18622 = VERTEX_POINT ( 'NONE', #22756 ) ;
#18623 = CARTESIAN_POINT ( 'NONE',  ( 21.09992658989238734, 38.56284415653841791, 47.04930799450051637 ) ) ;
#18624 = DIRECTION ( 'NONE',  ( -1.000000000000000000, -0.000000000000000000, -0.000000000000000000 ) ) ;
#18625 = DIRECTION ( 'NONE',  ( 0.000000000000000000, 0.000000000000000000, -1.000000000000000000 ) ) ;
#18626 = ORIENTED_EDGE ( 'NONE', *, *, #26677, .T. ) ;
#18627 = DIRECTION ( 'NONE',  ( -0.000000000000000000, 1.000000000000000000, -0.000000000000000000 ) ) ;
#18628 = ORIENTED_EDGE ( 'NONE', *, *, #13754, .F. ) ;
#18629 = CARTESIAN_POINT ( 'NONE',  ( 21.09785597605719332, 13.74476430820393347, 47.04930799450051637 ) ) ;
#18630 = DIRECTION ( 'NONE',  ( -2.779292025043186357E-18, 1.288349127009862211E-17, -1.000000000000000000 ) ) ;
#18631 = VERTEX_POINT ( 'NONE', #22914 ) ;
#18632 = LINE ( 'NONE', #28979, #19480 ) ;
#18633 = DIRECTION ( 'NONE',  ( -1.000000000000000000, -1.101824276508910010E-16, 0.000000000000000000 ) ) ;
#18634 = DIRECTION ( 'NONE',  ( 1.169615070119504008E-16, -0.2964022880492265255, 0.9550631830613005580 ) ) ;
#18635 = DIRECTION ( 'NONE',  ( -1.101824276508909887E-16, 1.000000000000000000, -0.000000000000000000 ) ) ;
#18636 = EDGE_LOOP ( 'NONE', ( #19202, #17396, #15734 ) ) ;
#18637 = CARTESIAN_POINT ( 'NONE',  ( 45.96182992765472619, 28.57822092656774160, 44.82232689504103007 ) ) ;
#18638 = CARTESIAN_POINT ( 'NONE',  ( 33.72499318558949710, 24.34184655352419213, 47.04930799450051637 ) ) ;
#18639 = VERTEX_POINT ( 'NONE', #28014 ) ;
#18640 = EDGE_CURVE ( 'NONE', #14790, #11991, #20685, .T. ) ;
#18641 = CARTESIAN_POINT ( 'NONE',  ( -44.31642079201742490, -5.935454207752207445, 40.32453457621193849 ) ) ;
#18642 = AXIS2_PLACEMENT_3D ( 'NONE', #8595, #13689, #25984 ) ;
#18643 = DIRECTION ( 'NONE',  ( -0.000000000000000000, -1.000000000000000000, 0.000000000000000000 ) ) ;
#18644 = ORIENTED_EDGE ( 'NONE', *, *, #31395, .T. ) ;
#18645 = ORIENTED_EDGE ( 'NONE', *, *, #8459, .T. ) ;
#18646 = PRODUCT_DEFINITION_CONTEXT ( 'detailed design', #23750, 'design' ) ;
#18647 = CIRCLE ( 'NONE', #8182, 12.36707279061065101 ) ;
#18648 = VERTEX_POINT ( 'NONE', #30160 ) ;
#18649 = ADVANCED_BREP_SHAPE_REPRESENTATION ( '', ( #1854, #8172 ), #12388 ) ;
#18650 = ADVANCED_FACE ( 'NONE', ( #17510 ), #17830, .T. ) ;
#18651 = EDGE_CURVE ( 'NONE', #13855, #18274, #6545, .T. ) ;
#18652 = VERTEX_POINT ( 'NONE', #17664 ) ;
#18653 = DIRECTION ( 'NONE',  ( -1.101824276508909887E-16, 1.000000000000000000, -0.000000000000000000 ) ) ;
#18654 = AXIS2_PLACEMENT_3D ( 'NONE', #24130, #29387, #28911 ) ;
#18655 =( GEOMETRIC_REPRESENTATION_CONTEXT ( 3 ) GLOBAL_UNCERTAINTY_ASSIGNED_CONTEXT ( ( #21595 ) ) GLOBAL_UNIT_ASSIGNED_CONTEXT ( ( #17430, #27453, #17591 ) ) REPRESENTATION_CONTEXT ( 'NONE', 'WORKASPACE' ) );
#18656 = ADVANCED_FACE ( 'NONE', ( #10298 ), #7053, .T. ) ;
#18657 = EDGE_LOOP ( 'NONE', ( #25884, #8891 ) ) ;
#18658 = ADVANCED_FACE ( 'NONE', ( #5528 ), #31174, .T. ) ;
#18659 = CARTESIAN_POINT ( 'NONE',  ( 48.00914065539375741, 22.93807716476589320, 48.47992731990171933 ) ) ;
#18660 = DIRECTION ( 'NONE',  ( 0.000000000000000000, 0.000000000000000000, -1.000000000000000000 ) ) ;
#18661 = CARTESIAN_POINT ( 'NONE',  ( 21.09785597605720042, -13.59284023713420630, 47.04930799450051637 ) ) ;
#18662 = CARTESIAN_POINT ( 'NONE',  ( 49.44739180854976013, 27.33456182964376779, 47.17133137409169308 ) ) ;
#18663 = ORIENTED_EDGE ( 'NONE', *, *, #13633, .T. ) ;
#18664 = EDGE_LOOP ( 'NONE', ( #27685, #28175 ) ) ;
#18665 = CYLINDRICAL_SURFACE ( 'NONE', #13272, 2.500000000000002220 ) ;
#18666 = ORIENTED_EDGE ( 'NONE', *, *, #16402, .F. ) ;
#18667 = DIRECTION ( 'NONE',  ( -1.000000000000000000, 0.000000000000000000, 0.000000000000000000 ) ) ;
#18668 = AXIS2_PLACEMENT_3D ( 'NONE', #3688, #8298, #18295 ) ;
#18669 = CARTESIAN_POINT ( 'NONE',  ( -40.57420052961184354, 7.102220148652932608, 38.86693366820416884 ) ) ;
#18670 = CARTESIAN_POINT ( 'NONE',  ( -40.69423955692156625, 6.789232590171205395, 39.42520008276828491 ) ) ;
#18671 = DIRECTION ( 'NONE',  ( 0.000000000000000000, 1.000000000000000000, -0.000000000000000000 ) ) ;
#18672 = CARTESIAN_POINT ( 'NONE',  ( -40.08841711228579641, 7.575633567407562552, 53.54930799450051637 ) ) ;
#18673 = CARTESIAN_POINT ( 'NONE',  ( -40.16174044770769314, 7.468546898574135895, 53.54930799450051637 ) ) ;
#18674 = ORIENTED_EDGE ( 'NONE', *, *, #26083, .T. ) ;
#18675 = CARTESIAN_POINT ( 'NONE',  ( 48.34748475735720064, 24.70653309617948423, 49.49898713858203791 ) ) ;
#18676 = CARTESIAN_POINT ( 'NONE',  ( -40.16174044770769314, 7.468546898574136783, 54.64930799450051779 ) ) ;
#18677 = DIRECTION ( 'NONE',  ( -1.000000000000000000, 0.000000000000000000, 0.000000000000000000 ) ) ;
#18678 = CARTESIAN_POINT ( 'NONE',  ( 33.50134396954523197, 28.34164230456639544, 47.04930799450051637 ) ) ;
#18679 = DIRECTION ( 'NONE',  ( -1.000000000000000000, -1.101824276508909887E-16, 0.000000000000000000 ) ) ;
#18680 = EDGE_LOOP ( 'NONE', ( #19100, #181, #21816, #333 ) ) ;
#18681 = CARTESIAN_POINT ( 'NONE',  ( 48.83862994770795041, 25.24118040159427068, 48.17861352429476085 ) ) ;
#18682 = ORIENTED_EDGE ( 'NONE', *, *, #23970, .T. ) ;
#18683 = DIRECTION ( 'NONE',  ( 0.000000000000000000, 1.000000000000000000, 0.000000000000000000 ) ) ;
#18684 = DIRECTION ( 'NONE',  ( 0.4441739386572013393, 0.2110602665713099402, 0.8707256032141217350 ) ) ;
#18685 = AXIS2_PLACEMENT_3D ( 'NONE', #8523, #3587, #26067 ) ;
#18686 = EDGE_LOOP ( 'NONE', ( #32261, #25328 ) ) ;
#18687 = EDGE_CURVE ( 'NONE', #9226, #1319, #25409, .T. ) ;
#18688 = EDGE_LOOP ( 'NONE', ( #21587, #12787, #22489, #28535 ) ) ;
#18689 = CARTESIAN_POINT ( 'NONE',  ( 48.66895200406656130, 25.78420399681023056, 44.62753372671561181 ) ) ;
#18690 = CARTESIAN_POINT ( 'NONE',  ( 21.09785597605720042, -6.314304012688826795, 113.0177564892293987 ) ) ;
#18691 = CARTESIAN_POINT ( 'NONE',  ( 21.09992658989238734, 38.56284415653841791, 47.04930799450051637 ) ) ;
#18692 = EDGE_CURVE ( 'NONE', #19345, #10922, #1280, .T. ) ;
#18693 = ORIENTED_EDGE ( 'NONE', *, *, #21076, .F. ) ;
#18694 = DIRECTION ( 'NONE',  ( -1.000000000000000000, 0.000000000000000000, 0.000000000000000000 ) ) ;
#18695 = CARTESIAN_POINT ( 'NONE',  ( -35.23450526646055891, 11.85135420694099651, 40.60670944852148523 ) ) ;
#18696 = LINE ( 'NONE', #5601, #4337 ) ;
#18697 = AXIS2_PLACEMENT_3D ( 'NONE', #17524, #12124, #17355 ) ;
#18698 = ORIENTED_EDGE ( 'NONE', *, *, #4545, .T. ) ;
#18699 = LINE ( 'NONE', #3777, #10356 ) ;
#18700 = ORIENTED_EDGE ( 'NONE', *, *, #21978, .T. ) ;
#18701 = CARTESIAN_POINT ( 'NONE',  ( 21.09785597605720042, 13.74476430820393347, -8.950692005499485404 ) ) ;
#18702 = CARTESIAN_POINT ( 'NONE',  ( -43.37834615508418068, 1.121909970995877082, 39.54930799450052348 ) ) ;
#18703 = CARTESIAN_POINT ( 'NONE',  ( -40.69571722278732295, 6.786566810383045656, 34.64930799450051779 ) ) ;
#18704 = ORIENTED_EDGE ( 'NONE', *, *, #13439, .F. ) ;
#18705 = ORIENTED_EDGE ( 'NONE', *, *, #28933, .F. ) ;
#18706 = CARTESIAN_POINT ( 'NONE',  ( -40.23397449525940317, 6.794506605641764452, 39.44930799450052206 ) ) ;
#18707 = DIRECTION ( 'NONE',  ( 0.1949050434465252335, -0.6797146636928682595, -0.7071067811865469066 ) ) ;
#18708 = ORIENTED_EDGE ( 'NONE', *, *, #29128, .F. ) ;
#18709 = DIRECTION ( 'NONE',  ( -0.6184495258776564475, 0.3428121700606708289, -0.7071067811865443531 ) ) ;
#18710 = PLANE ( 'NONE',  #18820 ) ;
#18711 = PRODUCT_DEFINITION ( 'UNKNOWN', '', #26528, #23589 ) ;
#18712 = VERTEX_POINT ( 'NONE', #28500 ) ;
#18713 = DIRECTION ( 'NONE',  ( -1.000000000000000000, -1.101824276508910010E-16, 0.000000000000000000 ) ) ;
#18714 = CARTESIAN_POINT ( 'NONE',  ( 44.91142894931555674, 27.29787913140503974, 45.63089057098605394 ) ) ;
#18715 = CARTESIAN_POINT ( 'NONE',  ( 21.09785597605720042, 13.74476430820393347, -7.950692005499485404 ) ) ;
#18716 = AXIS2_PLACEMENT_3D ( 'NONE', #22991, #7586, #12517 ) ;
#18717 = CIRCLE ( 'NONE', #2481, 12.62506659569710443 ) ;
#18718 = AXIS2_PLACEMENT_3D ( 'NONE', #4070, #9169, #19325 ) ;
#18719 = ORIENTED_EDGE ( 'NONE', *, *, #13062, .T. ) ;
#18720 = VECTOR ( 'NONE', #1127, 1000.000000000000000 ) ;
#18721 = DIRECTION ( 'NONE',  ( -1.000000000000000000, 0.000000000000000000, 0.000000000000000000 ) ) ;
#18722 = CARTESIAN_POINT ( 'NONE',  ( 45.96182992765472619, 28.70087065737811827, 44.82232689504103007 ) ) ;
#18723 = CARTESIAN_POINT ( 'NONE',  ( 47.20353132263855400, 25.45286309983299233, 45.01455027646041174 ) ) ;
#18724 = EDGE_CURVE ( 'NONE', #16034, #4198, #9683, .T. ) ;
#18725 = CIRCLE ( 'NONE', #4599, 0.2000000000000012601 ) ;
#18726 = ORIENTED_EDGE ( 'NONE', *, *, #24260, .F. ) ;
#18727 = EDGE_CURVE ( 'NONE', #5329, #12476, #15691, .T. ) ;
#18728 = EDGE_CURVE ( 'NONE', #15237, #16253, #21209, .T. ) ;
#18729 = EDGE_CURVE ( 'NONE', #24958, #27541, #23884, .T. ) ;
#18730 = EDGE_CURVE ( 'NONE', #16546, #30985, #31729, .T. ) ;
#18731 = DIRECTION ( 'NONE',  ( 0.000000000000000000, 0.000000000000000000, 1.000000000000000000 ) ) ;
#18732 = CARTESIAN_POINT ( 'NONE',  ( 46.17891025898683921, 22.93807716476589675, 48.46582155994513386 ) ) ;
#18733 = EDGE_CURVE ( 'NONE', #21016, #1311, #27016, .T. ) ;
#18734 = FACE_BOUND ( 'NONE', #11808, .T. ) ;
#18735 = EDGE_LOOP ( 'NONE', ( #12031, #1805, #9792, #10119 ) ) ;
#18736 = FACE_OUTER_BOUND ( 'NONE', #30701, .T. ) ;
#18737 = CARTESIAN_POINT ( 'NONE',  ( 8.698509210239526723, 26.09164230456639899, 47.04930799450051637 ) ) ;
#18738 = DIRECTION ( 'NONE',  ( -8.751303817264967506E-17, -0.6995351541602693457, -0.7145981864614324719 ) ) ;
#18739 = CARTESIAN_POINT ( 'NONE',  ( -40.58856461370174884, 7.499380836222963254, 60.14930799450051779 ) ) ;
#18740 = ORIENTED_EDGE ( 'NONE', *, *, #6625, .F. ) ;
#18741 = CARTESIAN_POINT ( 'NONE',  ( 46.79396160029377683, 22.86454579224780659, 45.03082974987060538 ) ) ;
#18743 = CARTESIAN_POINT ( 'NONE',  ( 46.00908685603032922, 26.14624452788249087, 44.91496614357595263 ) ) ;
#18742 = AXIS2_PLACEMENT_3D ( 'NONE', #29724, #22479, #170 ) ;
#18744 = VECTOR ( 'NONE', #13245, 1000.000000000000000 ) ;
#18745 = CARTESIAN_POINT ( 'NONE',  ( 21.09992658989239089, 24.96664230456639899, 47.04930799450051637 ) ) ;
#18746 = CARTESIAN_POINT ( 'NONE',  ( -40.11553135844172147, 6.871094863070437597, 34.58253047105350220 ) ) ;
#18747 = CIRCLE ( 'NONE', #3581, 54.30000000000000426 ) ;
#18748 = CARTESIAN_POINT ( 'NONE',  ( -39.58809650894544774, 2.596771453999702661, 47.04930799450051637 ) ) ;
#18749 = VERTEX_POINT ( 'NONE', #3865 ) ;
#18750 = DIRECTION ( 'NONE',  ( -1.000000000000000000, 0.000000000000000000, 0.000000000000000000 ) ) ;
#18751 = CARTESIAN_POINT ( 'NONE',  ( 106.0978559760575735, 11.92558985988973497, 26.63511333407112858 ) ) ;
#18752 = FACE_OUTER_BOUND ( 'NONE', #24294, .T. ) ;
#18753 = VECTOR ( 'NONE', #12125, 999.9999999999998863 ) ;
#18754 = VERTEX_POINT ( 'NONE', #16016 ) ;
#18755 = DIRECTION ( 'NONE',  ( -1.101824276508909887E-16, 1.000000000000000000, -0.000000000000000000 ) ) ;
#18756 = CARTESIAN_POINT ( 'NONE',  ( 21.09785597605720753, 13.86454579224779948, 47.04930799450052348 ) ) ;
#18757 = LINE ( 'NONE', #21874, #25154 ) ;
#18758 = DIRECTION ( 'NONE',  ( -0.000000000000000000, 1.000000000000000000, -0.000000000000000000 ) ) ;
#18759 = ORIENTED_EDGE ( 'NONE', *, *, #15632, .T. ) ;
#18760 = CARTESIAN_POINT ( 'NONE',  ( 21.09785597605718976, -13.68121847681060643, 47.04930799450051637 ) ) ;
#18761 = ORIENTED_EDGE ( 'NONE', *, *, #25215, .F. ) ;
#18762 = ADVANCED_FACE ( 'NONE', ( #20934 ), #6165, .F. ) ;
#18763 = ORIENTED_EDGE ( 'NONE', *, *, #17236, .T. ) ;
#18764 = AXIS2_PLACEMENT_3D ( 'NONE', #17941, #30592, #22371 ) ;
#18765 = CIRCLE ( 'NONE', #4637, 1.500000000000001332 ) ;
#18766 = VECTOR ( 'NONE', #4105, 1000.000000000000114 ) ;
#18767 = EDGE_CURVE ( 'NONE', #12476, #28743, #32250, .T. ) ;
#18768 = ADVANCED_FACE ( 'NONE', ( #23560 ), #13885, .F. ) ;
#18769 = AXIS2_PLACEMENT_3D ( 'NONE', #28518, #25243, #15707 ) ;
#18770 = CARTESIAN_POINT ( 'NONE',  ( -42.28293707589220674, 13.65198258188957148, 59.54475713566496609 ) ) ;
#18771 = CARTESIAN_POINT ( 'NONE',  ( 45.96182992765471909, 25.90087065737812466, 44.82232689504102296 ) ) ;
#18772 = CARTESIAN_POINT ( 'NONE',  ( 81.68521218355431301, -5.935668157269678780, 78.02222375751645700 ) ) ;
#18773 = EDGE_CURVE ( 'NONE', #2250, #16708, #13395, .T. ) ;
#18774 = ORIENTED_EDGE ( 'NONE', *, *, #6044, .T. ) ;
#18775 = AXIS2_PLACEMENT_3D ( 'NONE', #30893, #13495, #18401 ) ;
#18776 = DIRECTION ( 'NONE',  ( 0.2756373558170082672, -0.9612616959383162296, 0.000000000000000000 ) ) ;
#18777 = ORIENTED_EDGE ( 'NONE', *, *, #28366, .F. ) ;
#18778 = FACE_OUTER_BOUND ( 'NONE', #18948, .T. ) ;
#18779 = DIRECTION ( 'NONE',  ( 0.000000000000000000, 0.000000000000000000, 1.000000000000000000 ) ) ;
#18780 = DIRECTION ( 'NONE',  ( 1.000000000000000000, 0.000000000000000000, 0.000000000000000000 ) ) ;
#18781 = VERTEX_POINT ( 'NONE', #1079 ) ;
#18782 = DIRECTION ( 'NONE',  ( 0.000000000000000000, 0.000000000000000000, 1.000000000000000000 ) ) ;
#18783 = CARTESIAN_POINT ( 'NONE',  ( 21.09785597605719332, 24.74924423484549507, 7.113493622051541010 ) ) ;
#18784 = DIRECTION ( 'NONE',  ( -1.000000000000000000, -1.101824276508910010E-16, 0.000000000000000000 ) ) ;
#18785 = ORIENTED_EDGE ( 'NONE', *, *, #30440, .F. ) ;
#18786 = CARTESIAN_POINT ( 'NONE',  ( 46.61910388458303345, 22.93328494799376216, 45.39920705986084215 ) ) ;
#18787 = CYLINDRICAL_SURFACE ( 'NONE', #24133, 12.36707279061065101 ) ;
#18788 = PLANE ( 'NONE',  #3685 ) ;
#18789 = CARTESIAN_POINT ( 'NONE',  ( 21.09992658989239089, 28.09164230456639544, 47.04930799450051637 ) ) ;
#18790 = ORIENTED_EDGE ( 'NONE', *, *, #22715, .T. ) ;
#18791 = CARTESIAN_POINT ( 'NONE',  ( -40.12089182904525586, 6.795442088152954696, 34.54930799450050927 ) ) ;
#18792 = CARTESIAN_POINT ( 'NONE',  ( -40.64264863745435719, 6.822556421824200967, 34.67218454412468986 ) ) ;
#18793 = EDGE_LOOP ( 'NONE', ( #14459, #11092 ) ) ;
#18794 = CARTESIAN_POINT ( 'NONE',  ( -44.02797724526854495, -5.204561149836106182, 41.60063710421776051 ) ) ;
#18795 = B_SPLINE_CURVE_WITH_KNOTS ( 'NONE', 3,
 ( #7641, #17635, #10268, #7796, #17797, #27821, #25353, #30451, #9077, #6458, #31407, #6291 ),
 .UNSPECIFIED., .F., .F.,
 ( 4, 2, 2, 2, 2, 4 ),
 ( 0.000000000000000000, 7.988424390431281264E-05, 0.0001597684878086256253, 0.0001997106097607669680, 0.0002396527317129083649, 0.0003195369756171903726 ),
 .UNSPECIFIED. ) ;
#18796 = CIRCLE ( 'NONE', #19865, 0.1250000000000018319 ) ;
#18797 = FACE_OUTER_BOUND ( 'NONE', #27187, .T. ) ;
#18798 = CIRCLE ( 'NONE', #4071, 1.300000000000002487 ) ;
#18799 = ORIENTED_EDGE ( 'NONE', *, *, #992, .T. ) ;
#18800 = ORIENTED_EDGE ( 'NONE', *, *, #16167, .T. ) ;
#18801 = EDGE_CURVE ( 'NONE', #112, #14283, #9185, .T. ) ;
#18802 = ADVANCED_FACE ( 'NONE', ( #3536 ), #17047, .T. ) ;
#18803 = VECTOR ( 'NONE', #17229, 1000.000000000000000 ) ;
#18804 = VERTEX_POINT ( 'NONE', #8782 ) ;
#18805 = VERTEX_POINT ( 'NONE', #3377 ) ;
#18806 = ADVANCED_FACE ( 'NONE', ( #16170 ), #13410, .T. ) ;
#18807 = CIRCLE ( 'NONE', #31425, 0.1250000000000001110 ) ;
#18808 = TOROIDAL_SURFACE ( 'NONE', #19363, 12.40141737965284463, 0.1250000000000005274 ) ;
#18809 = ORIENTED_EDGE ( 'NONE', *, *, #16881, .T. ) ;
#18810 = CARTESIAN_POINT ( 'NONE',  ( -42.30123736278718383, 13.66041317296246937, 59.53596428539564300 ) ) ;
#18811 = DIRECTION ( 'NONE',  ( -1.000000000000000000, 0.000000000000000000, 0.000000000000000000 ) ) ;
#18812 = DIRECTION ( 'NONE',  ( 0.000000000000000000, 0.000000000000000000, -1.000000000000000000 ) ) ;
#18813 = CARTESIAN_POINT ( 'NONE',  ( 46.71168188241476571, 25.16454579224780019, 44.57931415454905988 ) ) ;
#18814 = CARTESIAN_POINT ( 'NONE',  ( 48.80717017713595141, 27.31952976649965592, 48.15820438821415195 ) ) ;
#18815 = ORIENTED_EDGE ( 'NONE', *, *, #19441, .T. ) ;
#18816 = ORIENTED_EDGE ( 'NONE', *, *, #7379, .T. ) ;
#18817 = CARTESIAN_POINT ( 'NONE',  ( 21.09992658989239089, 26.47145308207318593, 47.04930799450051637 ) ) ;
#18818 = ORIENTED_EDGE ( 'NONE', *, *, #5908, .T. ) ;
#18819 = CARTESIAN_POINT ( 'NONE',  ( 48.74040444119073356, 29.48593875711943113, 48.49014004655320065 ) ) ;
#18820 = AXIS2_PLACEMENT_3D ( 'NONE', #19367, #21501, #14302 ) ;
#18821 = AXIS2_PLACEMENT_3D ( 'NONE', #13231, #18281, #28315 ) ;
#18822 = DIRECTION ( 'NONE',  ( -0.000000000000000000, -1.000000000000000000, 0.000000000000000000 ) ) ;
#18823 = CARTESIAN_POINT ( 'NONE',  ( -40.68984688381694070, 6.797157182225249450, 39.37314909236572191 ) ) ;
#18824 = CARTESIAN_POINT ( 'NONE',  ( 8.482002859293471531, 31.71664230456639544, 47.04930799450051637 ) ) ;
#18825 = CARTESIAN_POINT ( 'NONE',  ( 45.46000861347822308, 28.17287913140503619, 49.57397645940629616 ) ) ;
#18826 = CIRCLE ( 'NONE', #13607, 0.1250000000000001110 ) ;
#18827 = CARTESIAN_POINT ( 'NONE',  ( -3.128431330128486287, 11.18784031540631574, -4.623178182644472223 ) ) ;
#18828 = DIRECTION ( 'NONE',  ( 0.4848096202463506588, 0.8746197071393884137, 9.920727850371624621E-18 ) ) ;
#18829 = EDGE_CURVE ( 'NONE', #31159, #1392, #7078, .T. ) ;
#18830 = ORIENTED_EDGE ( 'NONE', *, *, #1746, .F. ) ;
#18831 = CYLINDRICAL_SURFACE ( 'NONE', #6635, 12.36707279061065101 ) ;
#18832 = AXIS2_PLACEMENT_3D ( 'NONE', #1529, #8607, #24177 ) ;
#18833 = FACE_OUTER_BOUND ( 'NONE', #5038, .T. ) ;
#18834 = DIRECTION ( 'NONE',  ( -1.000000000000000000, 0.000000000000000000, 0.000000000000000000 ) ) ;
#18835 = ADVANCED_FACE ( 'NONE', ( #26181 ), #1394, .T. ) ;
#18836 = DIRECTION ( 'NONE',  ( 0.2756373558169970539, -0.9612616959383194493, -1.315048337272770435E-17 ) ) ;
#18837 = CARTESIAN_POINT ( 'NONE',  ( 21.09992658989239089, 23.84164230456639544, 47.04930799450051637 ) ) ;
#18838 = ORIENTED_EDGE ( 'NONE', *, *, #5753, .T. ) ;
#18839 = FACE_OUTER_BOUND ( 'NONE', #7501, .T. ) ;
#18840 = ORIENTED_EDGE ( 'NONE', *, *, #14409, .F. ) ;
#18841 = FACE_OUTER_BOUND ( 'NONE', #23596, .T. ) ;
#18842 = FACE_OUTER_BOUND ( 'NONE', #22546, .T. ) ;
#18843 = EDGE_CURVE ( 'NONE', #11316, #7874, #21758, .T. ) ;
#18844 = AXIS2_PLACEMENT_3D ( 'NONE', #1038, #12891, #11064 ) ;
#18845 = EDGE_CURVE ( 'NONE', #5658, #17034, #25425, .T. ) ;
#18846 = EDGE_CURVE ( 'NONE', #2312, #18936, #20195, .T. ) ;
#18847 = ORIENTED_EDGE ( 'NONE', *, *, #30138, .T. ) ;
#18848 = AXIS2_PLACEMENT_3D ( 'NONE', #1269, #26059, #6207 ) ;
#18849 = VECTOR ( 'NONE', #9021, 1000.000000000000000 ) ;
#18850 = EDGE_LOOP ( 'NONE', ( #10463, #9982, #8533, #31708 ) ) ;
#18851 = AXIS2_PLACEMENT_3D ( 'NONE', #30324, #28348, #15870 ) ;
#18852 = CARTESIAN_POINT ( 'NONE',  ( 47.60921136374460616, 22.86454579224779948, 45.07316987100104200 ) ) ;
#18853 = EDGE_CURVE ( 'NONE', #23707, #9682, #27544, .T. ) ;
#18854 = AXIS2_PLACEMENT_3D ( 'NONE', #11876, #27131, #31741 ) ;
#18855 = DIRECTION ( 'NONE',  ( 0.000000000000000000, -0.000000000000000000, -1.000000000000000000 ) ) ;
#18856 = CYLINDRICAL_SURFACE ( 'NONE', #15220, 2.500000000000002220 ) ;
#18857 = ORIENTED_EDGE ( 'NONE', *, *, #6962, .F. ) ;
#18858 = CARTESIAN_POINT ( 'NONE',  ( -20.95081142018943510, -13.30632128221581212, 10.16668169048477566 ) ) ;
#18859 = DIRECTION ( 'NONE',  ( -1.224646799147353207E-16, -1.349345573449484691E-32, 1.000000000000000000 ) ) ;
#18860 = CARTESIAN_POINT ( 'NONE',  ( -25.18206523986666312, 14.81645899701909563, 47.04930799450052348 ) ) ;
#18861 = ORIENTED_EDGE ( 'NONE', *, *, #14465, .T. ) ;
#18862 = DIRECTION ( 'NONE',  ( 0.8746197071393925215, -0.4848096202463429982, -8.676864087101708112E-18 ) ) ;
#18863 = CIRCLE ( 'NONE', #29907, 0.1250000000000001110 ) ;
#18864 = VERTEX_POINT ( 'NONE', #9773 ) ;
#18865 = CYLINDRICAL_SURFACE ( 'NONE', #21158, 2.500000000000002220 ) ;
#18866 = DIRECTION ( 'NONE',  ( 0.000000000000000000, 1.000000000000000000, -0.000000000000000000 ) ) ;
#18867 = CARTESIAN_POINT ( 'NONE',  ( 21.09992658989238734, 30.96664230456641675, 47.04930799450051637 ) ) ;
#18868 = EDGE_CURVE ( 'NONE', #10602, #9753, #18092, .T. ) ;
#18869 = ORIENTED_EDGE ( 'NONE', *, *, #31391, .T. ) ;
#18870 = VERTEX_POINT ( 'NONE', #14530 ) ;
#18871 = CARTESIAN_POINT ( 'NONE',  ( 21.09992658989239089, 28.34164230456639544, 47.04930799450051637 ) ) ;
#18872 = CARTESIAN_POINT ( 'NONE',  ( -42.38687957179150345, 4.148162238788003719, 57.04930799450051637 ) ) ;
#18873 = AXIS2_PLACEMENT_3D ( 'NONE', #26417, #21314, #31350 ) ;
#18874 = EDGE_CURVE ( 'NONE', #15187, #3444, #2218, .T. ) ;
#18875 = DIRECTION ( 'NONE',  ( -0.000000000000000000, -1.000000000000000000, 0.000000000000000000 ) ) ;
#18876 = ORIENTED_EDGE ( 'NONE', *, *, #1074, .T. ) ;
#18877 = CARTESIAN_POINT ( 'NONE',  ( 33.46699938050302592, 32.47145308207318237, 47.04930799450050927 ) ) ;
#18878 = VECTOR ( 'NONE', #16901, 1000.000000000000000 ) ;
#18879 = FACE_OUTER_BOUND ( 'NONE', #20657, .T. ) ;
#18880 = ORIENTED_EDGE ( 'NONE', *, *, #7815, .F. ) ;
#18881 = AXIS2_PLACEMENT_3D ( 'NONE', #24900, #25224, #9639 ) ;
#18882 = CARTESIAN_POINT ( 'NONE',  ( 48.46535932150934656, 27.58954579807170759, 49.73005965046827015 ) ) ;
#18883 = TOROIDAL_SURFACE ( 'NONE', #18294, 64.50000000000000000, 5.099019513592785380 ) ;
#18884 = CIRCLE ( 'NONE', #31482, 12.27641737965286239 ) ;
#18885 = EDGE_CURVE ( 'NONE', #30931, #14214, #30176, .T. ) ;
#18886 = CARTESIAN_POINT ( 'NONE',  ( 21.09785597605720753, 13.86454579224779948, 47.04930799450052348 ) ) ;
#18887 = EDGE_CURVE ( 'NONE', #3483, #32275, #16513, .T. ) ;
#18888 = CIRCLE ( 'NONE', #23104, 1.199999999999999734 ) ;
#18889 = ORIENTED_EDGE ( 'NONE', *, *, #17751, .T. ) ;
#18890 = CARTESIAN_POINT ( 'NONE',  ( 21.09992658989239089, 29.34164230456639899, 47.04930799450051637 ) ) ;
#18891 = CARTESIAN_POINT ( 'NONE',  ( 52.05217022815784844, -5.936245040125577077, -13.58841950574782587 ) ) ;
#18892 = DIRECTION ( 'NONE',  ( 0.8746197071393926326, -0.4848096202463430537, -8.676864087101709653E-18 ) ) ;
#18893 = CARTESIAN_POINT ( 'NONE',  ( 46.02876340639226527, 26.21119643316632164, 44.95353858666495483 ) ) ;
#18894 = VECTOR ( 'NONE', #12737, 1000.000000000000227 ) ;
#18895 = ORIENTED_EDGE ( 'NONE', *, *, #3600, .F. ) ;
#18896 = CIRCLE ( 'NONE', #11085, 0.3000000000000016542 ) ;
#18897 = AXIS2_PLACEMENT_3D ( 'NONE', #4465, #31876, #16599 ) ;
#18898 = DIRECTION ( 'NONE',  ( -1.101824276508909887E-16, 1.000000000000000000, -0.000000000000000000 ) ) ;
#18899 = CARTESIAN_POINT ( 'NONE',  ( 48.59785597605720397, 14.86454579224779948, 47.04930799450052348 ) ) ;
#18900 = VECTOR ( 'NONE', #31124, 1000.000000000000000 ) ;
#18901 = LINE ( 'NONE', #1505, #8389 ) ;
#18902 = AXIS2_PLACEMENT_3D ( 'NONE', #12740, #85, #10107 ) ;
#18903 = CARTESIAN_POINT ( 'NONE',  ( 45.52675994804781112, 26.71155426599985461, 49.47108226228597516 ) ) ;
#18904 = CARTESIAN_POINT ( 'NONE',  ( -40.60333149162104860, 7.557375771971039491, 54.01510846932453092 ) ) ;
#18905 = DIRECTION ( 'NONE',  ( -1.101824276508909887E-16, 1.000000000000000000, -0.000000000000000000 ) ) ;
#18906 =( NAMED_UNIT ( * ) PLANE_ANGLE_UNIT ( ) SI_UNIT ( $, .RADIAN. ) );
#18907 = ORIENTED_EDGE ( 'NONE', *, *, #24446, .T. ) ;
#18908 = DIRECTION ( 'NONE',  ( -1.101824276508909887E-16, 1.000000000000000000, -0.000000000000000000 ) ) ;
#18909 = CARTESIAN_POINT ( 'NONE',  ( 48.83862994770794330, 28.65457786121581663, 48.17861352429476796 ) ) ;
#18910 = CONICAL_SURFACE ( 'NONE', #1632, 55.00000000000000000, 0.7853981633974552734 ) ;
#18911 = CARTESIAN_POINT ( 'NONE',  ( 33.37634396954521065, 30.09164230456639544, 47.04930799450051637 ) ) ;
#18912 = FACE_OUTER_BOUND ( 'NONE', #27714, .T. ) ;
#18913 = CARTESIAN_POINT ( 'NONE',  ( 21.09992658989239089, 25.84143805560860940, 47.04930799450051637 ) ) ;
#18914 = ORIENTED_EDGE ( 'NONE', *, *, #6801, .T. ) ;
#18915 = DIRECTION ( 'NONE',  ( 0.4848096202463673121, 0.8746197071393789768, 0.000000000000000000 ) ) ;
#18916 = DIRECTION ( 'NONE',  ( -0.2756373558169930016, 0.9612616959383205595, 1.315048337272770743E-17 ) ) ;
#18917 = CARTESIAN_POINT ( 'NONE',  ( 21.09785597605720753, 14.05098971466613023, 47.04930799450052348 ) ) ;
#18918 = ORIENTED_EDGE ( 'NONE', *, *, #15872, .T. ) ;
#18919 = CARTESIAN_POINT ( 'NONE',  ( 21.09785597605719332, 6.547041198165487685, 47.04930799450051637 ) ) ;
#18920 = FACE_OUTER_BOUND ( 'NONE', #696, .T. ) ;
#18921 = CARTESIAN_POINT ( 'NONE',  ( -43.64073206722599707, 1.267352857069779848, 39.54930799450052348 ) ) ;
#18922 = ADVANCED_FACE ( 'NONE', ( #24210 ), #10255, .T. ) ;
#18923 = DIRECTION ( 'NONE',  ( 0.000000000000000000, 0.000000000000000000, 1.000000000000000000 ) ) ;
#18924 = ORIENTED_EDGE ( 'NONE', *, *, #30909, .F. ) ;
#18925 = AXIS2_PLACEMENT_3D ( 'NONE', #8961, #23896, #31933 ) ;
#18926 = ORIENTED_EDGE ( 'NONE', *, *, #7613, .T. ) ;
#18927 = TOROIDAL_SURFACE ( 'NONE', #12684, 12.40141737965281088, 0.1249999999999987788 ) ;
#18928 = CLOSED_SHELL ( 'NONE', ( #27878, #12504, #5547, #30912, #14199, #1509, #21838, #25613, #9339, #28752, #8346, #19374, #6667, #15452, #31101, #12227, #857, #32278, #17380, #8197, #28204, #5952, #21469, #13357, #14435, #14126, #5858, #30443, #24884, #4177, #16202, #15969, #4040, #10690, #9910, #8676, #18372, #24686, #9456, #669, #27801, #15163, #7080, #5968, #10171, #19934, #18208, #13103, #1893, #10872, #12584, #8927, #18433, #7210, #24512, #4442, #9672, #17021, #4969, #892, #13489, #18762, #32171, #17325, #18053, #24270, #3026, #10054, #25172, #11002, #9829, #4740, #11759, #29394, #24428, #27670, #22904, #1115, #1, #19828, #29271, #27021, #22613, #20798, #9041, #13986, #31492, #7816, #10613, #30687, #17789, #24292, #12052, #23529, #31258, #24520, #1791, #32029, #1175, #22154, #26207, #12877, #20233, #24829, #14805, #22590, #25262, #10354, #24025, #14989, #13540, #30028, #31786, #30827, #22783, #18407, #20117, #15641, #11234, #6219, #30220, #22404 ) ) ;
#18929 = VECTOR ( 'NONE', #4195, 1000.000000000000000 ) ;
#18930 = ORIENTED_EDGE ( 'NONE', *, *, #10954, .F. ) ;
#18931 =( BOUNDED_CURVE ( )  B_SPLINE_CURVE ( 3, ( #22808, #2304, #4597, #25115 ),
 .UNSPECIFIED., .F., .F. ) 
 B_SPLINE_CURVE_WITH_KNOTS ( ( 4, 4 ),
 ( 0.1488899476094779073, 1.570796326794886344 ),
 .UNSPECIFIED. ) 
 CURVE ( )  GEOMETRIC_REPRESENTATION_ITEM ( )  RATIONAL_B_SPLINE_CURVE ( ( 1.000000000000000000, 0.8384934736035551950, 0.8384934736035551950, 1.000000000000000000 ) ) 
 REPRESENTATION_ITEM ( '' )  );
#18932 = CIRCLE ( 'NONE', #21561, 12.00000000000000355 ) ;
#18933 = DIRECTION ( 'NONE',  ( 0.000000000000000000, 1.000000000000000000, 0.000000000000000000 ) ) ;
#18934 = FACE_OUTER_BOUND ( 'NONE', #24324, .T. ) ;
#18935 = CARTESIAN_POINT ( 'NONE',  ( 8.474859994195286461, 25.59184655352419213, 47.04930799450051637 ) ) ;
#18936 = VERTEX_POINT ( 'NONE', #26510 ) ;
#18937 = FACE_OUTER_BOUND ( 'NONE', #6890, .T. ) ;
#18938 = ORIENTED_EDGE ( 'NONE', *, *, #14475, .T. ) ;
#18939 = COLOUR_RGB ( '',0.7921568627450980005, 0.8196078431372548767, 0.9333333333333333481 ) ;
#18940 = CARTESIAN_POINT ( 'NONE',  ( 21.09785597605719332, -5.935454207752083988, -20.13750291342764598 ) ) ;
#18941 = AXIS2_PLACEMENT_3D ( 'NONE', #22522, #27463, #7109 ) ;
#18942 = DIRECTION ( 'NONE',  ( -0.9612616959383200044, -0.2756373558169954996, 1.660411357259285896E-16 ) ) ;
#18943 = ORIENTED_EDGE ( 'NONE', *, *, #21858, .F. ) ;
#18944 = DIRECTION ( 'NONE',  ( -1.000000000000000000, 0.000000000000000000, 0.000000000000000000 ) ) ;
#18945 = CARTESIAN_POINT ( 'NONE',  ( 21.09785597605720753, 14.46497581658974063, 47.04930799450052348 ) ) ;
#18946 = CARTESIAN_POINT ( 'NONE',  ( 100.3079064823960493, -16.63545420775219696, 44.54930799450134771 ) ) ;
#18947 =( LENGTH_UNIT ( ) NAMED_UNIT ( * ) SI_UNIT ( .MILLI., .METRE. ) );
#18948 = EDGE_LOOP ( 'NONE', ( #7865, #30694, #16147, #23655 ) ) ;
#18949 = CARTESIAN_POINT ( 'NONE',  ( 67.18867716679213231, 14.05098971466613023, 47.04930799450051637 ) ) ;
#18950 = DIRECTION ( 'NONE',  ( -1.101824276508909887E-16, 1.000000000000000000, -0.000000000000000000 ) ) ;
#18951 = DIRECTION ( 'NONE',  ( 1.000000000000000000, 0.000000000000000000, 0.000000000000000000 ) ) ;
#18952 = CARTESIAN_POINT ( 'NONE',  ( 21.09785597605719687, 42.30003263981368633, 77.04930799450052348 ) ) ;
#18953 = VERTEX_POINT ( 'NONE', #21898 ) ;
#18954 = FACE_OUTER_BOUND ( 'NONE', #2890, .T. ) ;
#18955 = CARTESIAN_POINT ( 'NONE',  ( 33.46699938050304013, 24.21183152705959785, 47.04930799450051637 ) ) ;
#18956 = EDGE_LOOP ( 'NONE', ( #19459, #20999, #7855, #30466, #21271 ) ) ;
#18957 = LINE ( 'NONE', #14059, #1467 ) ;
#18958 = AXIS2_PLACEMENT_3D ( 'NONE', #9933, #19446, #31768 ) ;
#18959 = CARTESIAN_POINT ( 'NONE',  ( 21.09992658989239089, 29.09164230456639899, 47.04930799450051637 ) ) ;
#18960 = EDGE_CURVE ( 'NONE', #5905, #9364, #18610, .T. ) ;
#18961 = EDGE_CURVE ( 'NONE', #6997, #15396, #4476, .T. ) ;
#18962 = AXIS2_PLACEMENT_3D ( 'NONE', #26017, #11531, #22014 ) ;
#18963 = ORIENTED_EDGE ( 'NONE', *, *, #10905, .T. ) ;
#18964 = ADVANCED_FACE ( 'NONE', ( #14371, #31604 ), #29297, .F. ) ;
#18965 = ORIENTED_EDGE ( 'NONE', *, *, #19053, .F. ) ;
#18966 = EDGE_CURVE ( 'NONE', #12082, #17901, #31926, .T. ) ;
#18967 = EDGE_CURVE ( 'NONE', #18206, #31078, #31226, .T. ) ;
#18968 = ORIENTED_EDGE ( 'NONE', *, *, #11049, .T. ) ;
#18969 = AXIS2_PLACEMENT_3D ( 'NONE', #18678, #5306, #21301 ) ;
#18970 = PRODUCT_DEFINITION_SHAPE ( 'NONE', 'NONE',  #32503 ) ;
#18971 = CARTESIAN_POINT ( 'NONE',  ( 21.09785597605719332, 25.56454579224779167, 34.04930799450050927 ) ) ;
#18972 = EDGE_LOOP ( 'NONE', ( #13125, #32479, #8443 ) ) ;
#18973 = CARTESIAN_POINT ( 'NONE',  ( -40.70484894842233103, 8.274204744976163539, 54.64930799450051779 ) ) ;
#18974 = AXIS2_PLACEMENT_3D ( 'NONE', #26431, #4273, #31843 ) ;
#18975 = FACE_OUTER_BOUND ( 'NONE', #21462, .T. ) ;
#18976 = CARTESIAN_POINT ( 'NONE',  ( 8.474859994195286461, 28.09143805560861296, 47.04930799450051637 ) ) ;
#18977 = CARTESIAN_POINT ( 'NONE',  ( -40.31405849284424647, 8.392931372713462679, 40.47149053519531492 ) ) ;
#18978 = CIRCLE ( 'NONE', #3279, 12.62506659569710266 ) ;
#18979 = CARTESIAN_POINT ( 'NONE',  ( 45.28286642839709231, 24.94289516297709852, 47.97516931882780966 ) ) ;
#18980 = EDGE_CURVE ( 'NONE', #10403, #13364, #28054, .T. ) ;
#18981 = ORIENTED_EDGE ( 'NONE', *, *, #12621, .F. ) ;
#18982 = VERTEX_POINT ( 'NONE', #9444 ) ;
#18983 = DIRECTION ( 'NONE',  ( 0.000000000000000000, 0.000000000000000000, -1.000000000000000000 ) ) ;
#18984 = ADVANCED_FACE ( 'NONE', ( #16973 ), #19442, .F. ) ;
#18985 = EDGE_LOOP ( 'NONE', ( #15888, #8040, #29681, #17310 ) ) ;
#18987 = VECTOR ( 'NONE', #10790, 1000.000000000000000 ) ;
#18986 = CARTESIAN_POINT ( 'NONE',  ( 49.20498434852767389, 29.54590370372963903, 46.77290885782220187 ) ) ;
#18988 = LINE ( 'NONE', #1001, #9497 ) ;
#18989 = DIRECTION ( 'NONE',  ( -0.000000000000000000, 1.000000000000000000, -0.000000000000000000 ) ) ;
#18990 = CARTESIAN_POINT ( 'NONE',  ( 21.09992658989238734, 38.56284415653841791, 47.04930799450051637 ) ) ;
#18991 = LINE ( 'NONE', #4889, #10657 ) ;
#18992 = CARTESIAN_POINT ( 'NONE',  ( 47.23302798462060537, 25.08121246473838184, 44.44659793406428605 ) ) ;
#18993 = VECTOR ( 'NONE', #8969, 1000.000000000000000 ) ;
#18994 = CARTESIAN_POINT ( 'NONE',  ( 33.72499318558949710, 32.09143805560860585, 47.04930799450051637 ) ) ;
#18995 = CARTESIAN_POINT ( 'NONE',  ( 33.37634396954526039, 25.34164230456639899, 47.04930799450051637 ) ) ;
#18996 = ORIENTED_EDGE ( 'NONE', *, *, #11827, .F. ) ;
#18997 = CARTESIAN_POINT ( 'NONE',  ( -40.38516919650994197, 8.640923867788874446, 39.54930799450052348 ) ) ;
#18998 = DIRECTION ( 'NONE',  ( -1.000000000000000000, 0.000000000000000000, 0.000000000000000000 ) ) ;
#18999 = DIRECTION ( 'NONE',  ( 0.2756373558169958327, -0.9612616959383198934, 0.000000000000000000 ) ) ;
#19000 = LINE ( 'NONE', #29031, #23187 ) ;
#19001 = DIRECTION ( 'NONE',  ( -1.101824276508909887E-16, 1.000000000000000000, -0.000000000000000000 ) ) ;
#19002 = VERTEX_POINT ( 'NONE', #24530 ) ;
#19003 = CYLINDRICAL_SURFACE ( 'NONE', #12475, 2.000000000000001776 ) ;
#19004 = EDGE_LOOP ( 'NONE', ( #30426, #3260, #5721, #6790 ) ) ;
#19005 = FACE_OUTER_BOUND ( 'NONE', #10484, .T. ) ;
#19006 = EDGE_CURVE ( 'NONE', #29925, #12345, #3938, .T. ) ;
#19007 = VERTEX_POINT ( 'NONE', #15340 ) ;
#19008 = AXIS2_PLACEMENT_3D ( 'NONE', #32464, #27371, #24912 ) ;
#19009 = VECTOR ( 'NONE', #5892, 1000.000000000000000 ) ;
#19010 = CIRCLE ( 'NONE', #5432, 37.50000000000000711 ) ;
#19011 = VECTOR ( 'NONE', #5416, 1000.000000000000000 ) ;
#19012 = ORIENTED_EDGE ( 'NONE', *, *, #22578, .T. ) ;
#19013 = EDGE_CURVE ( 'NONE', #32160, #12556, #19126, .T. ) ;
#19014 = CARTESIAN_POINT ( 'NONE',  ( 48.35473289974373756, 22.80400562401889530, 45.11188864597615833 ) ) ;
#19015 = LINE ( 'NONE', #29044, #15505 ) ;
#19016 = CARTESIAN_POINT ( 'NONE',  ( 47.09785597605719687, 30.56554579224779644, 47.04930799450078638 ) ) ;
#19017 = ADVANCED_FACE ( 'NONE', ( #12563 ), #17305, .F. ) ;
#19018 = ORIENTED_EDGE ( 'NONE', *, *, #21024, .F. ) ;
#19019 = DIRECTION ( 'NONE',  ( 0.3428121700606686084, 0.6184495258776648852, -0.7071067811865382469 ) ) ;
#19020 = DIRECTION ( 'NONE',  ( -1.000000000000000000, 0.000000000000000000, 0.000000000000000000 ) ) ;
#19021 = CARTESIAN_POINT ( 'NONE',  ( 72.84673228687861979, 6.668192824305379851, 17.53718116896199675 ) ) ;
#19022 = ADVANCED_FACE ( 'NONE', ( #32420 ), #23843, .T. ) ;
#19023 = ORIENTED_EDGE ( 'NONE', *, *, #8709, .T. ) ;
#19024 = CARTESIAN_POINT ( 'NONE',  ( -43.86407712052087504, -0.06377168781008255016, 32.09930799450052064 ) ) ;
#19025 = EDGE_CURVE ( 'NONE', #28135, #27014, #13907, .T. ) ;
#19026 = VERTEX_POINT ( 'NONE', #17632 ) ;
#19027 = DIRECTION ( 'NONE',  ( -1.000000000000000000, 0.000000000000000000, 0.000000000000000000 ) ) ;
#19028 = DIRECTION ( 'NONE',  ( -1.224646799147353207E-16, -1.349345573449484691E-32, 1.000000000000000000 ) ) ;
#19029 = AXIS2_PLACEMENT_3D ( 'NONE', #28022, #7840, #5381 ) ;
#19030 = AXIS2_PLACEMENT_3D ( 'NONE', #17914, #29746, #27930 ) ;
#19031 = ORIENTED_EDGE ( 'NONE', *, *, #26381, .F. ) ;
#19032 = EDGE_LOOP ( 'NONE', ( #21470, #4066, #21934, #15046 ) ) ;
#19033 = FACE_OUTER_BOUND ( 'NONE', #23607, .T. ) ;
#19034 = CARTESIAN_POINT ( 'NONE',  ( 21.09785597605720397, -16.72540370141334520, -37.25069200549950210 ) ) ;
#19035 = AXIS2_PLACEMENT_3D ( 'NONE', #884, #5656, #8754 ) ;
#19036 = CARTESIAN_POINT ( 'NONE',  ( -9.728297238921268075, -5.935454207752198563, 106.7470117857220373 ) ) ;
#19037 = ORIENTED_EDGE ( 'NONE', *, *, #17857, .F. ) ;
#19038 = AXIS2_PLACEMENT_3D ( 'NONE', #17773, #27136, #20236 ) ;
#19039 = CARTESIAN_POINT ( 'NONE',  ( -7.926226286961589373, 7.326690775934350697, -4.556490565496920553 ) ) ;
#19040 = DIRECTION ( 'NONE',  ( 0.000000000000000000, 0.000000000000000000, 1.000000000000000000 ) ) ;
#19041 = CIRCLE ( 'NONE', #26383, 2.500000000000002220 ) ;
#19042 = VERTEX_POINT ( 'NONE', #5337 ) ;
#19043 = CARTESIAN_POINT ( 'NONE',  ( -42.38687957179150345, 4.148162238788003719, 57.04930799450051637 ) ) ;
#19044 = CARTESIAN_POINT ( 'NONE',  ( 47.23302798462060537, 27.88121246473837544, 44.44659793406428605 ) ) ;
#19045 = EDGE_CURVE ( 'NONE', #31503, #19462, #10775, .T. ) ;
#19046 = CARTESIAN_POINT ( 'NONE',  ( 21.09785597605719332, -6.704410789454799513, -20.27960450816445359 ) ) ;
#19047 = ORIENTED_EDGE ( 'NONE', *, *, #15045, .T. ) ;
#19048 = DIRECTION ( 'NONE',  ( -1.101824276508909887E-16, 1.000000000000000000, -0.000000000000000000 ) ) ;
#19049 = EDGE_CURVE ( 'NONE', #4178, #19268, #20415, .T. ) ;
#19050 = CARTESIAN_POINT ( 'NONE',  ( 21.09785597605719332, -15.93545420775219945, 47.04930799450051637 ) ) ;
#19051 = CYLINDRICAL_SURFACE ( 'NONE', #13148, 2.000000000000001776 ) ;
#19052 = CARTESIAN_POINT ( 'NONE',  ( 49.49063479933183629, 28.09951373492759430, 47.17357720316391578 ) ) ;
#19053 = EDGE_CURVE ( 'NONE', #5246, #8335, #7318, .T. ) ;
#19054 = ORIENTED_EDGE ( 'NONE', *, *, #3172, .T. ) ;
#19055 = TOROIDAL_SURFACE ( 'NONE', #15936, 12.40141737965280200, 0.1249999999999999445 ) ;
#19056 = DIRECTION ( 'NONE',  ( 1.000000000000000000, 0.000000000000000000, 0.000000000000000000 ) ) ;
#19057 = DIRECTION ( 'NONE',  ( 0.8746197071393929656, -0.4848096202463424986, 7.034541100025353118E-15 ) ) ;
#19058 = CARTESIAN_POINT ( 'NONE',  ( 75.39785597605721534, 14.66454579224779842, 47.04930799450051637 ) ) ;
#19059 = EDGE_CURVE ( 'NONE', #15022, #27344, #10266, .T. ) ;
#19060 = LINE ( 'NONE', #6608, #24869 ) ;
#19061 = EDGE_CURVE ( 'NONE', #7489, #16711, #11297, .T. ) ;
#19062 = DIRECTION ( 'NONE',  ( 0.000000000000000000, -1.000000000000000000, 0.000000000000000000 ) ) ;
#19063 = CARTESIAN_POINT ( 'NONE',  ( 13.47645946438859355, -13.74047052604243646, 104.8978920147615810 ) ) ;
#19064 = DIRECTION ( 'NONE',  ( 0.000000000000000000, 1.000000000000000000, -0.000000000000000000 ) ) ;
#19065 = DIRECTION ( 'NONE',  ( -1.101824276508909887E-16, 1.000000000000000000, -0.000000000000000000 ) ) ;
#19066 = SURFACE_STYLE_FILL_AREA ( #31882 ) ;
#19067 = VERTEX_POINT ( 'NONE', #11068 ) ;
#19068 = DIRECTION ( 'NONE',  ( -1.000000000000000000, -1.101824276508909887E-16, 0.000000000000000000 ) ) ;
#19069 = CARTESIAN_POINT ( 'NONE',  ( 48.83862994770794330, 26.55457786121582231, 48.17861352429476796 ) ) ;
#19070 = CARTESIAN_POINT ( 'NONE',  ( 47.09785597605719687, 30.56554579224779644, 47.04930799450078638 ) ) ;
#19071 = CARTESIAN_POINT ( 'NONE',  ( 21.09992658989238734, 31.46183152705961561, 47.04930799450051637 ) ) ;
#19072 = CIRCLE ( 'NONE', #15952, 2.000000000000001776 ) ;
#19073 = ORIENTED_EDGE ( 'NONE', *, *, #12361, .F. ) ;
#19074 = CARTESIAN_POINT ( 'NONE',  ( -39.55421745345908846, -5.936056828695301490, 77.94890933298111690 ) ) ;
#19075 = DIRECTION ( 'NONE',  ( 0.000000000000000000, 0.000000000000000000, -1.000000000000000000 ) ) ;
#19076 = CARTESIAN_POINT ( 'NONE',  ( 8.823509210239560474, 29.34164230456639899, 47.04930799450051637 ) ) ;
#19077 = ORIENTED_EDGE ( 'NONE', *, *, #21024, .T. ) ;
#19079 = TOROIDAL_SURFACE ( 'NONE', #27490, 29.50000000000000355, 2.000000000000001776 ) ;
#19078 = DIRECTION ( 'NONE',  ( -1.101824276508909887E-16, 1.000000000000000000, -0.000000000000000000 ) ) ;
#19080 = CARTESIAN_POINT ( 'NONE',  ( -42.60588768478345401, 14.57151196022700113, 37.04930799450052348 ) ) ;
#19081 = AXIS2_PLACEMENT_3D ( 'NONE', #10580, #13365, #25505 ) ;
#19082 = CARTESIAN_POINT ( 'NONE',  ( 46.24715649518903149, 23.24793988701932435, 47.51120522962222736 ) ) ;
#19083 = DIRECTION ( 'NONE',  ( -1.000000000000000000, 0.000000000000000000, 0.000000000000000000 ) ) ;
#19084 = AXIS2_PLACEMENT_3D ( 'NONE', #25614, #15766, #3284 ) ;
#19085 = ORIENTED_EDGE ( 'NONE', *, *, #32211, .T. ) ;
#19086 = CARTESIAN_POINT ( 'NONE',  ( 33.72499318558949000, 38.56284415653841791, 47.04930799450051637 ) ) ;
#19087 = EDGE_LOOP ( 'NONE', ( #21444, #1633 ) ) ;
#19088 = ORIENTED_EDGE ( 'NONE', *, *, #24603, .T. ) ;
#19089 = ADVANCED_FACE ( 'NONE', ( #6128 ), #28079, .T. ) ;
#19090 = CARTESIAN_POINT ( 'NONE',  ( 21.09992658989239089, 26.59164230456639899, 47.04930799450051637 ) ) ;
#19091 = CIRCLE ( 'NONE', #7076, 0.1250000000000001110 ) ;
#19092 = CARTESIAN_POINT ( 'NONE',  ( 21.09785597605719332, 34.11266481626051217, 47.04930799450051637 ) ) ;
#19093 = CARTESIAN_POINT ( 'NONE',  ( -29.41290960217035533, 10.34548297403109807, 72.88772139469026001 ) ) ;
#19094 = CIRCLE ( 'NONE', #13906, 70.59901951359279337 ) ;
#19095 = CARTESIAN_POINT ( 'NONE',  ( 81.70930933238793159, -5.935454207752202116, 77.87546120947918382 ) ) ;
#19096 = CIRCLE ( 'NONE', #16486, 12.27641737965280555 ) ;
#19097 = EDGE_CURVE ( 'NONE', #18749, #26804, #23690, .T. ) ;
#19098 = ORIENTED_EDGE ( 'NONE', *, *, #30736, .T. ) ;
#19099 = CARTESIAN_POINT ( 'NONE',  ( 8.482002859293789498, 30.71664230456641675, 47.04930799450051637 ) ) ;
#19100 = ORIENTED_EDGE ( 'NONE', *, *, #23669, .F. ) ;
#19101 = AXIS2_PLACEMENT_3D ( 'NONE', #8504, #5559, #13438 ) ;
#19102 = EDGE_CURVE ( 'NONE', #28361, #5841, #21267, .T. ) ;
#19103 = CYLINDRICAL_SURFACE ( 'NONE', #4689, 12.62506659569710266 ) ;
#19104 = CARTESIAN_POINT ( 'NONE',  ( 0.6836613156275018754, 11.92558985988973497, 99.04321908912905315 ) ) ;
#19105 = ORIENTED_EDGE ( 'NONE', *, *, #5574, .T. ) ;
#19106 = DIRECTION ( 'NONE',  ( -0.000000000000000000, -1.000000000000000000, -0.000000000000000000 ) ) ;
#19107 = LINE ( 'NONE', #1231, #13202 ) ;
#19108 = DIRECTION ( 'NONE',  ( 1.000000000000000000, 6.722685822323786766E-17, 0.000000000000000000 ) ) ;
#19109 = ORIENTED_EDGE ( 'NONE', *, *, #5945, .T. ) ;
#19110 = CARTESIAN_POINT ( 'NONE',  ( 47.05339576314583638, 22.89977464660286444, 45.18578914680342251 ) ) ;
#19111 = CARTESIAN_POINT ( 'NONE',  ( 21.09992658989239089, 29.34164230456639899, 47.04930799450051637 ) ) ;
#19112 = DIRECTION ( 'NONE',  ( -1.224646799147353207E-16, -1.349345573449484691E-32, 1.000000000000000000 ) ) ;
#19113 = CARTESIAN_POINT ( 'NONE',  ( 21.09992658989239089, 27.34164230456639544, 47.04930799450051637 ) ) ;
#19114 = CARTESIAN_POINT ( 'NONE',  ( 21.09992658989238734, 38.56284415653841791, 47.04930799450051637 ) ) ;
#19115 = ORIENTED_EDGE ( 'NONE', *, *, #24865, .T. ) ;
#19116 = DIRECTION ( 'NONE',  ( -1.000000000000000000, -1.101824276508909887E-16, 0.000000000000000000 ) ) ;
#19117 = CARTESIAN_POINT ( 'NONE',  ( -30.88776590959009738, 11.92558985988972964, 26.61401058482698545 ) ) ;
#19118 = VERTEX_POINT ( 'NONE', #10590 ) ;
#19119 = FACE_OUTER_BOUND ( 'NONE', #12323, .T. ) ;
#19120 = CARTESIAN_POINT ( 'NONE',  ( 8.474859994195282908, 38.56284415653841791, 47.04930799450051637 ) ) ;
#19121 = ORIENTED_EDGE ( 'NONE', *, *, #28400, .F. ) ;
#19122 = AXIS2_PLACEMENT_3D ( 'NONE', #11291, #14241, #19139 ) ;
#19123 =( BOUNDED_CURVE ( )  B_SPLINE_CURVE ( 3, ( #5921, #6077, #16238, #8068 ),
 .UNSPECIFIED., .F., .F. ) 
 B_SPLINE_CURVE_WITH_KNOTS ( ( 4, 4 ),
 ( -8.881784197001252323E-16, 1.570796326794894782 ),
 .UNSPECIFIED. ) 
 CURVE ( )  GEOMETRIC_REPRESENTATION_ITEM ( )  RATIONAL_B_SPLINE_CURVE ( ( 1.000000000000000000, 0.8047378541243652705, 0.8047378541243652705, 1.000000000000000000 ) ) 
 REPRESENTATION_ITEM ( '' )  );
#19124 = ORIENTED_EDGE ( 'NONE', *, *, #9040, .T. ) ;
#19125 = CIRCLE ( 'NONE', #14959, 0.9031915329475500576 ) ;
#19126 = CIRCLE ( 'NONE', #19652, 2.500000000000002220 ) ;
#19127 = AXIS2_PLACEMENT_3D ( 'NONE', #17097, #26183, #18784 ) ;
#19128 = CIRCLE ( 'NONE', #18108, 0.1000000000000028644 ) ;
#19129 = VERTEX_POINT ( 'NONE', #1192 ) ;
#19130 = CARTESIAN_POINT ( 'NONE',  ( -40.18454328187963398, 7.548069831825862330, 60.54930799450051637 ) ) ;
#19131 = ADVANCED_FACE ( 'NONE', ( #11219 ), #28143, .T. ) ;
#19132 = EDGE_LOOP ( 'NONE', ( #12526, #23584 ) ) ;
#19133 = DIRECTION ( 'NONE',  ( -0.4544104193609917464, 0.000000000000000000, -0.8907924397839080966 ) ) ;
#19134 = EDGE_CURVE ( 'NONE', #22868, #13543, #8697, .T. ) ;
#19135 = EDGE_CURVE ( 'NONE', #18170, #26418, #67, .T. ) ;
#19136 = CIRCLE ( 'NONE', #14978, 12.62506659569710266 ) ;
#19137 = LINE ( 'NONE', #14240, #27190 ) ;
#19138 = ADVANCED_FACE ( 'NONE', ( #28462 ), #23841, .F. ) ;
#19139 = DIRECTION ( 'NONE',  ( -1.000000000000000000, -1.101824276508909887E-16, 0.000000000000000000 ) ) ;
#19140 = CARTESIAN_POINT ( 'NONE',  ( 21.09785597605719332, 45.28940914544685370, 47.04930799450051637 ) ) ;
#19141 = ADVANCED_FACE ( 'NONE', ( #5646 ), #1043, .F. ) ;
#19142 = EDGE_CURVE ( 'NONE', #32001, #28526, #24935, .T. ) ;
#19143 = CARTESIAN_POINT ( 'NONE',  ( 49.44739180854976013, 26.67786309983298665, 47.17133137409169308 ) ) ;
#19144 = ORIENTED_EDGE ( 'NONE', *, *, #27599, .F. ) ;
#19145 = CARTESIAN_POINT ( 'NONE',  ( 33.37634396954519644, 31.59164230456639544, 47.04930799450051637 ) ) ;
#19146 = ORIENTED_EDGE ( 'NONE', *, *, #7356, .F. ) ;
#19148 = DIRECTION ( 'NONE',  ( -0.9612616959383210036, -0.2756373558169918914, -9.967286752943808104E-15 ) ) ;
#19147 = AXIS2_PLACEMENT_3D ( 'NONE', #25668, #3496, #31247 ) ;
#19149 = ORIENTED_EDGE ( 'NONE', *, *, #7275, .F. ) ;
#19150 = CARTESIAN_POINT ( 'NONE',  ( 47.09785597605719687, 29.86454579224779948, 47.04930799450078638 ) ) ;
#19151 = PLANE ( 'NONE',  #13691 ) ;
#19152 = CARTESIAN_POINT ( 'NONE',  ( -40.64522151305494191, 6.818818762547858014, 39.52645928364133709 ) ) ;
#19153 = AXIS2_PLACEMENT_3D ( 'NONE', #22674, #12842, #2333 ) ;
#19154 = CARTESIAN_POINT ( 'NONE',  ( 41.51205063648688309, 1.925589859889728972, -37.95069200549950494 ) ) ;
#19155 = DIRECTION ( 'NONE',  ( 1.000000000000000000, 0.000000000000000000, 0.000000000000000000 ) ) ;
#19156 = CARTESIAN_POINT ( 'NONE',  ( 45.73035263060504718, 26.53954579807170688, 44.36855633853329550 ) ) ;
#19157 = LINE ( 'NONE', #31809, #27309 ) ;
#19158 = CARTESIAN_POINT ( 'NONE',  ( 8.474859994195281132, 38.56284415653841791, 47.04930799450051637 ) ) ;
#19159 = ORIENTED_EDGE ( 'NONE', *, *, #12988, .T. ) ;
#19160 = DIRECTION ( 'NONE',  ( -1.000000000000000000, 0.000000000000000000, 0.000000000000000000 ) ) ;
#19161 = LINE ( 'NONE', #21299, #1988 ) ;
#19162 = FACE_OUTER_BOUND ( 'NONE', #23751, .T. ) ;
#19163 = AXIS2_PLACEMENT_3D ( 'NONE', #984, #8701, #11010 ) ;
#19164 = CARTESIAN_POINT ( 'NONE',  ( 48.41187465712202709, 22.98765316579147111, 46.37900169951733886 ) ) ;
#19165 = LINE ( 'NONE', #6222, #27209 ) ;
#19166 = ORIENTED_EDGE ( 'NONE', *, *, #7127, .F. ) ;
#19167 = DIRECTION ( 'NONE',  ( -1.101824276508909887E-16, 1.000000000000000000, -0.000000000000000000 ) ) ;
#19168 = VERTEX_POINT ( 'NONE', #3825 ) ;
#19169 = CARTESIAN_POINT ( 'NONE',  ( 33.72499318558949000, 38.56284415653841791, 47.04930799450051637 ) ) ;
#19170 = FACE_OUTER_BOUND ( 'NONE', #17875, .T. ) ;
#19171 = ORIENTED_EDGE ( 'NONE', *, *, #19006, .T. ) ;
#19172 = EDGE_CURVE ( 'NONE', #20563, #15480, #30607, .T. ) ;
#19173 = VECTOR ( 'NONE', #17397, 1000.000000000000114 ) ;
#19174 = STYLED_ITEM ( 'NONE', ( #15459 ), #8462 ) ;
#19175 = ORIENTED_EDGE ( 'NONE', *, *, #14875, .T. ) ;
#19176 = FACE_OUTER_BOUND ( 'NONE', #28779, .T. ) ;
#19177 = DIRECTION ( 'NONE',  ( 0.2756373558169974980, -0.9612616959383193382, 8.979771562518858393E-33 ) ) ;
#19178 = FACE_OUTER_BOUND ( 'NONE', #435, .T. ) ;
#19179 = AXIS2_PLACEMENT_3D ( 'NONE', #22869, #2844, #30267 ) ;
#19180 = ORIENTED_EDGE ( 'NONE', *, *, #3576, .T. ) ;
#19181 = CARTESIAN_POINT ( 'NONE',  ( 45.47421713364555274, 22.88065857334294861, 45.99599230681428708 ) ) ;
#19182 = ADVANCED_FACE ( 'NONE', ( #18114 ), #30567, .T. ) ;
#19183 = CARTESIAN_POINT ( 'NONE',  ( -35.40773169500607054, 11.64114591743160076, 41.11337043081405795 ) ) ;
#19184 = DIRECTION ( 'NONE',  ( -0.000000000000000000, -1.000000000000000000, 0.000000000000000000 ) ) ;
#19185 = ADVANCED_FACE ( 'NONE', ( #12026 ), #16608, .T. ) ;
#19186 = ORIENTED_EDGE ( 'NONE', *, *, #8416, .F. ) ;
#19187 = FACE_OUTER_BOUND ( 'NONE', #12532, .T. ) ;
#19188 = ORIENTED_EDGE ( 'NONE', *, *, #11685, .F. ) ;
#19189 = DIRECTION ( 'NONE',  ( 0.2756373558169961102, -0.9612616959383197823, 0.000000000000000000 ) ) ;
#19190 = LINE ( 'NONE', #14292, #31591 ) ;
#19191 = LINE ( 'NONE', #29219, #4743 ) ;
#19192 = DIRECTION ( 'NONE',  ( 1.000000000000000000, 0.000000000000000000, 0.000000000000000000 ) ) ;
#19193 = ORIENTED_EDGE ( 'NONE', *, *, #23615, .T. ) ;
#19194 = ORIENTED_EDGE ( 'NONE', *, *, #30953, .T. ) ;
#19195 = CARTESIAN_POINT ( 'NONE',  ( 21.09992658989238734, 38.56284415653841791, 47.04930799450051637 ) ) ;
#19196 = CIRCLE ( 'NONE', #31784, 0.1250000000000001110 ) ;
#19197 = DIRECTION ( 'NONE',  ( 0.9996573249755574819, 1.344306794811909066E-16, -0.02617694830786587712 ) ) ;
#19198 = FACE_OUTER_BOUND ( 'NONE', #6422, .T. ) ;
#19199 = ORIENTED_EDGE ( 'NONE', *, *, #23938, .F. ) ;
#19200 = CARTESIAN_POINT ( 'NONE',  ( -12.54358740205593215, -1.580002914024313254, -7.565473790375000895 ) ) ;
#19201 = CARTESIAN_POINT ( 'NONE',  ( 56.61384086331115384, -13.74047052604243646, 0.7550407962218190772 ) ) ;
#19202 = ORIENTED_EDGE ( 'NONE', *, *, #522, .T. ) ;
#19203 = DIRECTION ( 'NONE',  ( -0.000000000000000000, -1.000000000000000000, -0.000000000000000000 ) ) ;
#19204 = CARTESIAN_POINT ( 'NONE',  ( -40.82286654448606811, 10.16735592115171549, 37.04930799450052348 ) ) ;
#19205 = EDGE_CURVE ( 'NONE', #1940, #13978, #25975, .T. ) ;
#19206 = CIRCLE ( 'NONE', #8216, 56.65825807113184709 ) ;
#19207 = DIRECTION ( 'NONE',  ( 1.000000000000000000, 0.000000000000000000, 0.000000000000000000 ) ) ;
#19208 = EDGE_CURVE ( 'NONE', #3764, #29013, #7842, .T. ) ;
#19209 = ADVANCED_FACE ( 'NONE', ( #4635 ), #24490, .F. ) ;
#19210 = ORIENTED_EDGE ( 'NONE', *, *, #7218, .T. ) ;
#19211 = CARTESIAN_POINT ( 'NONE',  ( 8.698509210239565803, 29.84164230456639899, 47.04930799450051637 ) ) ;
#19212 = DIRECTION ( 'NONE',  ( -1.000000000000000000, 0.000000000000000000, 0.000000000000000000 ) ) ;
#19213 = VECTOR ( 'NONE', #6622, 1000.000000000000000 ) ;
#19214 = DIRECTION ( 'NONE',  ( -0.9612616959383221138, -0.2756373558169876170, 0.000000000000000000 ) ) ;
#19215 = CARTESIAN_POINT ( 'NONE',  ( 44.70507715278255745, 27.74951373492759643, 46.92503878583764987 ) ) ;
#19216 = ORIENTED_EDGE ( 'NONE', *, *, #20678, .F. ) ;
#19217 = DIRECTION ( 'NONE',  ( 0.4848096202463430537, 0.8746197071393926326, 1.323854077651070671E-16 ) ) ;
#19218 = CARTESIAN_POINT ( 'NONE',  ( -43.64073206722599707, 1.267352857069778960, 34.64930799450052490 ) ) ;
#19219 = EDGE_CURVE ( 'NONE', #11938, #5749, #9240, .T. ) ;
#19220 = CARTESIAN_POINT ( 'NONE',  ( 54.27408594025197175, -4.576799740321103371, -8.853384888801278052 ) ) ;
#19221 = FACE_OUTER_BOUND ( 'NONE', #14238, .T. ) ;
#19222 = DIRECTION ( 'NONE',  ( 0.000000000000000000, 0.000000000000000000, 1.000000000000000000 ) ) ;
#19223 = CARTESIAN_POINT ( 'NONE',  ( 6.001413532006956153, -13.74047052604243468, 103.4110129320797853 ) ) ;
#19224 = DIRECTION ( 'NONE',  ( -0.9612616959383200044, -0.2756373558169954996, 1.660411357259285896E-16 ) ) ;
#19225 = CARTESIAN_POINT ( 'NONE',  ( 21.09992658989238734, 31.34164230456639544, 47.04930799450051637 ) ) ;
#19226 =( NAMED_UNIT ( * ) PLANE_ANGLE_UNIT ( ) SI_UNIT ( $, .RADIAN. ) );
#19227 = ORIENTED_EDGE ( 'NONE', *, *, #17621, .T. ) ;
#19228 = CARTESIAN_POINT ( 'NONE',  ( 8.732853799281734553, 38.56284415653841791, 47.04930799450051637 ) ) ;
#19229 = CARTESIAN_POINT ( 'NONE',  ( -42.38474149870877028, 15.25146566812707505, 35.54930799450051637 ) ) ;
#19230 = CARTESIAN_POINT ( 'NONE',  ( 40.09785597605721108, -5.098646251524523443, 47.04930799450052348 ) ) ;
#19231 = CIRCLE ( 'NONE', #6148, 1.500000000000001332 ) ;
#19232 = LINE ( 'NONE', #16780, #9484 ) ;
#19233 = EDGE_LOOP ( 'NONE', ( #27245, #26405 ) ) ;
#19234 = CARTESIAN_POINT ( 'NONE',  ( -39.55199796652554767, -5.935626912768316998, 77.88283516045706278 ) ) ;
#19235 = AXIS2_PLACEMENT_3D ( 'NONE', #31311, #31635, #23913 ) ;
#19236 = CARTESIAN_POINT ( 'NONE',  ( -44.35518986140444753, -4.284653979202247776, 42.04930799450063716 ) ) ;
#19237 = CYLINDRICAL_SURFACE ( 'NONE', #9097, 27.99999999999999645 ) ;
#19238 = ADVANCED_FACE ( 'NONE', ( #2008 ), #23359, .T. ) ;
#19239 = ORIENTED_EDGE ( 'NONE', *, *, #27431, .T. ) ;
#19240 = ORIENTED_EDGE ( 'NONE', *, *, #27994, .F. ) ;
#19241 = DIRECTION ( 'NONE',  ( -0.000000000000000000, -1.000000000000000000, -0.000000000000000000 ) ) ;
#19242 = FACE_OUTER_BOUND ( 'NONE', #12228, .T. ) ;
#19243 = AXIS2_PLACEMENT_3D ( 'NONE', #2981, #209, #10228 ) ;
#19244 = DIRECTION ( 'NONE',  ( 0.000000000000000000, 0.000000000000000000, 1.000000000000000000 ) ) ;
#19245 = ADVANCED_FACE ( 'NONE', ( #6773 ), #30707, .T. ) ;
#19246 = DIRECTION ( 'NONE',  ( -1.101824276508909887E-16, 1.000000000000000000, -0.000000000000000000 ) ) ;
#19247 = EDGE_LOOP ( 'NONE', ( #21892, #9898, #25898, #9913, #13017 ) ) ;
#19248 = CARTESIAN_POINT ( 'NONE',  ( 46.63102355535853150, 29.41114986400162934, 49.25898951255931735 ) ) ;
#19249 = ORIENTED_EDGE ( 'NONE', *, *, #7805, .T. ) ;
#19250 = EDGE_CURVE ( 'NONE', #18749, #15685, #27035, .T. ) ;
#19251 = EDGE_CURVE ( 'NONE', #22420, #22576, #1871, .T. ) ;
#19252 = TOROIDAL_SURFACE ( 'NONE', #13512, 12.40141737965280022, 0.1249999999999992228 ) ;
#19253 = ORIENTED_EDGE ( 'NONE', *, *, #16334, .F. ) ;
#19254 = ADVANCED_FACE ( 'NONE', ( #14006 ), #4144, .T. ) ;
#19255 = CARTESIAN_POINT ( 'NONE',  ( 52.21187923486668581, -5.935340315990531579, 107.6772108465075490 ) ) ;
#19256 = CARTESIAN_POINT ( 'NONE',  ( -38.36853489569023168, 7.065850718397949315, 32.14930799450051779 ) ) ;
#19257 = CARTESIAN_POINT ( 'NONE',  ( -31.41618342396850494, 0.9942232071982006758, 79.85214699334892430 ) ) ;
#19258 = CARTESIAN_POINT ( 'NONE',  ( 81.65861757311864721, -5.935454078358223917, 78.02743665865710909 ) ) ;
#19259 = CIRCLE ( 'NONE', #5143, 0.1249999999999983763 ) ;
#19260 = VECTOR ( 'NONE', #31633, 1000.000000000000000 ) ;
#19261 = VERTEX_POINT ( 'NONE', #31884 ) ;
#19262 = CARTESIAN_POINT ( 'NONE',  ( -40.69571722278732295, 6.786566810383045656, 34.64930799450051779 ) ) ;
#19263 = EDGE_LOOP ( 'NONE', ( #15405, #14592, #12166, #22625 ) ) ;
#19264 = FACE_OUTER_BOUND ( 'NONE', #29777, .T. ) ;
#19265 = CIRCLE ( 'NONE', #24526, 12.27641737965282154 ) ;
#19266 = FACE_OUTER_BOUND ( 'NONE', #28065, .T. ) ;
#19267 = DIRECTION ( 'NONE',  ( 0.000000000000000000, 0.000000000000000000, 1.000000000000000000 ) ) ;
#19268 = VERTEX_POINT ( 'NONE', #2501 ) ;
#19269 = DIRECTION ( 'NONE',  ( 1.000000000000000000, 0.000000000000000000, 0.000000000000000000 ) ) ;
#19270 = FACE_OUTER_BOUND ( 'NONE', #31991, .T. ) ;
#19271 = CARTESIAN_POINT ( 'NONE',  ( -40.58094809379417001, 7.465224162809761310, 53.91088180535781760 ) ) ;
#19272 = CARTESIAN_POINT ( 'NONE',  ( 21.09785597605720753, 17.16467605102632632, 47.04930799450052348 ) ) ;
#19273 = CARTESIAN_POINT ( 'NONE',  ( 33.37634396954518934, 31.84164230456639544, 47.04930799450051637 ) ) ;
#19274 = CIRCLE ( 'NONE', #6711, 2.500000000000002220 ) ;
#19275 = FACE_OUTER_BOUND ( 'NONE', #31822, .T. ) ;
#19276 = CARTESIAN_POINT ( 'NONE',  ( -42.36153388572594736, 13.68895619636815653, 54.64930799450051779 ) ) ;
#19277 = ORIENTED_EDGE ( 'NONE', *, *, #19976, .T. ) ;
#19278 = CARTESIAN_POINT ( 'NONE',  ( -40.01196617104008624, 7.363926680071349651, 35.23477324418088585 ) ) ;
#19279 = CARTESIAN_POINT ( 'NONE',  ( -40.50146157965988891, 7.595301493077381672, 35.64930799450052490 ) ) ;
#19280 = EDGE_CURVE ( 'NONE', #16708, #1140, #14824, .T. ) ;
#19281 = ORIENTED_EDGE ( 'NONE', *, *, #21424, .T. ) ;
#19282 = FACE_OUTER_BOUND ( 'NONE', #9422, .T. ) ;
#19283 = B_SPLINE_CURVE_WITH_KNOTS ( 'NONE', 3,
 ( #10188, #22810, #30369, #8362, #324, #5581, #25439, #27741, #18359, #15107, #20672, #10345 ),
 .UNSPECIFIED., .F., .F.,
 ( 4, 2, 2, 2, 2, 4 ),
 ( 0.000000000000000000, 7.988424390472266816E-05, 0.0001597684878094453363, 0.0001997106097618206498, 0.0002396527317141959905, 0.0003195369756189209219 ),
 .UNSPECIFIED. ) ;
#19284 = EDGE_CURVE ( 'NONE', #29304, #28041, #13924, .T. ) ;
#19285 = CARTESIAN_POINT ( 'NONE',  ( -63.90214402394282445, 11.92558985988973674, 54.04930799450053769 ) ) ;
#19286 = ORIENTED_EDGE ( 'NONE', *, *, #2797, .F. ) ;
#19287 = ORIENTED_EDGE ( 'NONE', *, *, #29853, .F. ) ;
#19288 = CIRCLE ( 'NONE', #5156, 0.1250000000000001110 ) ;
#19289 = UNCERTAINTY_MEASURE_WITH_UNIT (LENGTH_MEASURE( 1.000000000000000082E-05 ), #28350, 'distance_accuracy_value', 'NONE');
#19290 = CIRCLE ( 'NONE', #27171, 55.85791022362053582 ) ;
#19291 = EDGE_CURVE ( 'NONE', #12553, #24565, #305, .T. ) ;
#19292 = AXIS2_PLACEMENT_3D ( 'NONE', #28559, #3598, #6389 ) ;
#19293 = ORIENTED_EDGE ( 'NONE', *, *, #25730, .F. ) ;
#19294 = AXIS2_PLACEMENT_3D ( 'NONE', #16131, #3665, #28775 ) ;
#19295 = CIRCLE ( 'NONE', #5167, 12.36707279061065101 ) ;
#19296 = AXIS2_PLACEMENT_3D ( 'NONE', #18575, #30599, #15640 ) ;
#19297 = DIRECTION ( 'NONE',  ( 1.000000000000000000, 0.000000000000000000, -1.224646799147353207E-16 ) ) ;
#19298 = VERTEX_POINT ( 'NONE', #5459 ) ;
#19299 = VERTEX_POINT ( 'NONE', #24990 ) ;
#19300 = DIRECTION ( 'NONE',  ( -1.188208965918165239E-16, -1.880121038077812885E-16, -1.000000000000000000 ) ) ;
#19301 = CARTESIAN_POINT ( 'NONE',  ( 21.09992658989239089, 25.59164230456639899, 47.04930799450051637 ) ) ;
#19302 = CARTESIAN_POINT ( 'NONE',  ( -40.28779227465695101, 2.984619150196775372, 39.04930799450052348 ) ) ;
#19303 = CARTESIAN_POINT ( 'NONE',  ( -40.50726676055796105, 7.559560307024984382, 53.81156708294278701 ) ) ;
#19304 = CARTESIAN_POINT ( 'NONE',  ( 45.38854177497844944, 26.96952976649965450, 45.94041160078741370 ) ) ;
#19305 = EDGE_LOOP ( 'NONE', ( #20816, #16054, #7829, #13782, #825 ) ) ;
#19306 = CARTESIAN_POINT ( 'NONE',  ( 33.50134396954519644, 31.59164230456639544, 47.04930799450051637 ) ) ;
#19307 = EDGE_LOOP ( 'NONE', ( #3678, #29155, #28999, #13293 ) ) ;
#19308 = CARTESIAN_POINT ( 'NONE',  ( -12.64026357700385716, -2.474457146986663414, -7.147442258105406232 ) ) ;
#19309 = CIRCLE ( 'NONE', #26684, 0.1000000000000020595 ) ;
#19310 = ORIENTED_EDGE ( 'NONE', *, *, #29461, .F. ) ;
#19311 = CARTESIAN_POINT ( 'NONE',  ( 48.93186884373860579, 29.49610055912359741, 48.21814732446082985 ) ) ;
#19312 = DIRECTION ( 'NONE',  ( -0.9612616959383206705, -0.2756373558169931681, 1.660411357259282445E-16 ) ) ;
#19313 = CIRCLE ( 'NONE', #25635, 1.524998423334080533 ) ;
#19314 = DIRECTION ( 'NONE',  ( -1.000000000000000000, 0.000000000000000000, 0.000000000000000000 ) ) ;
#19315 = CARTESIAN_POINT ( 'NONE',  ( 47.59785597605720397, 13.86454579224779948, 47.04930799450052348 ) ) ;
#19316 = DIRECTION ( 'NONE',  ( 0.8746197071393926326, -0.4848096202463430537, -8.676864087101709653E-18 ) ) ;
#19317 = CONICAL_SURFACE ( 'NONE', #28750, 0.9031915329475502796, 0.7853981633974456145 ) ;
#19318 = CARTESIAN_POINT ( 'NONE',  ( 44.91142894931555674, 25.19787913140504543, 45.63089057098605394 ) ) ;
#19319 =( BOUNDED_CURVE ( )  B_SPLINE_CURVE ( 2, ( #28580, #18225, #20860 ),
 .UNSPECIFIED., .F., .T. ) 
 B_SPLINE_CURVE_WITH_KNOTS ( ( 3, 3 ),
 ( 0.8928571440184154273, 0.8999500719669653037 ),
 .UNSPECIFIED. ) 
 CURVE ( )  GEOMETRIC_REPRESENTATION_ITEM ( )  RATIONAL_B_SPLINE_CURVE ( ( 0.9330127018922200755, 0.9330127057854562533, 0.9567921774292901249 ) ) 
 REPRESENTATION_ITEM ( '' )  );
#19320 = CARTESIAN_POINT ( 'NONE',  ( 21.09785597605719332, 30.56454579224779522, 47.04930799450051637 ) ) ;
#19321 = DIRECTION ( 'NONE',  ( -0.000000000000000000, -1.000000000000000000, 0.000000000000000000 ) ) ;
#19322 = EDGE_LOOP ( 'NONE', ( #14756, #21789 ) ) ;
#19323 = CARTESIAN_POINT ( 'NONE',  ( 21.09992658989238734, 32.47145308207317527, 47.04930799450051637 ) ) ;
#19324 = CARTESIAN_POINT ( 'NONE',  ( 21.09785597605719332, 44.06454579224779877, 48.04930799450048795 ) ) ;
#19325 = DIRECTION ( 'NONE',  ( -7.588956326749211550E-18, 4.206627182996912454E-18, -1.000000000000000000 ) ) ;
#19326 = CIRCLE ( 'NONE', #14114, 45.49665035954053138 ) ;
#19327 = LINE ( 'NONE', #29352, #7985 ) ;
#19328 = DIRECTION ( 'NONE',  ( 0.8643320973212949010, 0.2419218955996663700, -0.4409124878812526460 ) ) ;
#19329 = ORIENTED_EDGE ( 'NONE', *, *, #6930, .T. ) ;
#19330 = CARTESIAN_POINT ( 'NONE',  ( 33.72499318558949710, 25.84184655352419213, 47.04930799450051637 ) ) ;
#19331 = EDGE_LOOP ( 'NONE', ( #17186, #5617, #16667, #18705 ) ) ;
#19332 = CARTESIAN_POINT ( 'NONE',  ( -40.73728033978215990, 8.177846351970792682, 59.56562166518216372 ) ) ;
#19333 = DIRECTION ( 'NONE',  ( -1.000000000000000000, 0.000000000000000000, 0.000000000000000000 ) ) ;
#19334 = EDGE_CURVE ( 'NONE', #7595, #5139, #4500, .T. ) ;
#19335 = EDGE_LOOP ( 'NONE', ( #29452, #27663, #10878, #14451, #27938, #28955, #26267, #6055, #5939, #29372, #7545, #787, #22326, #3571, #28217, #5513, #2550, #11477, #3030, #18597, #8724, #29119 ) ) ;
#19336 = EDGE_CURVE ( 'NONE', #21342, #23289, #12912, .T. ) ;
#19337 = EDGE_CURVE ( 'NONE', #23072, #7677, #7597, .T. ) ;
#19338 = AXIS2_PLACEMENT_3D ( 'NONE', #26996, #14038, #29136 ) ;
#19339 = TOROIDAL_SURFACE ( 'NONE', #8338, 58.03288776117695846, 0.1999999999999970968 ) ;
#19340 = ORIENTED_EDGE ( 'NONE', *, *, #24432, .F. ) ;
#19341 = CARTESIAN_POINT ( 'NONE',  ( 21.09785597605719332, 30.56454579224779522, 47.04930799450051637 ) ) ;
#19342 = DIRECTION ( 'NONE',  ( 1.000000000000000000, 0.000000000000000000, 0.000000000000000000 ) ) ;
#19343 = CARTESIAN_POINT ( 'NONE',  ( -9.902144023942796025, 14.86454579224779948, 47.04930799450052348 ) ) ;
#19344 = VECTOR ( 'NONE', #7563, 1000.000000000000000 ) ;
#19345 = VERTEX_POINT ( 'NONE', #24830 ) ;
#19346 = DIRECTION ( 'NONE',  ( -1.101824276508909887E-16, 1.000000000000000000, -0.000000000000000000 ) ) ;
#19347 = CIRCLE ( 'NONE', #5756, 12.36707279061065101 ) ;
#19348 = DIRECTION ( 'NONE',  ( -0.000000000000000000, -1.000000000000000000, 0.000000000000000000 ) ) ;
#19349 = CARTESIAN_POINT ( 'NONE',  ( -41.52218637998914375, 11.15499190493234671, 38.09144330556765112 ) ) ;
#19350 = VERTEX_POINT ( 'NONE', #22687 ) ;
#19351 = ORIENTED_EDGE ( 'NONE', *, *, #11012, .F. ) ;
#19352 = DIRECTION ( 'NONE',  ( -1.000000000000000000, 0.000000000000000000, 0.000000000000000000 ) ) ;
#19353 = ORIENTED_EDGE ( 'NONE', *, *, #26381, .T. ) ;
#19354 = DIRECTION ( 'NONE',  ( 0.000000000000000000, -0.000000000000000000, -1.000000000000000000 ) ) ;
#19355 = FACE_OUTER_BOUND ( 'NONE', #20489, .T. ) ;
#19356 = DIRECTION ( 'NONE',  ( 1.000000000000000000, 0.000000000000000000, 0.000000000000000000 ) ) ;
#19357 = SURFACE_STYLE_USAGE ( .BOTH. , #9201 ) ;
#19358 = EDGE_LOOP ( 'NONE', ( #15845, #5947, #7877, #25060, #22651, #10332 ) ) ;
#19359 = ORIENTED_EDGE ( 'NONE', *, *, #11566, .F. ) ;
#19360 = ADVANCED_FACE ( 'NONE', ( #10064 ), #357, .T. ) ;
#19361 = CARTESIAN_POINT ( 'NONE',  ( 21.09785597605720753, 17.16467605102632632, 47.04930799450052348 ) ) ;
#19362 = CARTESIAN_POINT ( 'NONE',  ( -39.59300248568538194, 7.744584186742829779, 32.04930799450052348 ) ) ;
#19363 = AXIS2_PLACEMENT_3D ( 'NONE', #4158, #18600, #31418 ) ;
#19364 = CARTESIAN_POINT ( 'NONE',  ( 21.09785597605720042, -16.93545420775220478, 47.04930799450051637 ) ) ;
#19365 = ORIENTED_EDGE ( 'NONE', *, *, #9342, .T. ) ;
#19366 = CARTESIAN_POINT ( 'NONE',  ( -8.645724211769511669, 6.334306897662572489, -4.780293558379808516 ) ) ;
#19367 = CARTESIAN_POINT ( 'NONE',  ( -40.11967773290336226, 9.763195579837789850, 35.54930799450052348 ) ) ;
#19368 = ORIENTED_EDGE ( 'NONE', *, *, #5163, .F. ) ;
#19369 = DIRECTION ( 'NONE',  ( 0.000000000000000000, 0.000000000000000000, -1.000000000000000000 ) ) ;
#19370 = CARTESIAN_POINT ( 'NONE',  ( 46.96268396749378127, 26.13121246473837544, 49.65201805493727960 ) ) ;
#19371 = CIRCLE ( 'NONE', #5750, 46.09082119073493544 ) ;
#19372 = VECTOR ( 'NONE', #4329, 1000.000000000000114 ) ;
#19373 = DIRECTION ( 'NONE',  ( 0.000000000000000000, 0.000000000000000000, -1.000000000000000000 ) ) ;
#19374 = ADVANCED_FACE ( 'NONE', ( #32222 ), #21773, .T. ) ;
#19375 = EDGE_CURVE ( 'NONE', #5070, #20563, #13425, .T. ) ;
#19376 = EDGE_CURVE ( 'NONE', #21925, #10074, #21233, .T. ) ;
#19377 = AXIS2_PLACEMENT_3D ( 'NONE', #12557, #22547, #25185 ) ;
#19378 = EDGE_CURVE ( 'NONE', #5687, #19469, #7102, .T. ) ;
#19379 = AXIS2_PLACEMENT_3D ( 'NONE', #23050, #3184, #7804 ) ;
#19380 = ORIENTED_EDGE ( 'NONE', *, *, #15375, .T. ) ;
#19381 = CARTESIAN_POINT ( 'NONE',  ( 21.09992658989239089, 27.09164230456639899, 47.04930799450051637 ) ) ;
#19382 = CARTESIAN_POINT ( 'NONE',  ( -38.96025635604170390, 15.13029464144910108, 54.64930799450051779 ) ) ;
#19383 = DIRECTION ( 'NONE',  ( -0.9612616959383205595, -0.2756373558169931681, 1.660411357259282445E-16 ) ) ;
#19384 = CARTESIAN_POINT ( 'NONE',  ( 45.38854177497844944, 25.56952976649965947, 45.94041160078741370 ) ) ;
#19385 = CIRCLE ( 'NONE', #18332, 0.4062389912925720714 ) ;
#19386 = ORIENTED_EDGE ( 'NONE', *, *, #28316, .F. ) ;
#19387 = CARTESIAN_POINT ( 'NONE',  ( 21.09785597605719332, 30.56454579224779522, 21.04930799450051282 ) ) ;
#19388 = DIRECTION ( 'NONE',  ( -0.4848096202463746951, -0.8746197071393748690, 0.000000000000000000 ) ) ;
#19389 = CARTESIAN_POINT ( 'NONE',  ( -40.23397449525940317, 6.794506605641760011, 34.64930799450051779 ) ) ;
#19390 = CIRCLE ( 'NONE', #7893, 0.1250000000000001110 ) ;
#19391 = VECTOR ( 'NONE', #23790, 1000.000000000000000 ) ;
#19392 = DIRECTION ( 'NONE',  ( -0.05186525298099629866, -6.405245952009066254E-18, 0.9986540920324801229 ) ) ;
#19393 = CARTESIAN_POINT ( 'NONE',  ( -16.40214402394279958, 13.86454579224779948, 47.04930799450052348 ) ) ;
#19394 = CARTESIAN_POINT ( 'NONE',  ( -40.51045226066063520, 7.589116544599141534, 60.22001867261916885 ) ) ;
#19395 = CARTESIAN_POINT ( 'NONE',  ( -4.704135725172196025, -13.74047052604243646, 99.38286875800066866 ) ) ;
#19396 = DIRECTION ( 'NONE',  ( 0.9761574614375593262, -0.2110602665713099957, 0.05069688703093822718 ) ) ;
#19397 = TOROIDAL_SURFACE ( 'NONE', #5270, 12.40141737965286595, 0.1249999999999979183 ) ;
#19398 = AXIS2_PLACEMENT_3D ( 'NONE', #31712, #26296, #21192 ) ;
#19399 = ORIENTED_EDGE ( 'NONE', *, *, #6520, .T. ) ;
#19400 = CIRCLE ( 'NONE', #17847, 0.1250000000000001110 ) ;
#19401 = ADVANCED_FACE ( 'NONE', ( #30245 ), #5550, .T. ) ;
#19402 = EDGE_CURVE ( 'NONE', #3968, #3369, #18104, .T. ) ;
#19403 = AXIS2_PLACEMENT_3D ( 'NONE', #17918, #23331, #30885 ) ;
#19404 = CARTESIAN_POINT ( 'NONE',  ( 45.67943855254225127, 25.37287913140503548, 49.23573502124227730 ) ) ;
#19405 = CARTESIAN_POINT ( 'NONE',  ( -29.42591059354393934, 10.36022259761711162, 21.25795413502442699 ) ) ;
#19406 = CARTESIAN_POINT ( 'NONE',  ( 52.97684575647971172, -5.738638231773880882, 104.4392655406692256 ) ) ;
#19407 = ORIENTED_EDGE ( 'NONE', *, *, #23285, .T. ) ;
#19408 = CARTESIAN_POINT ( 'NONE',  ( -39.56997771603464997, -5.935920012143626856, 77.89936816942207543 ) ) ;
#19409 = DIRECTION ( 'NONE',  ( -1.000000000000000000, 0.000000000000000000, 0.000000000000000000 ) ) ;
#19410 = CARTESIAN_POINT ( 'NONE',  ( -41.47915246182644466, 10.76506190587095801, 57.22447320499356493 ) ) ;
#19411 = VERTEX_POINT ( 'NONE', #19890 ) ;
#19412 = ORIENTED_EDGE ( 'NONE', *, *, #4996, .F. ) ;
#19413 = CARTESIAN_POINT ( 'NONE',  ( -39.57405207560572791, -5.935454207752198563, 77.87546120947918382 ) ) ;
#19414 = CIRCLE ( 'NONE', #19932, 13.20000000000000995 ) ;
#19415 = DIRECTION ( 'NONE',  ( -0.000000000000000000, -0.000000000000000000, 1.000000000000000000 ) ) ;
#19416 = DIRECTION ( 'NONE',  ( 0.000000000000000000, 0.000000000000000000, -1.000000000000000000 ) ) ;
#19417 = ORIENTED_EDGE ( 'NONE', *, *, #21063, .T. ) ;
#19418 = DIRECTION ( 'NONE',  ( 1.000000000000000000, 0.000000000000000000, 0.000000000000000000 ) ) ;
#19419 = VERTEX_POINT ( 'NONE', #27456 ) ;
#19420 = ADVANCED_FACE ( 'NONE', ( #4970 ), #15305, .F. ) ;
#19421 = AXIS2_PLACEMENT_3D ( 'NONE', #30972, #14049, #24046 ) ;
#19422 = ORIENTED_EDGE ( 'NONE', *, *, #19814, .T. ) ;
#19423 = CIRCLE ( 'NONE', #22017, 0.2000000000000012601 ) ;
#19424 = TOROIDAL_SURFACE ( 'NONE', #2665, 12.40141737965285529, 0.1250000000000000555 ) ;
#19425 = DIRECTION ( 'NONE',  ( -2.779292025043186357E-18, 1.288349127009862057E-17, -1.000000000000000000 ) ) ;
#19426 = VECTOR ( 'NONE', #28621, 1000.000000000000000 ) ;
#19427 = ORIENTED_EDGE ( 'NONE', *, *, #19375, .T. ) ;
#19428 = ADVANCED_FACE ( 'NONE', ( #20060 ), #15142, .T. ) ;
#19429 = CARTESIAN_POINT ( 'NONE',  ( -42.26253548098706858, 13.64258395852576911, 59.54930799450052348 ) ) ;
#19430 = CARTESIAN_POINT ( 'NONE',  ( -31.71490984672070823, 0.2276820184178854067, 80.17571310813880814 ) ) ;
#19431 = DIRECTION ( 'NONE',  ( -1.101824276508909887E-16, 1.000000000000000000, -0.000000000000000000 ) ) ;
#19432 = TOROIDAL_SURFACE ( 'NONE', #11573, 12.40141737965283042, 0.1249999999999995420 ) ;
#19433 = EDGE_CURVE ( 'NONE', #22755, #7305, #12697, .T. ) ;
#19434 = ORIENTED_EDGE ( 'NONE', *, *, #11394, .T. ) ;
#19435 = DIRECTION ( 'NONE',  ( 1.000000000000000000, 0.000000000000000000, 0.000000000000000000 ) ) ;
#19436 = ORIENTED_EDGE ( 'NONE', *, *, #17029, .T. ) ;
#19437 = CYLINDRICAL_SURFACE ( 'NONE', #19338, 12.36707279061065279 ) ;
#19438 = DIRECTION ( 'NONE',  ( -1.101824276508909887E-16, 1.000000000000000000, -0.000000000000000000 ) ) ;
#19439 = FACE_OUTER_BOUND ( 'NONE', #27211, .T. ) ;
#19440 = ORIENTED_EDGE ( 'NONE', *, *, #8220, .F. ) ;
#19441 = EDGE_CURVE ( 'NONE', #27386, #21015, #28738, .T. ) ;
#19442 = PLANE ( 'NONE',  #1303 ) ;
#19443 = DIRECTION ( 'NONE',  ( 0.8746197071393840838, -0.4848096202463581528, 0.000000000000000000 ) ) ;
#19444 = CARTESIAN_POINT ( 'NONE',  ( 21.09785597605719332, -8.535454207752287914, 47.04930799450051637 ) ) ;
#19445 = ADVANCED_FACE ( 'NONE', ( #31050 ), #25947, .T. ) ;
#19446 = DIRECTION ( 'NONE',  ( -0.000000000000000000, -1.000000000000000000, 0.000000000000000000 ) ) ;
#19447 = FACE_OUTER_BOUND ( 'NONE', #12627, .T. ) ;
#19448 = ADVANCED_FACE ( 'NONE', ( #23492 ), #23003, .T. ) ;
#19449 =( NAMED_UNIT ( * ) SI_UNIT ( $, .STERADIAN. ) SOLID_ANGLE_UNIT ( ) );
#19450 = VERTEX_POINT ( 'NONE', #688 ) ;
#19451 = CIRCLE ( 'NONE', #23107, 12.27641737965287128 ) ;
#19452 = CARTESIAN_POINT ( 'NONE',  ( -40.12089184044746304, 6.795442064577187580, 34.64508164218045039 ) ) ;
#19453 = DIRECTION ( 'NONE',  ( -1.224646799147353207E-16, -1.349345573449484691E-32, 1.000000000000000000 ) ) ;
#19454 = VERTEX_POINT ( 'NONE', #3464 ) ;
#19455 = CIRCLE ( 'NONE', #30483, 1.000000000000000888 ) ;
#19456 = CARTESIAN_POINT ( 'NONE',  ( 8.732853799281738105, 24.71183152705960140, 47.04930799450051637 ) ) ;
#19457 = CIRCLE ( 'NONE', #25695, 55.00000000000000000 ) ;
#19458 = DIRECTION ( 'NONE',  ( -1.000000000000000000, 0.000000000000000000, 0.000000000000000000 ) ) ;
#19459 = ORIENTED_EDGE ( 'NONE', *, *, #28235, .T. ) ;
#19460 = ORIENTED_EDGE ( 'NONE', *, *, #9426, .T. ) ;
#19461 = EDGE_CURVE ( 'NONE', #23152, #229, #20764, .T. ) ;
#19462 = VERTEX_POINT ( 'NONE', #16095 ) ;
#19463 = CIRCLE ( 'NONE', #24181, 2.500000000000002220 ) ;
#19464 = CIRCLE ( 'NONE', #31019, 1.500000000000001332 ) ;
#19465 = EDGE_CURVE ( 'NONE', #20784, #2889, #25474, .T. ) ;
#19466 = VECTOR ( 'NONE', #18738, 1000.000000000000114 ) ;
#19467 = DIRECTION ( 'NONE',  ( 2.779292025043186357E-18, -1.288349127009862211E-17, 1.000000000000000000 ) ) ;
#19468 = EDGE_CURVE ( 'NONE', #16672, #25906, #25475, .T. ) ;
#19469 = VERTEX_POINT ( 'NONE', #3306 ) ;
#19470 = ORIENTED_EDGE ( 'NONE', *, *, #29732, .T. ) ;
#19471 = CARTESIAN_POINT ( 'NONE',  ( -9.902144023942794249, 13.86454579224779948, 47.04930799450052348 ) ) ;
#19472 = DIRECTION ( 'NONE',  ( 0.9986540920324801229, 1.233316085972235327E-16, 0.05186525298099630560 ) ) ;
#19473 = DIRECTION ( 'NONE',  ( -1.101824276508909887E-16, 1.000000000000000000, -0.000000000000000000 ) ) ;
#19474 = DIRECTION ( 'NONE',  ( -0.8746197071393926326, 0.4848096202463430537, 8.676864087101709653E-18 ) ) ;
#19475 = CARTESIAN_POINT ( 'NONE',  ( 46.02876340639226527, 28.31119643316631240, 44.95353858666495483 ) ) ;
#19476 = EDGE_LOOP ( 'NONE', ( #24839, #28260, #28644, #23689 ) ) ;
#19477 = DIRECTION ( 'NONE',  ( -1.101824276508909887E-16, 1.000000000000000000, -0.000000000000000000 ) ) ;
#19478 = ORIENTED_EDGE ( 'NONE', *, *, #18551, .F. ) ;
#19479 = CARTESIAN_POINT ( 'NONE',  ( -9.248156207842958665, 5.417291301124353531, -4.090610767477680376 ) ) ;
#19480 = VECTOR ( 'NONE', #14215, 1000.000000000000000 ) ;
#19481 = EDGE_CURVE ( 'NONE', #4922, #155, #2976, .T. ) ;
#19482 = VERTEX_POINT ( 'NONE', #20544 ) ;
#19483 = CARTESIAN_POINT ( 'NONE',  ( -42.50976151518962354, 14.59907569580870224, 36.00717268343339583 ) ) ;
#19484 = CYLINDRICAL_SURFACE ( 'NONE', #29938, 0.1000000000000006301 ) ;
#19485 = CARTESIAN_POINT ( 'NONE',  ( 52.07598125554712709, -5.935454207752203004, 107.6091390186649761 ) ) ;
#19486 = DIRECTION ( 'NONE',  ( 0.5442436726714897643, 6.721291001053910056E-17, -0.8389271868029121171 ) ) ;
#19487 = LINE ( 'NONE', #26233, #12760 ) ;
#19488 = EDGE_CURVE ( 'NONE', #17225, #2185, #31265, .T. ) ;
#19489 = CARTESIAN_POINT ( 'NONE',  ( 48.46535932150934656, 26.88954579807171186, 49.73005965046827015 ) ) ;
#19490 = CARTESIAN_POINT ( 'NONE',  ( 46.31454563678332903, 22.93807716476589675, 48.55381333958629142 ) ) ;
#19491 = DIRECTION ( 'NONE',  ( -0.09590798424311161585, 0.9774730502038649904, -0.1880108898004995421 ) ) ;
#19492 = ORIENTED_EDGE ( 'NONE', *, *, #12588, .F. ) ;
#19493 = DIRECTION ( 'NONE',  ( 0.4848096202463424431, 0.8746197071393928546, -2.220446049250313081E-16 ) ) ;
#19494 = DIRECTION ( 'NONE',  ( -1.000000000000000000, -1.101824276508909764E-16, 0.000000000000000000 ) ) ;
#19495 = DIRECTION ( 'NONE',  ( -0.2756373558169932236, 0.9612616959383205595, 1.994417650674054674E-31 ) ) ;
#19496 = DIRECTION ( 'NONE',  ( -0.9612616959383194493, -0.2756373558169972759, -8.795445018804907668E-19 ) ) ;
#19497 = FACE_OUTER_BOUND ( 'NONE', #2767, .T. ) ;
#19498 = ORIENTED_EDGE ( 'NONE', *, *, #22968, .F. ) ;
#19499 = TOROIDAL_SURFACE ( 'NONE', #22640, 1.100000000000000089, 0.1000000000000000056 ) ;
#19500 = ORIENTED_EDGE ( 'NONE', *, *, #8413, .F. ) ;
#19501 = DIRECTION ( 'NONE',  ( -1.000000000000000000, 0.000000000000000000, 0.000000000000000000 ) ) ;
#19502 = ORIENTED_EDGE ( 'NONE', *, *, #18829, .T. ) ;
#19503 = AXIS2_PLACEMENT_3D ( 'NONE', #29217, #9361, #7060 ) ;
#19504 = B_SPLINE_SURFACE_WITH_KNOTS ( 'NONE', 3, 1, ( 
 ( #2873, #14265 ),
 ( #5352, #15350 ),
 ( #4563, #24756 ),
 ( #408, #27830 ),
 ( #17189, #2273 ),
 ( #22895, #14585 ),
 ( #26890, #1938 ),
 ( #27210, #16702 ),
 ( #9660, #24423 ),
 ( #24262, #19656 ),
 ( #11956, #6875 ),
 ( #29687, #2104 ) ),
 .UNSPECIFIED., .F., .F., .F.,
 ( 4, 1, 1, 1, 1, 1, 1, 1, 1, 4 ),
 ( 2, 2 ),
 ( 0.000000000000000000, 0.06961316558564611956, 0.1171086334586786126, 0.1635501317099198326, 0.2110163436193570607, 0.3800399093095634395, 0.5436454160257098156, 0.6849566023255588831, 0.8083832489416957756, 1.000000000000000000 ),
 ( 0.000000000000000000, 1.000000000000000000 ),
 .UNSPECIFIED. ) ;
#19505 = ORIENTED_EDGE ( 'NONE', *, *, #25528, .T. ) ;
#19506 = DIRECTION ( 'NONE',  ( 0.000000000000000000, -0.000000000000000000, -1.000000000000000000 ) ) ;
#19507 = CARTESIAN_POINT ( 'NONE',  ( 51.67049335409638644, 5.388785998227653806, -3.337848843846767721 ) ) ;
#19508 = FACE_OUTER_BOUND ( 'NONE', #13282, .T. ) ;
#19509 = AXIS2_PLACEMENT_3D ( 'NONE', #20324, #24944, #15255 ) ;
#19510 = ORIENTED_EDGE ( 'NONE', *, *, #4755, .F. ) ;
#19511 = CARTESIAN_POINT ( 'NONE',  ( 58.59785597605721108, 13.86454579224779948, 47.04930799450051637 ) ) ;
#19512 = TOROIDAL_SURFACE ( 'NONE', #6945, 1.299999999999999822, 0.1000000000000000056 ) ;
#19513 = DIRECTION ( 'NONE',  ( 0.000000000000000000, 0.000000000000000000, -1.000000000000000000 ) ) ;
#19514 = CARTESIAN_POINT ( 'NONE',  ( -10.01358250815963125, -5.935454354499447582, -13.39048028849681771 ) ) ;
#19515 = EDGE_LOOP ( 'NONE', ( #30730, #7150, #6655, #19286 ) ) ;
#19516 = EDGE_LOOP ( 'NONE', ( #4728, #2048, #31292, #19470 ) ) ;
#19517 = CARTESIAN_POINT ( 'NONE',  ( -39.51359738027355206, -5.935454207752198563, 77.87546120947918382 ) ) ;
#19518 = ADVANCED_FACE ( 'NONE', ( #15787 ), #30889, .T. ) ;
#19519 = ORIENTED_EDGE ( 'NONE', *, *, #21032, .F. ) ;
#19520 = CARTESIAN_POINT ( 'NONE',  ( -38.36853489569023168, 7.065850718397948427, 62.04930799450052348 ) ) ;
#19521 = CARTESIAN_POINT ( 'NONE',  ( 21.09992658989239089, 26.34164230456639899, 47.04930799450051637 ) ) ;
#19522 = DIRECTION ( 'NONE',  ( 0.000000000000000000, -0.000000000000000000, -1.000000000000000000 ) ) ;
#19523 = EDGE_CURVE ( 'NONE', #5852, #5096, #13176, .T. ) ;
#19524 = CARTESIAN_POINT ( 'NONE',  ( -45.22803192368630931, -5.771461585458397714, 40.85022782416209708 ) ) ;
#19525 = CARTESIAN_POINT ( 'NONE',  ( 0.000000000000000000, 0.000000000000000000, 0.000000000000000000 ) ) ;
#19526 = ORIENTED_EDGE ( 'NONE', *, *, #1320, .T. ) ;
#19527 = ORIENTED_EDGE ( 'NONE', *, *, #21962, .F. ) ;
#19528 = CARTESIAN_POINT ( 'NONE',  ( 21.09785597605719332, 42.30003263981368633, 77.04930799450052348 ) ) ;
#19529 = DIRECTION ( 'NONE',  ( 0.8746197071393858602, -0.4848096202463547666, 0.000000000000000000 ) ) ;
#19530 = LINE ( 'NONE', #30051, #30899 ) ;
#19531 = AXIS2_PLACEMENT_3D ( 'NONE', #16862, #31969, #16372 ) ;
#19532 = ORIENTED_EDGE ( 'NONE', *, *, #10805, .F. ) ;
#19533 = CARTESIAN_POINT ( 'NONE',  ( -9.732626758893591301, 4.638969541771042593, -5.235519273104768168 ) ) ;
#19534 = DIRECTION ( 'NONE',  ( -1.000000000000000000, 0.000000000000000000, 0.000000000000000000 ) ) ;
#19535 = CIRCLE ( 'NONE', #5399, 19.99999999999999645 ) ;
#19536 = ORIENTED_EDGE ( 'NONE', *, *, #27906, .F. ) ;
#19537 = CARTESIAN_POINT ( 'NONE',  ( -40.65487266620045403, 9.475231293617262907, 34.66144002885648945 ) ) ;
#19538 = CARTESIAN_POINT ( 'NONE',  ( 8.732853799281734553, 38.56284415653841791, 47.04930799450051637 ) ) ;
#19539 = CARTESIAN_POINT ( 'NONE',  ( 21.09992658989238734, 31.09184655352422411, 47.04930799450051637 ) ) ;
#19540 = VECTOR ( 'NONE', #31144, 1000.000000000000000 ) ;
#19541 = ORIENTED_EDGE ( 'NONE', *, *, #4705, .T. ) ;
#19542 = DIRECTION ( 'NONE',  ( -1.000000000000000000, 0.000000000000000000, 0.000000000000000000 ) ) ;
#19543 = DIRECTION ( 'NONE',  ( -0.000000000000000000, -1.000000000000000000, -0.000000000000000000 ) ) ;
#19544 = CARTESIAN_POINT ( 'NONE',  ( 47.79865503179234310, 9.702389020015065313, -3.412202488244239884 ) ) ;
#19545 = CARTESIAN_POINT ( 'NONE',  ( 45.79384627280941089, 27.16618040159427139, 49.05938063676249072 ) ) ;
#19546 = ORIENTED_EDGE ( 'NONE', *, *, #12628, .F. ) ;
#19547 = VECTOR ( 'NONE', #10637, 1000.000000000000000 ) ;
#19548 = DIRECTION ( 'NONE',  ( -1.000000000000000000, 0.000000000000000000, 0.000000000000000000 ) ) ;
#19550 = CARTESIAN_POINT ( 'NONE',  ( 21.09992658989239089, 26.71183152705960495, 47.04930799450051637 ) ) ;
#19549 = TOROIDAL_SURFACE ( 'NONE', #30569, 58.88977237527051756, 0.9999999999999997780 ) ;
#19551 = DIRECTION ( 'NONE',  ( -0.8746197071393810862, 0.4848096202463637039, 8.676864087101942305E-18 ) ) ;
#19552 = EDGE_CURVE ( 'NONE', #12341, #19026, #22867, .T. ) ;
#19553 = CARTESIAN_POINT ( 'NONE',  ( 33.50134396954521776, 29.59164230456639899, 47.04930799450051637 ) ) ;
#19554 = DIRECTION ( 'NONE',  ( 1.234978253042719660E-16, -1.000000000000000000, -1.109335647967047851E-31 ) ) ;
#19555 = DIRECTION ( 'NONE',  ( -1.000000000000000000, 0.000000000000000000, 0.000000000000000000 ) ) ;
#19556 = EDGE_CURVE ( 'NONE', #15217, #9970, #330, .T. ) ;
#19557 = CARTESIAN_POINT ( 'NONE',  ( 2.337203576606295297, -13.74047052604243646, -8.200871005066998620 ) ) ;
#19558 = DIRECTION ( 'NONE',  ( -0.9612616959383204485, -0.2756373558169933347, 1.660411357259282692E-16 ) ) ;
#19559 = EDGE_CURVE ( 'NONE', #7408, #6923, #3408, .T. ) ;
#19560 = TOROIDAL_SURFACE ( 'NONE', #28483, 12.40141737965283930, 0.1250000000000007216 ) ;
#19561 = AXIS2_PLACEMENT_3D ( 'NONE', #4558, #14416, #11628 ) ;
#19562 = ADVANCED_FACE ( 'NONE', ( #24455 ), #23387, .T. ) ;
#19563 = FACE_BOUND ( 'NONE', #25085, .T. ) ;
#19564 = CARTESIAN_POINT ( 'NONE',  ( -40.46271621608484281, 3.081581074246048768, 35.54930799450051637 ) ) ;
#19565 = EDGE_CURVE ( 'NONE', #18541, #9695, #7674, .T. ) ;
#19566 = DIRECTION ( 'NONE',  ( 1.000000000000000000, 0.000000000000000000, 0.000000000000000000 ) ) ;
#19567 = ORIENTED_EDGE ( 'NONE', *, *, #1968, .F. ) ;
#19568 = DIRECTION ( 'NONE',  ( -0.9612616959383206705, -0.2756373558169931681, 1.660411357259282445E-16 ) ) ;
#19569 = FACE_OUTER_BOUND ( 'NONE', #26876, .T. ) ;
#19570 = LINE ( 'NONE', #12201, #7740 ) ;
#19571 = DIRECTION ( 'NONE',  ( -0.4848096202463432203, -0.8746197071393924105, -9.920727850371698576E-18 ) ) ;
#19572 = VERTEX_POINT ( 'NONE', #16729 ) ;
#19573 = DIRECTION ( 'NONE',  ( 0.2756373558169956106, -0.9612616959383200044, -1.546443900056102631E-15 ) ) ;
#19574 = DIRECTION ( 'NONE',  ( -0.000000000000000000, -1.000000000000000000, 0.000000000000000000 ) ) ;
#19575 = DIRECTION ( 'NONE',  ( -0.000000000000000000, -1.000000000000000000, -0.000000000000000000 ) ) ;
#19576 = EDGE_LOOP ( 'NONE', ( #6995, #9454, #27384, #24053 ) ) ;
#19577 = ORIENTED_EDGE ( 'NONE', *, *, #25650, .T. ) ;
#19578 = CARTESIAN_POINT ( 'NONE',  ( -40.15611298324447631, 6.923081382651431248, 39.54802830809165215 ) ) ;
#19579 = DIRECTION ( 'NONE',  ( -0.5442436726714893203, -1.289618226626749726E-16, 0.8389271868029124501 ) ) ;
#19580 = CARTESIAN_POINT ( 'NONE',  ( -7.324817582041172948, 8.310461108307681144, -3.351769630585352377 ) ) ;
#19581 = DIRECTION ( 'NONE',  ( -0.000000000000000000, 1.000000000000000000, -0.000000000000000000 ) ) ;
#19582 = CIRCLE ( 'NONE', #30612, 0.1250000000000001110 ) ;
#19583 = DIRECTION ( 'NONE',  ( 0.4848096202463673676, 0.8746197071393789768, 0.000000000000000000 ) ) ;
#19584 = ORIENTED_EDGE ( 'NONE', *, *, #30868, .T. ) ;
#19585 = EDGE_CURVE ( 'NONE', #7034, #28434, #18134, .T. ) ;
#19586 = ORIENTED_EDGE ( 'NONE', *, *, #12465, .F. ) ;
#19587 = AXIS2_PLACEMENT_3D ( 'NONE', #10601, #8605, #15509 ) ;
#19588 = AXIS2_PLACEMENT_3D ( 'NONE', #27749, #4781, #29897 ) ;
#19589 = DIRECTION ( 'NONE',  ( -1.101824276508909887E-16, 1.000000000000000000, -0.000000000000000000 ) ) ;
#19590 = ADVANCED_FACE ( 'NONE', ( #9533 ), #1650, .T. ) ;
#19591 = ORIENTED_EDGE ( 'NONE', *, *, #12952, .F. ) ;
#19592 = CARTESIAN_POINT ( 'NONE',  ( -40.14060284811700541, 7.788019651925920606, 39.54930799450052348 ) ) ;
#19593 = CARTESIAN_POINT ( 'NONE',  ( -30.88361636257000598, 11.92558985988973141, 67.49515520264003499 ) ) ;
#19594 = EDGE_LOOP ( 'NONE', ( #1410, #21906, #11513, #22460 ) ) ;
#19595 = DIRECTION ( 'NONE',  ( -1.224646799147353207E-16, -1.349345573449484691E-32, 1.000000000000000000 ) ) ;
#19596 = VERTEX_POINT ( 'NONE', #13810 ) ;
#19597 = AXIS2_PLACEMENT_3D ( 'NONE', #19387, #14319, #11854 ) ;
#19598 = DIRECTION ( 'NONE',  ( 0.000000000000000000, 0.000000000000000000, 1.000000000000000000 ) ) ;
#19599 = EDGE_CURVE ( 'NONE', #16423, #27923, #4525, .T. ) ;
#19600 = CARTESIAN_POINT ( 'NONE',  ( -37.21204910874187988, -5.721341737285086992, 15.20211895544695757 ) ) ;
#19601 = ORIENTED_EDGE ( 'NONE', *, *, #25247, .T. ) ;
#19602 = CARTESIAN_POINT ( 'NONE',  ( 21.09785597605719332, 11.92558985988973497, 47.04930799450051637 ) ) ;
#19603 = DIRECTION ( 'NONE',  ( -0.2756373558169974980, 0.9612616959383193382, 1.315048337272770589E-17 ) ) ;
#19604 = DIRECTION ( 'NONE',  ( 0.9612616959383221138, 0.2756373558169876170, 0.000000000000000000 ) ) ;
#19605 = DIRECTION ( 'NONE',  ( -0.8746197071393895239, 0.4848096202463481053, 0.000000000000000000 ) ) ;
#19606 = CARTESIAN_POINT ( 'NONE',  ( 21.09785597605719332, -12.82881809906321458, 47.04930799450051637 ) ) ;
#19607 = ORIENTED_EDGE ( 'NONE', *, *, #17146, .F. ) ;
#19608 = DIRECTION ( 'NONE',  ( -1.101824276508909887E-16, 1.000000000000000000, -0.000000000000000000 ) ) ;
#19609 = DIRECTION ( 'NONE',  ( -1.000000000000000000, 0.000000000000000000, 0.000000000000000000 ) ) ;
#19610 = EDGE_LOOP ( 'NONE', ( #17892, #10134 ) ) ;
#19611 = CARTESIAN_POINT ( 'NONE',  ( 21.09992658989239089, 25.34143805560860940, 47.04930799450051637 ) ) ;
#19612 = CARTESIAN_POINT ( 'NONE',  ( 33.37634396954527460, 24.34164230456639544, 47.04930799450051637 ) ) ;
#19613 = EDGE_LOOP ( 'NONE', ( #6634, #12817, #4749, #27405 ) ) ;
#19614 = ADVANCED_FACE ( 'NONE', ( #19033 ), #21826, .T. ) ;
#19615 = EDGE_LOOP ( 'NONE', ( #10769, #22309, #28715, #21656 ) ) ;
#19616 = EDGE_CURVE ( 'NONE', #2499, #24828, #16044, .T. ) ;
#19617 = VERTEX_POINT ( 'NONE', #19528 ) ;
#19618 = AXIS2_PLACEMENT_3D ( 'NONE', #1997, #27761, #15130 ) ;
#19619 = CIRCLE ( 'NONE', #29603, 12.62506659569710443 ) ;
#19620 = EDGE_CURVE ( 'NONE', #19851, #26545, #26527, .T. ) ;
#19621 = CIRCLE ( 'NONE', #30667, 12.36707279061065101 ) ;
#19622 = EDGE_CURVE ( 'NONE', #2789, #20229, #16255, .T. ) ;
#19623 = AXIS2_PLACEMENT_3D ( 'NONE', #20516, #3105, #20345 ) ;
#19624 = AXIS2_PLACEMENT_3D ( 'NONE', #12989, #17903, #25454 ) ;
#19625 = CARTESIAN_POINT ( 'NONE',  ( -40.65487266620045403, 9.475231293617264683, 39.54930799450052348 ) ) ;
#19626 = EDGE_LOOP ( 'NONE', ( #10966, #15286, #13079, #24381 ) ) ;
#19627 = ORIENTED_EDGE ( 'NONE', *, *, #10287, .F. ) ;
#19628 = CARTESIAN_POINT ( 'NONE',  ( -40.73091736380679606, 9.483895492497156354, 39.44930799450052916 ) ) ;
#19629 = CARTESIAN_POINT ( 'NONE',  ( 21.09992658989239089, 26.46664230456639899, 47.04930799450051637 ) ) ;
#19630 = DIRECTION ( 'NONE',  ( 0.000000000000000000, -1.000000000000000000, 0.000000000000000000 ) ) ;
#19631 = DIRECTION ( 'NONE',  ( 0.2756373558169942228, -0.9612616959383203374, 0.000000000000000000 ) ) ;
#19632 = EDGE_CURVE ( 'NONE', #19261, #4546, #9289, .T. ) ;
#19633 = EDGE_LOOP ( 'NONE', ( #11578, #16703, #32092, #28417 ) ) ;
#19634 = DIRECTION ( 'NONE',  ( -1.000000000000000000, 0.000000000000000000, 0.000000000000000000 ) ) ;
#19635 = VERTEX_POINT ( 'NONE', #23805 ) ;
#19636 = CARTESIAN_POINT ( 'NONE',  ( -30.67295000222299706, 6.587260180950779365, 17.48485802005428624 ) ) ;
#19637 = DIRECTION ( 'NONE',  ( 0.9612616959383205595, 0.2756373558169931681, -1.660411357259282445E-16 ) ) ;
#19638 = EDGE_LOOP ( 'NONE', ( #31462, #15507, #11599, #13256 ) ) ;
#19639 = CARTESIAN_POINT ( 'NONE',  ( 8.732853799281729223, 27.72145308207318237, 47.04930799450051637 ) ) ;
#19640 = DIRECTION ( 'NONE',  ( 0.000000000000000000, -0.000000000000000000, -1.000000000000000000 ) ) ;
#19641 = CARTESIAN_POINT ( 'NONE',  ( 47.09785597605719687, 25.56454579224779167, 44.54930799450078638 ) ) ;
#19642 = CARTESIAN_POINT ( 'NONE',  ( 21.09992658989239089, 25.72145308207319303, 47.04930799450051637 ) ) ;
#19643 = DIRECTION ( 'NONE',  ( -0.000000000000000000, -1.000000000000000000, 0.000000000000000000 ) ) ;
#19644 = CARTESIAN_POINT ( 'NONE',  ( 48.83862994770794330, 26.55457786121582231, 48.17861352429476796 ) ) ;
#19645 = AXIS2_PLACEMENT_3D ( 'NONE', #190, #5113, #10208 ) ;
#19646 = CYLINDRICAL_SURFACE ( 'NONE', #6882, 2.500000000000002220 ) ;
#19647 = CARTESIAN_POINT ( 'NONE',  ( -42.30426555199245797, 13.25214768565125034, 59.74914412770269934 ) ) ;
#19648 = CIRCLE ( 'NONE', #18584, 39.69941114636694124 ) ;
#19649 = ORIENTED_EDGE ( 'NONE', *, *, #25255, .F. ) ;
#19650 = FACE_OUTER_BOUND ( 'NONE', #23786, .T. ) ;
#19651 = CARTESIAN_POINT ( 'NONE',  ( 2.097855976057206639, -5.098646251524523443, 47.04930799450052348 ) ) ;
#19652 = AXIS2_PLACEMENT_3D ( 'NONE', #22882, #14860, #27819 ) ;
#19653 = CYLINDRICAL_SURFACE ( 'NONE', #32393, 12.36707279061065101 ) ;
#19654 = AXIS2_PLACEMENT_3D ( 'NONE', #1554, #24824, #8951 ) ;
#19655 = AXIS2_PLACEMENT_3D ( 'NONE', #2284, #22297, #22130 ) ;
#19656 = CARTESIAN_POINT ( 'NONE',  ( -29.27337757263006424, 11.23353061944650655, 22.24400271019782593 ) ) ;
#19657 = ORIENTED_EDGE ( 'NONE', *, *, #25392, .T. ) ;
#19658 = EDGE_CURVE ( 'NONE', #18133, #3119, #11856, .T. ) ;
#19659 = EDGE_LOOP ( 'NONE', ( #29400, #15257, #11935, #30348 ) ) ;
#19660 = DIRECTION ( 'NONE',  ( -1.000000000000000000, 0.000000000000000000, 0.000000000000000000 ) ) ;
#19661 = EDGE_CURVE ( 'NONE', #10922, #15685, #11322, .T. ) ;
#19662 = ORIENTED_EDGE ( 'NONE', *, *, #16843, .F. ) ;
#19663 = EDGE_CURVE ( 'NONE', #30888, #28530, #22320, .T. ) ;
#19664 = EDGE_CURVE ( 'NONE', #14591, #32254, #15518, .T. ) ;
#19665 = ORIENTED_EDGE ( 'NONE', *, *, #14802, .F. ) ;
#19666 = AXIS2_PLACEMENT_3D ( 'NONE', #19683, #14613, #32007 ) ;
#19667 = CARTESIAN_POINT ( 'NONE',  ( 46.76015065834239692, 23.11533908250407165, 47.22157799611917994 ) ) ;
#19668 = CARTESIAN_POINT ( 'NONE',  ( 8.732853799281731000, 27.22145308207318237, 47.04930799450051637 ) ) ;
#19669 = AXIS2_PLACEMENT_3D ( 'NONE', #29254, #11374, #8910 ) ;
#19670 =( GEOMETRIC_REPRESENTATION_CONTEXT ( 3 ) GLOBAL_UNCERTAINTY_ASSIGNED_CONTEXT ( ( #25891 ) ) GLOBAL_UNIT_ASSIGNED_CONTEXT ( ( #18266, #3340, #23367 ) ) REPRESENTATION_CONTEXT ( 'NONE', 'WORKASPACE' ) );
#19671 = AXIS2_PLACEMENT_3D ( 'NONE', #9923, #7630, #17467 ) ;
#19672 = VERTEX_POINT ( 'NONE', #27577 ) ;
#19673 = DIRECTION ( 'NONE',  ( -1.101824276508909887E-16, 1.000000000000000000, -0.000000000000000000 ) ) ;
#19674 = CARTESIAN_POINT ( 'NONE',  ( 21.09992658989239089, 26.71664230456639899, 47.04930799450051637 ) ) ;
#19675 = PLANE ( 'NONE',  #11679 ) ;
#19676 = CARTESIAN_POINT ( 'NONE',  ( 45.35708200440645044, 25.50457786121582515, 45.92000246470679770 ) ) ;
#19677 = ORIENTED_EDGE ( 'NONE', *, *, #17038, .F. ) ;
#19678 = VERTEX_POINT ( 'NONE', #17066 ) ;
#19679 = CARTESIAN_POINT ( 'NONE',  ( 52.59785597605720397, 13.86454579224779948, 47.04930799450051637 ) ) ;
#19680 = ORIENTED_EDGE ( 'NONE', *, *, #22751, .F. ) ;
#19681 = AXIS2_PLACEMENT_3D ( 'NONE', #21313, #9020, #1461 ) ;
#19682 = CARTESIAN_POINT ( 'NONE',  ( 21.09785597605719332, 12.11061942510878886, 47.04930799450051637 ) ) ;
#19683 = CARTESIAN_POINT ( 'NONE',  ( 21.09785597605719332, 38.31023907818019580, 47.04930799450051637 ) ) ;
#19684 = CARTESIAN_POINT ( 'NONE',  ( -40.68572042366847086, 6.804601513393308210, 34.76387516412972190 ) ) ;
#19685 = CARTESIAN_POINT ( 'NONE',  ( -45.06166779280744095, -5.721341737285086992, 40.94964444931001424 ) ) ;
#19686 = CARTESIAN_POINT ( 'NONE',  ( 48.94625023931840246, 27.37124452788248874, 46.10640627770149536 ) ) ;
#19687 =( LENGTH_UNIT ( ) NAMED_UNIT ( * ) SI_UNIT ( .MILLI., .METRE. ) );
#19688 = ORIENTED_EDGE ( 'NONE', *, *, #27391, .F. ) ;
#19689 = EDGE_LOOP ( 'NONE', ( #28299, #20612, #22908, #19607 ) ) ;
#19690 = DIRECTION ( 'NONE',  ( -1.101824276508909887E-16, 1.000000000000000000, -0.000000000000000000 ) ) ;
#19691 = DIRECTION ( 'NONE',  ( 0.000000000000000000, -1.000000000000000000, 0.000000000000000000 ) ) ;
#19692 = CARTESIAN_POINT ( 'NONE',  ( 21.09785597605720042, -8.535454207752287914, 115.0493079945004951 ) ) ;
#19693 = ORIENTED_EDGE ( 'NONE', *, *, #18457, .F. ) ;
#19694 = CARTESIAN_POINT ( 'NONE',  ( 52.10659382688164243, -5.936607700120022812, 107.4592332772410259 ) ) ;
#19695 = CARTESIAN_POINT ( 'NONE',  ( 33.50134396954523197, 28.09164230456639544, 47.04930799450051637 ) ) ;
#19696 = EDGE_CURVE ( 'NONE', #15433, #7860, #1348, .T. ) ;
#19697 = ORIENTED_EDGE ( 'NONE', *, *, #5166, .T. ) ;
#19698 = DIRECTION ( 'NONE',  ( 0.000000000000000000, -1.000000000000000000, 0.000000000000000000 ) ) ;
#19699 = CARTESIAN_POINT ( 'NONE',  ( 21.09785597605718266, -13.49020584019834601, 105.1414762132873193 ) ) ;
#19700 = AXIS2_PLACEMENT_3D ( 'NONE', #32013, #26436, #26924 ) ;
#19701 = PRESENTATION_LAYER_ASSIGNMENT (  '', '', ( #19174 ) ) ;
#19702 = EDGE_CURVE ( 'NONE', #19678, #20658, #23900, .T. ) ;
#19703 = LINE ( 'NONE', #10194, #7055 ) ;
#19704 = EDGE_CURVE ( 'NONE', #2267, #31427, #9756, .T. ) ;
#19705 = CIRCLE ( 'NONE', #5570, 0.8928932188134564019 ) ;
#19706 = EDGE_LOOP ( 'NONE', ( #13351, #4809, #11576, #12375 ) ) ;
#19707 =( BOUNDED_CURVE ( )  B_SPLINE_CURVE ( 2, ( #7743, #2654, #17741, #27763, #15293, #12841, #30389, #7912, #17911 ),
 .UNSPECIFIED., .F., .F. ) 
 B_SPLINE_CURVE_WITH_KNOTS ( ( 3, 2, 2, 2, 3 ),
 ( 0.6785714297327011257, 0.6904761904761904656, 0.7142857142857143016, 0.7380952380952381375, 0.7500000011612726336 ),
 .UNSPECIFIED. ) 
 CURVE ( )  GEOMETRIC_REPRESENTATION_ITEM ( )  RATIONAL_B_SPLINE_CURVE ( ( 0.9330127018922200755, 0.9330127084266224280, 1.000000000000000000, 0.8660254037844388186, 1.000000000000000000, 0.8660254037844388186, 1.000000000000000000, 0.9330126953578160576, 0.9330127018922200755 ) ) 
 REPRESENTATION_ITEM ( '' )  );
#19708 = ORIENTED_EDGE ( 'NONE', *, *, #25492, .T. ) ;
#19709 = DIRECTION ( 'NONE',  ( 0.2756373558169927240, -0.9612616959383207815, 2.391708153157048402E-17 ) ) ;
#19710 = DIRECTION ( 'NONE',  ( -1.101824276508909887E-16, 1.000000000000000000, -0.000000000000000000 ) ) ;
#19711 = FACE_OUTER_BOUND ( 'NONE', #12221, .T. ) ;
#19712 = ORIENTED_EDGE ( 'NONE', *, *, #13494, .T. ) ;
#19713 = CARTESIAN_POINT ( 'NONE',  ( 21.09785597605719332, -16.43545420775217281, 132.0493079945005377 ) ) ;
#19714 = DIRECTION ( 'NONE',  ( -1.000000000000000000, 0.000000000000000000, 0.000000000000000000 ) ) ;
#19715 = AXIS2_PLACEMENT_3D ( 'NONE', #4067, #14097, #6698 ) ;
#19716 = CARTESIAN_POINT ( 'NONE',  ( 52.36305255737380548, 3.903925281081623844, -4.517372811625020468 ) ) ;
#19717 = FACE_OUTER_BOUND ( 'NONE', #3882, .T. ) ;
#19718 = CARTESIAN_POINT ( 'NONE',  ( 33.46699938050304013, 23.97145308207319658, 47.04930799450050927 ) ) ;
#19719 = DIRECTION ( 'NONE',  ( 0.000000000000000000, 0.000000000000000000, -1.000000000000000000 ) ) ;
#19720 = CARTESIAN_POINT ( 'NONE',  ( -17.37805493069433282, -13.74047052604243646, 3.184189302845381153 ) ) ;
#19721 = CYLINDRICAL_SURFACE ( 'NONE', #12626, 12.36707279061065101 ) ;
#19722 = DIRECTION ( 'NONE',  ( 0.000000000000000000, -1.000000000000000000, 0.000000000000000000 ) ) ;
#19723 = CARTESIAN_POINT ( 'NONE',  ( -0.4021440239427923058, 14.86454579224779948, 47.04930799450052348 ) ) ;
#19724 = ORIENTED_EDGE ( 'NONE', *, *, #8807, .F. ) ;
#19725 = EDGE_LOOP ( 'NONE', ( #10789, #4016, #18423, #26781, #28196, #27432, #8332, #15446, #18914, #29706, #18644, #16460, #11996, #4785, #5067 ) ) ;
#19726 = DIRECTION ( 'NONE',  ( 0.000000000000000000, 1.000000000000000000, 0.000000000000000000 ) ) ;
#19727 = CARTESIAN_POINT ( 'NONE',  ( 48.34748475735720774, 24.70653309617948423, 49.49898713858203791 ) ) ;
#19728 = DIRECTION ( 'NONE',  ( 0.9612616959383191162, 0.2756373558169986082, 8.795445018805098335E-19 ) ) ;
#19729 = AXIS2_PLACEMENT_3D ( 'NONE', #17247, #22336, #27263 ) ;
#19730 = CARTESIAN_POINT ( 'NONE',  ( 80.85108986838919520, 8.310461108307681144, 75.47198155259910379 ) ) ;
#19731 = ORIENTED_EDGE ( 'NONE', *, *, #2310, .F. ) ;
#19732 = DIRECTION ( 'NONE',  ( -0.5319835227803602073, 0.2110602665713099124, 0.8200287161831869565 ) ) ;
#19733 = CARTESIAN_POINT ( 'NONE',  ( 21.09785597605720753, -5.098646251524523443, 47.04930799450052348 ) ) ;
#19734 = CARTESIAN_POINT ( 'NONE',  ( 43.69445516536492846, 11.70027025134008625, -4.173706942055579461 ) ) ;
#19735 = EDGE_LOOP ( 'NONE', ( #2328, #7253, #20801, #26525 ) ) ;
#19736 = ORIENTED_EDGE ( 'NONE', *, *, #10945, .F. ) ;
#19737 = DIRECTION ( 'NONE',  ( -0.000000000000000000, -1.000000000000000000, 0.000000000000000000 ) ) ;
#19738 = CARTESIAN_POINT ( 'NONE',  ( -21.90214402394278892, -5.098646251524523443, 47.04930799450052348 ) ) ;
#19739 = DIRECTION ( 'NONE',  ( -1.000000000000000000, 0.000000000000000000, 0.000000000000000000 ) ) ;
#19740 = CARTESIAN_POINT ( 'NONE',  ( -41.73034863705382946, 11.48775164340967336, 58.05249952744806308 ) ) ;
#19741 = ORIENTED_EDGE ( 'NONE', *, *, #28235, .F. ) ;
#19742 = AXIS2_PLACEMENT_3D ( 'NONE', #8752, #16136, #18750 ) ;
#19743 = EDGE_CURVE ( 'NONE', #29734, #6626, #18931, .T. ) ;
#19744 = VERTEX_POINT ( 'NONE', #12656 ) ;
#19745 = EDGE_CURVE ( 'NONE', #10438, #14591, #322, .T. ) ;
#19746 = ADVANCED_FACE ( 'NONE', ( #5092 ), #32296, .T. ) ;
#19747 = EDGE_CURVE ( 'NONE', #10620, #16477, #22329, .T. ) ;
#19748 = DIRECTION ( 'NONE',  ( -0.9612616959383207815, -0.2756373558169926685, -8.795445018804289444E-19 ) ) ;
#19749 = EDGE_CURVE ( 'NONE', #16051, #7822, #30733, .T. ) ;
#19750 = CIRCLE ( 'NONE', #11367, 0.09999999999999795164 ) ;
#19751 = ORIENTED_EDGE ( 'NONE', *, *, #24105, .T. ) ;
#19752 = FACE_OUTER_BOUND ( 'NONE', #19335, .T. ) ;
#19753 = CARTESIAN_POINT ( 'NONE',  ( -40.18454328187963398, 7.548069831825863218, 53.64930799450051779 ) ) ;
#19754 = B_SPLINE_CURVE_WITH_KNOTS ( 'NONE', 3,
 ( #22233, #9778, #12567, #19768, #22392, #22729, #7312, #27331, #9935, #19936, #7481, #22556, #20101, #17479, #30131, #27653, #5176, #245, #5981, #28467, #3016, #20903, #880, #25515, #11073, #10907, #13378, #28148, #25989, #21057 ),
 .UNSPECIFIED., .F., .F.,
 ( 4, 2, 2, 2, 2, 2, 2, 2, 2, 2, 2, 2, 2, 2, 4 ),
 ( 0.000000000000000000, 0.001249755272498811022, 0.002499510544997622045, 0.003749265817496432850, 0.004999021089995244090, 0.007498531634992865701, 0.009998042179990488179, 0.01249755272498811152, 0.01374730799748691452, 0.01499706326998571926, 0.01562194090623512423, 0.01624681854248452573, 0.01749657381498331485, 0.01874632908748210397, 0.01999608435998089309 ),
 .UNSPECIFIED. ) ;
#19755 = ORIENTED_EDGE ( 'NONE', *, *, #27022, .T. ) ;
#19756 = CARTESIAN_POINT ( 'NONE',  ( -40.86567715954772240, 8.502676639195792418, 34.64880948087299117 ) ) ;
#19757 = ORIENTED_EDGE ( 'NONE', *, *, #20678, .T. ) ;
#19758 = CARTESIAN_POINT ( 'NONE',  ( 21.09992658989239089, 28.09143805560861296, 47.04930799450051637 ) ) ;
#19759 = DIRECTION ( 'NONE',  ( 0.9612616959383205595, 0.2756373558169932236, -1.660411357259282445E-16 ) ) ;
#19760 = CARTESIAN_POINT ( 'NONE',  ( 21.09992658989239089, 24.34164230456639544, 47.04930799450051637 ) ) ;
#19761 = ORIENTED_EDGE ( 'NONE', *, *, #8134, .F. ) ;
#19762 = CARTESIAN_POINT ( 'NONE',  ( 71.97287007337540388, 6.453333540778382726, 76.71314589128250816 ) ) ;
#19763 = CARTESIAN_POINT ( 'NONE',  ( -41.52623485060432529, 12.58989991563029598, 57.04930799450051637 ) ) ;
#19765 = DIRECTION ( 'NONE',  ( -0.8746197071393805311, 0.4848096202463645921, 8.676864087101954631E-18 ) ) ;
#19764 = TOROIDAL_SURFACE ( 'NONE', #4044, 12.40141737965284641, 0.1249999999999995698 ) ;
#19766 = DIRECTION ( 'NONE',  ( 1.000000000000000000, 0.000000000000000000, 0.000000000000000000 ) ) ;
#19767 = DIRECTION ( 'NONE',  ( -0.000000000000000000, -1.000000000000000000, 0.000000000000000000 ) ) ;
#19768 = CARTESIAN_POINT ( 'NONE',  ( 72.50791967827838391, 8.582373042058220491, 74.98955504367758351 ) ) ;
#19769 = ORIENTED_EDGE ( 'NONE', *, *, #30948, .T. ) ;
#19770 = DIRECTION ( 'NONE',  ( -1.000000000000000000, -1.101824276508909887E-16, 0.000000000000000000 ) ) ;
#19771 = CARTESIAN_POINT ( 'NONE',  ( 21.09785597605719332, 7.881678200673685630, 47.04930799450051637 ) ) ;
#19772 = TOROIDAL_SURFACE ( 'NONE', #6677, 83.95481021798164534, 94.94530576803560962 ) ;
#19773 = ORIENTED_EDGE ( 'NONE', *, *, #29808, .F. ) ;
#19775 = ADVANCED_FACE ( 'NONE', ( #24956 ), #15266, .F. ) ;
#19774 = DIRECTION ( 'NONE',  ( 1.000000000000000000, 0.000000000000000000, 0.000000000000000000 ) ) ;
#19776 =( REPRESENTATION_RELATIONSHIP ('NONE','NONE', #20382, #28161 ) REPRESENTATION_RELATIONSHIP_WITH_TRANSFORMATION ( #3268 )SHAPE_REPRESENTATION_RELATIONSHIP( ) );
#19777 = PLANE ( 'NONE',  #6451 ) ;
#19778 = ORIENTED_EDGE ( 'NONE', *, *, #2846, .F. ) ;
#19779 = PRODUCT ( 'Coil Support', 'Coil Support', '', ( #22958 ) ) ;
#19780 = VERTEX_POINT ( 'NONE', #4932 ) ;
#19781 = VERTEX_POINT ( 'NONE', #29884 ) ;
#19782 = EDGE_CURVE ( 'NONE', #25934, #18639, #7401, .T. ) ;
#19783 = EDGE_CURVE ( 'NONE', #17931, #13599, #13440, .T. ) ;
#19784 = EDGE_CURVE ( 'NONE', #2312, #30851, #8214, .T. ) ;
#19785 = EDGE_CURVE ( 'NONE', #15685, #2384, #23911, .T. ) ;
#19786 = AXIS2_PLACEMENT_3D ( 'NONE', #18556, #25952, #28432 ) ;
#19787 = TOROIDAL_SURFACE ( 'NONE', #20376, 12.40141737965281266, 0.1249999999999994865 ) ;
#19788 = VECTOR ( 'NONE', #14749, 1000.000000000000000 ) ;
#19789 = ORIENTED_EDGE ( 'NONE', *, *, #14720, .T. ) ;
#19790 = TOROIDAL_SURFACE ( 'NONE', #5662, 12.40141737965287305, 0.1250000000000000833 ) ;
#19791 = ORIENTED_EDGE ( 'NONE', *, *, #21443, .F. ) ;
#19792 = CARTESIAN_POINT ( 'NONE',  ( 21.09992658989239089, 28.84164230456639544, 47.04930799450051637 ) ) ;
#19793 = FACE_OUTER_BOUND ( 'NONE', #11020, .T. ) ;
#19794 = FACE_BOUND ( 'NONE', #9540, .T. ) ;
#19795 = CARTESIAN_POINT ( 'NONE',  ( -43.64647580959332629, 1.256990871545142774, 60.44930799450051495 ) ) ;
#19796 = DIRECTION ( 'NONE',  ( -0.000000000000000000, -1.000000000000000000, -0.000000000000000000 ) ) ;
#19797 = ORIENTED_EDGE ( 'NONE', *, *, #8062, .T. ) ;
#19798 = DIRECTION ( 'NONE',  ( 0.000000000000000000, 0.000000000000000000, 1.000000000000000000 ) ) ;
#19799 = ORIENTED_EDGE ( 'NONE', *, *, #9440, .T. ) ;
#19800 = CARTESIAN_POINT ( 'NONE',  ( -34.86662712495122918, -3.622750763374904093, 13.44772519608141437 ) ) ;
#19801 = DIRECTION ( 'NONE',  ( 0.01254734031692010705, 0.9702957262759969170, -0.2415962909928610070 ) ) ;
#19802 = ORIENTED_EDGE ( 'NONE', *, *, #10581, .F. ) ;
#19803 = CARTESIAN_POINT ( 'NONE',  ( -41.74033427429298371, 15.41509661078533355, 35.64930799450052490 ) ) ;
#19804 = CARTESIAN_POINT ( 'NONE',  ( -42.76364231915344050, 15.12166775071174030, 35.64930799450052490 ) ) ;
#19805 = CYLINDRICAL_SURFACE ( 'NONE', #30460, 1.000000000000000666 ) ;
#19806 = LINE ( 'NONE', #17178, #28837 ) ;
#19807 = CARTESIAN_POINT ( 'NONE',  ( 46.45074414369405957, 22.93328494799376571, 48.64093701409239401 ) ) ;
#19808 = CARTESIAN_POINT ( 'NONE',  ( 45.24946171279598417, 27.02124452788248732, 47.99220971130007030 ) ) ;
#19809 = DIRECTION ( 'NONE',  ( -0.000000000000000000, -1.000000000000000000, 0.000000000000000000 ) ) ;
#19810 = CARTESIAN_POINT ( 'NONE',  ( -43.72819403793993587, 1.315833819094414769, 39.44930799450052916 ) ) ;
#19811 = VERTEX_POINT ( 'NONE', #27739 ) ;
#19812 = DIRECTION ( 'NONE',  ( 0.000000000000000000, 0.000000000000000000, 1.000000000000000000 ) ) ;
#19814 = EDGE_CURVE ( 'NONE', #28677, #2146, #24973, .T. ) ;
#19813 = DIRECTION ( 'NONE',  ( 8.659560562354994488E-17, -0.7071067811865426878, 0.7071067811865524577 ) ) ;
#19815 = CIRCLE ( 'NONE', #18742, 94.94530576803616384 ) ;
#19816 = ORIENTED_EDGE ( 'NONE', *, *, #27391, .T. ) ;
#19817 = EDGE_CURVE ( 'NONE', #27962, #21721, #21308, .T. ) ;
#19818 = AXIS2_PLACEMENT_3D ( 'NONE', #8978, #4374, #1257 ) ;
#19819 = DIRECTION ( 'NONE',  ( 0.000000000000000000, 0.000000000000000000, -1.000000000000000000 ) ) ;
#19820 = CARTESIAN_POINT ( 'NONE',  ( 21.09992658989239089, 30.34164230456639544, 47.04930799450051637 ) ) ;
#19821 = TOROIDAL_SURFACE ( 'NONE', #5674, 12.40141737965286239, 0.1250000000000005551 ) ;
#19822 = VERTEX_POINT ( 'NONE', #20985 ) ;
#19823 = VECTOR ( 'NONE', #26526, 1000.000000000000114 ) ;
#19824 = VERTEX_POINT ( 'NONE', #811 ) ;
#19825 = CARTESIAN_POINT ( 'NONE',  ( -42.66751614955960292, 15.14923148629343608, 35.64930799450052490 ) ) ;
#19826 = AXIS2_PLACEMENT_3D ( 'NONE', #11364, #21688, #21351 ) ;
#19827 = ORIENTED_EDGE ( 'NONE', *, *, #11861, .F. ) ;
#19828 = ADVANCED_FACE ( 'NONE', ( #10511 ), #20506, .F. ) ;
#19829 = ORIENTED_EDGE ( 'NONE', *, *, #12433, .T. ) ;
#19830 = LINE ( 'NONE', #2447, #13910 ) ;
#19831 = DIRECTION ( 'NONE',  ( -1.000000000000000000, 0.000000000000000000, 0.000000000000000000 ) ) ;
#19832 = AXIS2_PLACEMENT_3D ( 'NONE', #26337, #3855, #1384 ) ;
#19833 = TOROIDAL_SURFACE ( 'NONE', #5703, 44.50000000000000000, 1.000000000000000000 ) ;
#19834 = EDGE_LOOP ( 'NONE', ( #26414, #18146, #14619, #8042 ) ) ;
#19835 = CIRCLE ( 'NONE', #5707, 0.09999999999999795164 ) ;
#19836 = DIRECTION ( 'NONE',  ( -1.000000000000000000, 0.000000000000000000, 0.000000000000000000 ) ) ;
#19837 = CARTESIAN_POINT ( 'NONE',  ( 48.66895200406656130, 26.48420399681022630, 44.62753372671561181 ) ) ;
#19838 = EDGE_CURVE ( 'NONE', #10702, #17879, #23454, .T. ) ;
#19839 = CARTESIAN_POINT ( 'NONE',  ( 45.35708200440645044, 26.90457786121582018, 45.92000246470679770 ) ) ;
#19840 = ORIENTED_EDGE ( 'NONE', *, *, #19006, .F. ) ;
#19841 = EDGE_LOOP ( 'NONE', ( #14713, #22397, #9146, #3847 ) ) ;
#19842 = CARTESIAN_POINT ( 'NONE',  ( 33.50134396954520355, 30.84164230456639544, 47.04930799450051637 ) ) ;
#19843 = EDGE_LOOP ( 'NONE', ( #22085, #14111, #32434, #22202 ) ) ;
#19844 = EDGE_CURVE ( 'NONE', #15722, #7100, #1377, .T. ) ;
#19845 = AXIS2_PLACEMENT_3D ( 'NONE', #19364, #32187, #27418 ) ;
#19846 = CARTESIAN_POINT ( 'NONE',  ( -40.56956524039851075, 6.944624558150292337, 34.94636766356422442 ) ) ;
#19847 = PLANE ( 'NONE',  #7032 ) ;
#19848 = DIRECTION ( 'NONE',  ( -1.000000000000000000, 0.000000000000000000, 0.000000000000000000 ) ) ;
#19849 = CARTESIAN_POINT ( 'NONE',  ( 21.09992658989239089, 27.84143805560860940, 47.04930799450051637 ) ) ;
#19850 = CARTESIAN_POINT ( 'NONE',  ( 44.70507715278255034, 29.06291119454914806, 46.92503878583765697 ) ) ;
#19851 = VERTEX_POINT ( 'NONE', #18039 ) ;
#19852 = VERTEX_POINT ( 'NONE', #30535 ) ;
#19853 = CARTESIAN_POINT ( 'NONE',  ( 21.09785597605719332, -5.721341737285094098, 47.04930799450051637 ) ) ;
#19854 = EDGE_CURVE ( 'NONE', #13978, #15187, #863, .T. ) ;
#19855 = CARTESIAN_POINT ( 'NONE',  ( 33.62240545574881878, 32.54735957529758394, 47.04930799450051637 ) ) ;
#19856 = ADVANCED_FACE ( 'NONE', ( #8050 ), #10844, .T. ) ;
#19857 = ADVANCED_FACE ( 'NONE', ( #20336, #967 ), #31013, .T. ) ;
#19858 = DIRECTION ( 'NONE',  ( 0.000000000000000000, 1.334402673828310677E-15, 1.000000000000000000 ) ) ;
#19859 = ORIENTED_EDGE ( 'NONE', *, *, #15168, .F. ) ;
#19860 = CARTESIAN_POINT ( 'NONE',  ( 49.49063479933183629, 28.09951373492759430, 47.17357720316391578 ) ) ;
#19861 = VERTEX_POINT ( 'NONE', #15745 ) ;
#19862 = CYLINDRICAL_SURFACE ( 'NONE', #19, 0.1000000000000007272 ) ;
#19863 = CARTESIAN_POINT ( 'NONE',  ( -43.35833523721898075, -3.935454207752190126, 42.04930799450051637 ) ) ;
#19864=STYLED_ITEM('',(#32543),#23129);
#19865 = AXIS2_PLACEMENT_3D ( 'NONE', #7618, #24347, #29610 ) ;
#19866 = ADVANCED_FACE ( 'NONE', ( #28549 ), #16071, .T. ) ;
#19867 = AXIS2_PLACEMENT_3D ( 'NONE', #10839, #28555, #18521 ) ;
#19868 = ORIENTED_EDGE ( 'NONE', *, *, #31177, .F. ) ;
#19869 = CIRCLE ( 'NONE', #25131, 19.00000000000000000 ) ;
#19870 = ORIENTED_EDGE ( 'NONE', *, *, #8560, .F. ) ;
#19871 = CARTESIAN_POINT ( 'NONE',  ( -42.60588768478345401, 14.57151196022700290, 35.90717268343339441 ) ) ;
#19872 = LINE ( 'NONE', #2648, #18167 ) ;
#19873 = CARTESIAN_POINT ( 'NONE',  ( 45.96182992765472619, 28.00087065737811898, 44.82232689504102296 ) ) ;
#19874 = ORIENTED_EDGE ( 'NONE', *, *, #3298, .T. ) ;
#19875 = DIRECTION ( 'NONE',  ( 0.000000000000000000, 0.000000000000000000, 1.000000000000000000 ) ) ;
#19876 = SPHERICAL_SURFACE ( 'NONE', #2235, 0.1000000000000000056 ) ;
#19877 = EDGE_CURVE ( 'NONE', #15854, #29858, #6108, .T. ) ;
#19878 = CARTESIAN_POINT ( 'NONE',  ( 54.10256253235530721, 0.5083845707908396516, -5.656102003009075396 ) ) ;
#19879 = CIRCLE ( 'NONE', #3627, 12.36707279061065101 ) ;
#19880 = CIRCLE ( 'NONE', #9424, 2.500000000000002220 ) ;
#19881 = EDGE_CURVE ( 'NONE', #26330, #2027, #29163, .T. ) ;
#19882 = CARTESIAN_POINT ( 'NONE',  ( 21.09992658989239089, 29.09184655352418858, 47.04930799450051637 ) ) ;
#19883 = CARTESIAN_POINT ( 'NONE',  ( -41.02113223168485234, 7.230835263863472306, 39.54930799450052348 ) ) ;
#19884 = DIRECTION ( 'NONE',  ( -1.101824276508909887E-16, 1.000000000000000000, -0.000000000000000000 ) ) ;
#19885 = DIRECTION ( 'NONE',  ( 0.000000000000000000, 0.000000000000000000, -1.000000000000000000 ) ) ;
#19886 = FACE_BOUND ( 'NONE', #10363, .T. ) ;
#19887 =( NAMED_UNIT ( * ) SI_UNIT ( $, .STERADIAN. ) SOLID_ANGLE_UNIT ( ) );
#19888 = ORIENTED_EDGE ( 'NONE', *, *, #30138, .F. ) ;
#19889 = ORIENTED_EDGE ( 'NONE', *, *, #6818, .F. ) ;
#19890 = CARTESIAN_POINT ( 'NONE',  ( 47.19823469859255738, 22.88065857334294861, 45.11653766655789610 ) ) ;
#19891 = CARTESIAN_POINT ( 'NONE',  ( 21.09992658989238734, 31.46664230456641675, 47.04930799450051637 ) ) ;
#19892 = ADVANCED_FACE ( 'NONE', ( #25593, #6063 ), #15909, .T. ) ;
#19893 = DIRECTION ( 'NONE',  ( 0.000000000000000000, 0.000000000000000000, -1.000000000000000000 ) ) ;
#19894 = AXIS2_PLACEMENT_3D ( 'NONE', #9411, #23853, #11873 ) ;
#19895 = VECTOR ( 'NONE', #23053, 1000.000000000000000 ) ;
#19896 = CARTESIAN_POINT ( 'NONE',  ( 80.85108986838918099, -5.983766253076979069, 79.12126923977233162 ) ) ;
#19897 = ORIENTED_EDGE ( 'NONE', *, *, #1746, .T. ) ;
#19898 = FACE_OUTER_BOUND ( 'NONE', #2995, .T. ) ;
#19899 = AXIS2_PLACEMENT_3D ( 'NONE', #974, #10997, #20992 ) ;
#19900 = DIRECTION ( 'NONE',  ( -1.000000000000000000, 0.000000000000000000, 0.000000000000000000 ) ) ;
#19901 = CARTESIAN_POINT ( 'NONE',  ( 8.474859994195281132, 32.09184655352418503, 47.04930799450051637 ) ) ;
#19902 = ORIENTED_EDGE ( 'NONE', *, *, #13107, .F. ) ;
#19903 = ORIENTED_EDGE ( 'NONE', *, *, #15354, .F. ) ;
#19904 = CARTESIAN_POINT ( 'NONE',  ( -40.14921103274695469, 6.917687794149812497, 39.54574681281872017 ) ) ;
#19905 = CARTESIAN_POINT ( 'NONE',  ( -39.39739818181173803, -5.936374393131169214, 77.91251232197767251 ) ) ;
#19906 = AXIS2_PLACEMENT_3D ( 'NONE', #21221, #4156, #16141 ) ;
#19907 = DIRECTION ( 'NONE',  ( 0.000000000000000000, -0.000000000000000000, -1.000000000000000000 ) ) ;
#19908 = CARTESIAN_POINT ( 'NONE',  ( 8.698509210239574685, 31.09164230456639544, 47.04930799450051637 ) ) ;
#19909 = CARTESIAN_POINT ( 'NONE',  ( 44.77595935755559253, 29.32712625747106827, 47.45364450062632500 ) ) ;
#19910 = ORIENTED_EDGE ( 'NONE', *, *, #14901, .F. ) ;
#19911 = TOROIDAL_SURFACE ( 'NONE', #28313, 12.40141737965282687, 0.1250000000000004718 ) ;
#19912 = AXIS2_PLACEMENT_3D ( 'NONE', #8585, #23994, #23516 ) ;
#19913 = ORIENTED_EDGE ( 'NONE', *, *, #6116, .F. ) ;
#19914 = DIRECTION ( 'NONE',  ( -1.000000000000000000, 0.000000000000000000, 0.000000000000000000 ) ) ;
#19915 = AXIS2_PLACEMENT_3D ( 'NONE', #13604, #31805, #26394 ) ;
#19916 = TOROIDAL_SURFACE ( 'NONE', #14160, 12.61792373059896732, 0.1249999999999974604 ) ;
#19917 = VERTEX_POINT ( 'NONE', #13135 ) ;
#19918 = AXIS2_PLACEMENT_3D ( 'NONE', #25506, #20247, #3005 ) ;
#19919 = DIRECTION ( 'NONE',  ( -0.9612616959383200044, -0.2756373558169954996, 1.660411357259285896E-16 ) ) ;
#19920 = DIRECTION ( 'NONE',  ( -1.000000000000000000, -1.101824276508909887E-16, 0.000000000000000000 ) ) ;
#19921 = CONICAL_SURFACE ( 'NONE', #1592, 84.50502525316943547, 0.7853981633974621568 ) ;
#19922 = EDGE_LOOP ( 'NONE', ( #28372, #3274, #3875, #2366 ) ) ;
#19923 = DIRECTION ( 'NONE',  ( -0.2756373558169932236, 0.9612616959383204485, -1.479773560108267395E-16 ) ) ;
#19924 = EDGE_LOOP ( 'NONE', ( #17852, #8217, #30801, #28950 ) ) ;
#19925 = DIRECTION ( 'NONE',  ( -1.000000000000000000, -1.101824276508909764E-16, 0.000000000000000000 ) ) ;
#19926 = DIRECTION ( 'NONE',  ( 0.000000000000000000, 0.000000000000000000, -1.000000000000000000 ) ) ;
#19927 = CARTESIAN_POINT ( 'NONE',  ( 21.09785597605719332, -5.986312001189870280, 47.04930799450051637 ) ) ;
#19928 = DIRECTION ( 'NONE',  ( -1.101824276508909887E-16, 1.000000000000000000, -0.000000000000000000 ) ) ;
#19929 = EDGE_LOOP ( 'NONE', ( #2666, #11230, #17974, #16428 ) ) ;
#19930 = CARTESIAN_POINT ( 'NONE',  ( 71.81585295342675579, 7.161243906346035359, 76.20117120572383840 ) ) ;
#19931 = CARTESIAN_POINT ( 'NONE',  ( -43.64647580959332629, 1.256990871545142774, 53.64930799450051779 ) ) ;
#19932 = AXIS2_PLACEMENT_3D ( 'NONE', #10058, #2337, #29920 ) ;
#19933 = DIRECTION ( 'NONE',  ( 1.234978253042719660E-16, -1.000000000000000000, -1.109335647967047851E-31 ) ) ;
#19934 = ADVANCED_FACE ( 'NONE', ( #13458 ), #17887, .T. ) ;
#19935 = FACE_OUTER_BOUND ( 'NONE', #29631, .T. ) ;
#19936 = CARTESIAN_POINT ( 'NONE',  ( 73.19123048883250249, 5.308358430270040174, 77.47344046293443398 ) ) ;
#19937 = ORIENTED_EDGE ( 'NONE', *, *, #24192, .F. ) ;
#19938 = DIRECTION ( 'NONE',  ( 0.000000000000000000, 1.000000000000000000, 0.000000000000000000 ) ) ;
#19939 = CARTESIAN_POINT ( 'NONE',  ( 33.46699938050304013, 31.71183152705962272, 47.04930799450051637 ) ) ;
#19940 = VERTEX_POINT ( 'NONE', #25437 ) ;
#19941 = CYLINDRICAL_SURFACE ( 'NONE', #24028, 12.48414152717711900 ) ;
#19942 = CIRCLE ( 'NONE', #29980, 1.199999999999999734 ) ;
#19943 = AXIS2_PLACEMENT_3D ( 'NONE', #11267, #31288, #8788 ) ;
#19944 = CARTESIAN_POINT ( 'NONE',  ( 33.72499318558949000, 38.56284415653841791, 47.04930799450051637 ) ) ;
#19945 = EDGE_LOOP ( 'NONE', ( #14295, #6143, #20542, #2788 ) ) ;
#19946 = CARTESIAN_POINT ( 'NONE',  ( -37.68353499307994525, 12.01442086639228712, 60.44930799450051495 ) ) ;
#19947 = AXIS2_PLACEMENT_3D ( 'NONE', #18073, #22997, #24985 ) ;
#19948 = ORIENTED_EDGE ( 'NONE', *, *, #21474, .T. ) ;
#19949 = CIRCLE ( 'NONE', #8410, 0.9999999999999940048 ) ;
#19950 = AXIS2_PLACEMENT_3D ( 'NONE', #29568, #7073, #17074 ) ;
#19951 = CIRCLE ( 'NONE', #2123, 1.799999999999998490 ) ;
#19952 = ORIENTED_EDGE ( 'NONE', *, *, #28144, .F. ) ;
#19953 = CIRCLE ( 'NONE', #561, 0.1000000000000028644 ) ;
#19954 = CARTESIAN_POINT ( 'NONE',  ( -41.56459318755936749, 7.281738416154046156, 53.64930799450051779 ) ) ;
#19955 = ORIENTED_EDGE ( 'NONE', *, *, #19782, .T. ) ;
#19956 = ORIENTED_EDGE ( 'NONE', *, *, #5054, .F. ) ;
#19957 = CARTESIAN_POINT ( 'NONE',  ( 76.91269118277453742, -4.491775094913941224, 13.81757365283580796 ) ) ;
#19958 = DIRECTION ( 'NONE',  ( -1.101824276508909887E-16, 1.000000000000000000, -0.000000000000000000 ) ) ;
#19959 = AXIS2_PLACEMENT_3D ( 'NONE', #29024, #6539, #26556 ) ;
#19960 = DIRECTION ( 'NONE',  ( -1.101824276508909887E-16, 1.000000000000000000, -0.000000000000000000 ) ) ;
#19961 = CARTESIAN_POINT ( 'NONE',  ( 21.09785597605719332, 13.06454579224780055, 47.04930799450051637 ) ) ;
#19962 = LINE ( 'NONE', #29993, #8935 ) ;
#19963 = AXIS2_PLACEMENT_3D ( 'NONE', #27359, #4878, #7508 ) ;
#19964 = ORIENTED_EDGE ( 'NONE', *, *, #3361, .F. ) ;
#19965 = CARTESIAN_POINT ( 'NONE',  ( 21.09785597605720042, -13.98292989133646103, 47.04930799450051637 ) ) ;
#19966 = ORIENTED_EDGE ( 'NONE', *, *, #25855, .T. ) ;
#19967 = DIRECTION ( 'NONE',  ( -0.3213166889719794583, -0.7071067811865470176, -0.6298853748009115572 ) ) ;
#19968 = DIRECTION ( 'NONE',  ( 1.234978253042719660E-16, -1.000000000000000000, -1.109335647967047851E-31 ) ) ;
#19969 = CIRCLE ( 'NONE', #12113, 1.899999999999999023 ) ;
#19970 = ORIENTED_EDGE ( 'NONE', *, *, #30, .T. ) ;
#19971 = FACE_OUTER_BOUND ( 'NONE', #17263, .T. ) ;
#19972 = DIRECTION ( 'NONE',  ( -0.9612616959383205595, -0.2756373558169932236, 1.660411357259282445E-16 ) ) ;
#19973 = FACE_OUTER_BOUND ( 'NONE', #22071, .T. ) ;
#19974 = DIRECTION ( 'NONE',  ( -1.000000000000000000, 0.000000000000000000, 0.000000000000000000 ) ) ;
#19975 = CARTESIAN_POINT ( 'NONE',  ( 0.6836613156275053171, 11.92558985988973497, -37.95069200549950494 ) ) ;
#19976 = EDGE_CURVE ( 'NONE', #30857, #30310, #19196, .T. ) ;
#19977 = EDGE_CURVE ( 'NONE', #17800, #10801, #11883, .T. ) ;
#19978 = CARTESIAN_POINT ( 'NONE',  ( 46.99023568444673060, 29.23791119454914877, 49.12151524109405898 ) ) ;
#19979 = EDGE_CURVE ( 'NONE', #10074, #4416, #15034, .T. ) ;
#19980 = DIRECTION ( 'NONE',  ( 1.000000000000000000, 0.000000000000000000, 1.224646799147353207E-16 ) ) ;
#19981 = DIRECTION ( 'NONE',  ( -1.000000000000000000, 0.000000000000000000, 0.000000000000000000 ) ) ;
#19982 = EDGE_CURVE ( 'NONE', #2064, #13866, #26537, .T. ) ;
#19983 = EDGE_CURVE ( 'NONE', #20832, #24454, #28653, .T. ) ;
#19984 = ORIENTED_EDGE ( 'NONE', *, *, #27305, .T. ) ;
#19985 = DIRECTION ( 'NONE',  ( 0.9612616959383194493, 0.2756373558169974980, 8.795445018804946186E-19 ) ) ;
#19986 = DIRECTION ( 'NONE',  ( 0.000000000000000000, 1.000000000000000000, -0.000000000000000000 ) ) ;
#19987 = EDGE_LOOP ( 'NONE', ( #2446, #7527, #850, #24305 ) ) ;
#19988 = AXIS2_PLACEMENT_3D ( 'NONE', #19090, #9101, #9427 ) ;
#19989 = DIRECTION ( 'NONE',  ( 0.000000000000000000, -1.000000000000000000, 0.000000000000000000 ) ) ;
#19990 = ORIENTED_EDGE ( 'NONE', *, *, #8808, .F. ) ;
#19991 = EDGE_LOOP ( 'NONE', ( #27070, #6588, #29386, #2129 ) ) ;
#19992 = AXIS2_PLACEMENT_3D ( 'NONE', #12238, #15180, #15654 ) ;
#19993 = ORIENTED_EDGE ( 'NONE', *, *, #4667, .F. ) ;
#19994 = AXIS2_PLACEMENT_3D ( 'NONE', #15346, #7483, #12245 ) ;
#19995 = VECTOR ( 'NONE', #4510, 1000.000000000000000 ) ;
#19996 = ORIENTED_EDGE ( 'NONE', *, *, #29232, .F. ) ;
#19997 = CARTESIAN_POINT ( 'NONE',  ( 45.65205965770037011, 22.98879437201065912, 47.30685321458182813 ) ) ;
#19998 = EDGE_CURVE ( 'NONE', #31745, #12208, #12948, .T. ) ;
#19999 = CIRCLE ( 'NONE', #1139, 19.21451602543517367 ) ;
#20000 = EDGE_CURVE ( 'NONE', #22418, #26434, #29028, .T. ) ;
#20001 = ORIENTED_EDGE ( 'NONE', *, *, #18520, .F. ) ;
#20002 = FILL_AREA_STYLE_COLOUR ( '', #6232 ) ;
#20003 = FACE_OUTER_BOUND ( 'NONE', #473, .T. ) ;
#20004 = CARTESIAN_POINT ( 'NONE',  ( -9.975557855541882901, -5.936694392936853859, -13.32360845848466013 ) ) ;
#20005 = CARTESIAN_POINT ( 'NONE',  ( 48.18662509608405031, 27.19624452788248803, 49.18364984542562013 ) ) ;
#20006 = ORIENTED_EDGE ( 'NONE', *, *, #2797, .T. ) ;
#20007 = ORIENTED_EDGE ( 'NONE', *, *, #15268, .T. ) ;
#20008 = DIRECTION ( 'NONE',  ( -1.000000000000000000, -1.101824276508909887E-16, 0.000000000000000000 ) ) ;
#20009 = ORIENTED_EDGE ( 'NONE', *, *, #22300, .T. ) ;
#20010 = CARTESIAN_POINT ( 'NONE',  ( 21.09992658989239089, 24.59143805560860940, 47.04930799450051637 ) ) ;
#20011 = AXIS2_PLACEMENT_3D ( 'NONE', #22883, #393, #28301 ) ;
#20012 = DIRECTION ( 'NONE',  ( -1.101824276508909887E-16, 1.000000000000000000, -0.000000000000000000 ) ) ;
#20013 = FACE_OUTER_BOUND ( 'NONE', #21177, .T. ) ;
#20014 = AXIS2_PLACEMENT_3D ( 'NONE', #16520, #4220, #6519 ) ;
#20015 = TOROIDAL_SURFACE ( 'NONE', #25777, 12.40141737965287838, 0.1249999999999998335 ) ;
#20016 = LINE ( 'NONE', #5087, #6849 ) ;
#20017 = CARTESIAN_POINT ( 'NONE',  ( 48.04075769285628894, 25.09624452788247950, 48.89770225776209855 ) ) ;
#20018 = ADVANCED_FACE ( 'NONE', ( #24418 ), #26023, .T. ) ;
#20019 = SHAPE_DEFINITION_REPRESENTATION ( #14818, #17018 ) ;
#20020 = VERTEX_POINT ( 'NONE', #6543 ) ;
#20021 = ORIENTED_EDGE ( 'NONE', *, *, #7650, .T. ) ;
#20022 = DIRECTION ( 'NONE',  ( 1.000000000000000000, 0.000000000000000000, 0.000000000000000000 ) ) ;
#20023 = LINE ( 'NONE', #19692, #19344 ) ;
#20024 = ORIENTED_EDGE ( 'NONE', *, *, #1711, .T. ) ;
#20025 = ORIENTED_EDGE ( 'NONE', *, *, #29698, .T. ) ;
#20026 = CARTESIAN_POINT ( 'NONE',  ( 8.698509210239516065, 25.09164230456639899, 47.04930799450051637 ) ) ;
#20027 = AXIS2_PLACEMENT_3D ( 'NONE', #4516, #6980, #32098 ) ;
#20028 = PLANE ( 'NONE',  #28568 ) ;
#20029 = CONICAL_SURFACE ( 'NONE', #4832, 72.49999999999997158, 0.7853981633974482790 ) ;
#20030 = EDGE_CURVE ( 'NONE', #13402, #19462, #21135, .T. ) ;
#20032 = ADVANCED_FACE ( 'NONE', ( #1278 ), #31172, .F. ) ;
#20031 = CIRCLE ( 'NONE', #5390, 12.36707279061065101 ) ;
#20033 = ORIENTED_EDGE ( 'NONE', *, *, #15999, .F. ) ;
#20034 = AXIS2_PLACEMENT_3D ( 'NONE', #20550, #22850, #26242 ) ;
#20035 = ORIENTED_EDGE ( 'NONE', *, *, #32281, .T. ) ;
#20036 = CIRCLE ( 'NONE', #22663, 0.1249999999999983763 ) ;
#20037 = CARTESIAN_POINT ( 'NONE',  ( -37.45475073248209696, -5.768184894878238822, 15.30568074843956516 ) ) ;
#20038 = EDGE_CURVE ( 'NONE', #10875, #22237, #32321, .T. ) ;
#20039 = LINE ( 'NONE', #2163, #5590 ) ;
#20040 = CARTESIAN_POINT ( 'NONE',  ( 21.09992658989239089, 27.59164230456639544, 47.04930799450051637 ) ) ;
#20041 = EDGE_CURVE ( 'NONE', #12393, #29883, #30750, .T. ) ;
#20042 = EDGE_LOOP ( 'NONE', ( #2590, #30012, #3932, #29550 ) ) ;
#20043 = FACE_OUTER_BOUND ( 'NONE', #28270, .T. ) ;
#20044 = CARTESIAN_POINT ( 'NONE',  ( 21.09785597605719332, 48.06454579224779877, 47.04930799450051637 ) ) ;
#20045 = CARTESIAN_POINT ( 'NONE',  ( 45.00053793792376666, 27.23655426599985674, 45.68869892245983522 ) ) ;
#20046 = CARTESIAN_POINT ( 'NONE',  ( 45.96182992765471909, 15.77906836436399374, 44.82232689504101586 ) ) ;
#20047 = CARTESIAN_POINT ( 'NONE',  ( 21.09785597605719332, -19.93545420775220123, 47.04930799450051637 ) ) ;
#20048 = CARTESIAN_POINT ( 'NONE',  ( -40.02540636251513462, 2.839176264122874382, 35.14930799450051779 ) ) ;
#20049 = CARTESIAN_POINT ( 'NONE',  ( -40.02540636251513462, 2.839176264122874382, 38.94930799450052206 ) ) ;
#20050 = FACE_OUTER_BOUND ( 'NONE', #12297, .T. ) ;
#20051 = DIRECTION ( 'NONE',  ( 0.000000000000000000, -0.000000000000000000, -1.000000000000000000 ) ) ;
#20052 = AXIS2_PLACEMENT_3D ( 'NONE', #16091, #1000, #1154 ) ;
#20053 = PRODUCT ( 'Membrane', 'Membrane', '', ( #30046 ) ) ;
#20054 = FACE_OUTER_BOUND ( 'NONE', #16403, .T. ) ;
#20055 = TOROIDAL_SURFACE ( 'NONE', #32126, 12.40141737965288371, 0.1249999999999996253 ) ;
#20056 = CARTESIAN_POINT ( 'NONE',  ( 34.59963999142011204, 16.03967147762301693, 47.04930799450052348 ) ) ;
#20057 = ADVANCED_FACE ( 'NONE', ( #26559 ), #18831, .F. ) ;
#20058 = ORIENTED_EDGE ( 'NONE', *, *, #21260, .F. ) ;
#20059 = VERTEX_POINT ( 'NONE', #6216 ) ;
#20060 = FACE_OUTER_BOUND ( 'NONE', #23742, .T. ) ;
#20061 = CARTESIAN_POINT ( 'NONE',  ( 33.37634396954519644, 31.34164230456639544, 47.04930799450051637 ) ) ;
#20062 = AXIS2_PLACEMENT_3D ( 'NONE', #14406, #14082, #26706 ) ;
#20063 = CARTESIAN_POINT ( 'NONE',  ( 21.09785597605719332, -15.72540370141337007, 118.3493079945004922 ) ) ;
#20064 = CARTESIAN_POINT ( 'NONE',  ( 8.823509210239571132, 30.34164230456639544, 47.04930799450051637 ) ) ;
#20065 = ORIENTED_EDGE ( 'NONE', *, *, #31621, .F. ) ;
#20066 = CIRCLE ( 'NONE', #15884, 0.1250000000000001110 ) ;
#20067 = DIRECTION ( 'NONE',  ( -0.000000000000000000, 1.000000000000000000, -0.000000000000000000 ) ) ;
#20068 = CARTESIAN_POINT ( 'NONE',  ( -40.12057988072736237, 7.355395738388401661, 38.85629451012739111 ) ) ;
#20069 = CARTESIAN_POINT ( 'NONE',  ( 46.84806919170409145, 10.40257568944042887, -3.470939490021768936 ) ) ;
#20070 = ORIENTED_EDGE ( 'NONE', *, *, #14231, .T. ) ;
#20071 = ORIENTED_EDGE ( 'NONE', *, *, #27161, .F. ) ;
#20072 = DIRECTION ( 'NONE',  ( 0.000000000000000000, 0.9550631830613039996, 0.2964022880492153122 ) ) ;
#20073 = CARTESIAN_POINT ( 'NONE',  ( 49.49063479933183629, 27.39951373492759856, 47.17357720316391578 ) ) ;
#20074 = CARTESIAN_POINT ( 'NONE',  ( -14.16142858629410028, -3.295808585244882849, -12.62465409255485582 ) ) ;
#20075 = DIRECTION ( 'NONE',  ( -1.224646799147353207E-16, -1.349345573449484691E-32, 1.000000000000000000 ) ) ;
#20076 = CARTESIAN_POINT ( 'NONE',  ( 45.43273841042186234, 29.36740968959510312, 48.63901743999641525 ) ) ;
#20077 = EDGE_CURVE ( 'NONE', #13126, #14963, #16867, .T. ) ;
#20078 = EDGE_LOOP ( 'NONE', ( #26564, #17010, #320, #17133 ) ) ;
#20079 = AXIS2_PLACEMENT_3D ( 'NONE', #10831, #15572, #22953 ) ;
#20080 = CIRCLE ( 'NONE', #10132, 1.500000000000001332 ) ;
#20081 = DIRECTION ( 'NONE',  ( -1.101824276508909887E-16, 1.000000000000000000, -0.000000000000000000 ) ) ;
#20082 = EDGE_CURVE ( 'NONE', #11143, #4372, #27082, .T. ) ;
#20083 = ORIENTED_EDGE ( 'NONE', *, *, #11399, .F. ) ;
#20084 = EDGE_CURVE ( 'NONE', #17431, #24463, #13776, .T. ) ;
#20085 = AXIS2_PLACEMENT_3D ( 'NONE', #25911, #13455, #15742 ) ;
#20086 = DIRECTION ( 'NONE',  ( -1.000000000000000000, 0.000000000000000000, 0.000000000000000000 ) ) ;
#20087 = DIRECTION ( 'NONE',  ( 0.000000000000000000, 0.000000000000000000, -1.000000000000000000 ) ) ;
#20088 = ORIENTED_EDGE ( 'NONE', *, *, #32053, .T. ) ;
#20089 = CARTESIAN_POINT ( 'NONE',  ( -40.28779227465695101, 2.984619150196775372, 35.54930799450051637 ) ) ;
#20090 = ORIENTED_EDGE ( 'NONE', *, *, #24482, .T. ) ;
#20091 = CARTESIAN_POINT ( 'NONE',  ( 21.09785597605733187, -5.935454207752083988, 47.04930799450051637 ) ) ;
#20092 = DIRECTION ( 'NONE',  ( -1.224646799147353207E-16, 0.000000000000000000, -1.000000000000000000 ) ) ;
#20093 = CARTESIAN_POINT ( 'NONE',  ( -43.68921302925062378, 1.179890886355839275, 34.64930799450052490 ) ) ;
#20094 = CARTESIAN_POINT ( 'NONE',  ( -40.69569484204229326, 6.786538238944499923, 39.45224069363045061 ) ) ;
#20095 = VERTEX_POINT ( 'NONE', #26401 ) ;
#20096 = DIRECTION ( 'NONE',  ( -1.101824276508909887E-16, 1.000000000000000000, -0.000000000000000000 ) ) ;
#20097 = CARTESIAN_POINT ( 'NONE',  ( 21.09992658989238734, 30.84164230456639544, 47.04930799450051637 ) ) ;
#20098 = DIRECTION ( 'NONE',  ( -1.101824276508909887E-16, 1.000000000000000000, -0.000000000000000000 ) ) ;
#20099 = DIRECTION ( 'NONE',  ( 0.000000000000000000, 0.000000000000000000, -1.000000000000000000 ) ) ;
#20100 = CIRCLE ( 'NONE', #26370, 72.49999999999997158 ) ;
#20101 = CARTESIAN_POINT ( 'NONE',  ( 74.01572245777501280, 2.529769287487848128, 79.09906317329492254 ) ) ;
#20102 = ORIENTED_EDGE ( 'NONE', *, *, #9617, .F. ) ;
#20103 = DIRECTION ( 'NONE',  ( -1.101824276508909887E-16, 1.000000000000000000, -0.000000000000000000 ) ) ;
#20104 = LINE ( 'NONE', #15030, #9120 ) ;
#20105 = AXIS2_PLACEMENT_3D ( 'NONE', #24654, #2173, #9234 ) ;
#20106 = ORIENTED_EDGE ( 'NONE', *, *, #27476, .F. ) ;
#20107 = DIRECTION ( 'NONE',  ( -1.000000000000000000, 0.000000000000000000, 0.000000000000000000 ) ) ;
#20108 = CARTESIAN_POINT ( 'NONE',  ( 8.732853799281732776, 32.22145308207317527, 47.04930799450051637 ) ) ;
#20109 = VECTOR ( 'NONE', #25033, 1000.000000000000000 ) ;
#20110 = ORIENTED_EDGE ( 'NONE', *, *, #21792, .F. ) ;
#20111 = VECTOR ( 'NONE', #25005, 1000.000000000000114 ) ;
#20112 = DIRECTION ( 'NONE',  ( -1.000000000000000000, 0.000000000000000000, 0.000000000000000000 ) ) ;
#20113 = EDGE_LOOP ( 'NONE', ( #27564, #20863, #16415 ) ) ;
#20114 = EDGE_CURVE ( 'NONE', #26617, #5208, #11359, .T. ) ;
#20115 = ORIENTED_EDGE ( 'NONE', *, *, #15843, .F. ) ;
#20116 = EDGE_CURVE ( 'NONE', #5658, #1265, #9001, .T. ) ;
#20117 = ADVANCED_FACE ( 'NONE', ( #16539 ), #29186, .F. ) ;
#20118 = AXIS2_PLACEMENT_3D ( 'NONE', #9055, #4458, #13991 ) ;
#20119 = CARTESIAN_POINT ( 'NONE',  ( -9.843081575490945312, -5.936629510748248073, 107.7114293576719604 ) ) ;
#20120 = ORIENTED_EDGE ( 'NONE', *, *, #17078, .F. ) ;
#20121 = ORIENTED_EDGE ( 'NONE', *, *, #28985, .T. ) ;
#20122 = CARTESIAN_POINT ( 'NONE',  ( 79.10241889060681331, -5.935454207752202116, 16.07118271501078510 ) ) ;
#20123 = AXIS2_PLACEMENT_3D ( 'NONE', #9286, #19453, #14379 ) ;
#20124 = DIRECTION ( 'NONE',  ( -0.000000000000000000, -1.000000000000000000, -0.000000000000000000 ) ) ;
#20125 = CARTESIAN_POINT ( 'NONE',  ( 67.77233896511883415, 14.36454579224780126, 47.04930799450051637 ) ) ;
#20126 = DIRECTION ( 'NONE',  ( -1.101824276508909887E-16, 1.000000000000000000, -0.000000000000000000 ) ) ;
#20127 = CARTESIAN_POINT ( 'NONE',  ( 21.09992658989239089, 26.84164230456639899, 47.04930799450051637 ) ) ;
#20128 = ORIENTED_EDGE ( 'NONE', *, *, #26902, .F. ) ;
#20129 = CARTESIAN_POINT ( 'NONE',  ( -12.39242563034483169, -3.977894809549909816, 102.3767317286982603 ) ) ;
#20130 = ORIENTED_EDGE ( 'NONE', *, *, #28609, .T. ) ;
#20131 = CARTESIAN_POINT ( 'NONE',  ( 21.09992658989239089, 28.84143805560861296, 47.04930799450051637 ) ) ;
#20132 = DIRECTION ( 'NONE',  ( 0.8746197071393928546, -0.4848096202463424986, -1.277302113040826515E-17 ) ) ;
#20133 = EDGE_LOOP ( 'NONE', ( #6645, #13682, #1995, #31439 ) ) ;
#20134 = CARTESIAN_POINT ( 'NONE',  ( 21.09992658989239089, 28.21183152705961206, 47.04930799450051637 ) ) ;
#20135 = DIRECTION ( 'NONE',  ( -1.000000000000000000, -1.101824276508910010E-16, 0.000000000000000000 ) ) ;
#20136 = CARTESIAN_POINT ( 'NONE',  ( 81.72488390788849699, -5.936701049740617187, 16.03361580170941991 ) ) ;
#20137 = DIRECTION ( 'NONE',  ( -0.000000000000000000, -1.000000000000000000, -0.000000000000000000 ) ) ;
#20138 = CARTESIAN_POINT ( 'NONE',  ( 33.37634396954525329, 25.84164230456639899, 47.04930799450051637 ) ) ;
#20139 = CARTESIAN_POINT ( 'NONE',  ( 48.83862994770794330, 28.65457786121581663, 48.17861352429476796 ) ) ;
#20140 = CARTESIAN_POINT ( 'NONE',  ( -40.01416947921581624, 7.179266651196238413, 35.24167910030048034 ) ) ;
#20141 = CARTESIAN_POINT ( 'NONE',  ( 8.482002859293400476, 24.46664230456639899, 47.04930799450051637 ) ) ;
#20142 = EDGE_LOOP ( 'NONE', ( #3537, #26045, #18907, #8798 ) ) ;
#20143 = DIRECTION ( 'NONE',  ( -1.000000000000000000, 0.000000000000000000, 0.000000000000000000 ) ) ;
#20144 = VERTEX_POINT ( 'NONE', #24092 ) ;
#20145 = DIRECTION ( 'NONE',  ( -1.000000000000000000, 0.000000000000000000, 0.000000000000000000 ) ) ;
#20146 = ORIENTED_EDGE ( 'NONE', *, *, #1338, .T. ) ;
#20147 = VECTOR ( 'NONE', #13035, 1000.000000000000227 ) ;
#20148 = EDGE_LOOP ( 'NONE', ( #9340, #28153, #21610 ) ) ;
#20149 = DIRECTION ( 'NONE',  ( -1.000000000000000000, 0.000000000000000000, 0.000000000000000000 ) ) ;
#20150 = VECTOR ( 'NONE', #22752, 1000.000000000000000 ) ;
#20151 = CIRCLE ( 'NONE', #783, 34.00000000000000000 ) ;
#20152 = AXIS2_PLACEMENT_3D ( 'NONE', #26778, #19543, #2162 ) ;
#20153 = ORIENTED_EDGE ( 'NONE', *, *, #17249, .F. ) ;
#20154 = EDGE_CURVE ( 'NONE', #29646, #22098, #7696, .T. ) ;
#20155 = EDGE_CURVE ( 'NONE', #30180, #27550, #21827, .T. ) ;
#20156 = ADVANCED_FACE ( 'NONE', ( #2433 ), #28126, .T. ) ;
#20157 = EDGE_CURVE ( 'NONE', #14214, #24454, #21844, .T. ) ;
#20158 = ORIENTED_EDGE ( 'NONE', *, *, #13321, .F. ) ;
#20159 = EDGE_CURVE ( 'NONE', #5895, #4564, #4568, .T. ) ;
#20160 = FACE_OUTER_BOUND ( 'NONE', #4457, .T. ) ;
#20161 = EDGE_CURVE ( 'NONE', #17431, #29734, #12450, .T. ) ;
#20162 = EDGE_LOOP ( 'NONE', ( #2367, #19591, #86, #18790 ) ) ;
#20163 = CIRCLE ( 'NONE', #13367, 55.72436264418301732 ) ;
#20164 = DIRECTION ( 'NONE',  ( -1.000000000000000000, 0.000000000000000000, 0.000000000000000000 ) ) ;
#20165 = LINE ( 'NONE', #20811, #13904 ) ;
#20166 = CARTESIAN_POINT ( 'NONE',  ( -40.28779227465695101, 2.984619150196775816, 37.04930799450052348 ) ) ;
#20167 = AXIS2_PLACEMENT_3D ( 'NONE', #19882, #15134, #25142 ) ;
#20168 = CARTESIAN_POINT ( 'NONE',  ( 48.91284552371730143, 28.79289516297709284, 46.12344667017377020 ) ) ;
#20169 = ORIENTED_EDGE ( 'NONE', *, *, #1891, .T. ) ;
#20170 = EDGE_LOOP ( 'NONE', ( #9521, #12469, #8310, #6261 ) ) ;
#20171 = FACE_OUTER_BOUND ( 'NONE', #11339, .T. ) ;
#20172 = CIRCLE ( 'NONE', #16995, 0.1250000000000001110 ) ;
#20173 = ORIENTED_EDGE ( 'NONE', *, *, #7760, .F. ) ;
#20174 = DIRECTION ( 'NONE',  ( -1.101824276508909887E-16, 1.000000000000000000, -0.000000000000000000 ) ) ;
#20175 = VECTOR ( 'NONE', #6886, 1000.000000000000000 ) ;
#20176 = CARTESIAN_POINT ( 'NONE',  ( -39.67555847965937943, 2.645252416024337361, 47.04930799450051637 ) ) ;
#20177 = DIRECTION ( 'NONE',  ( 0.000000000000000000, 0.000000000000000000, -1.000000000000000000 ) ) ;
#20178 = LINE ( 'NONE', #7556, #7896 ) ;
#20179 = FACE_OUTER_BOUND ( 'NONE', #17539, .T. ) ;
#20180 =( NAMED_UNIT ( * ) PLANE_ANGLE_UNIT ( ) SI_UNIT ( $, .RADIAN. ) );
#20181 = EDGE_LOOP ( 'NONE', ( #30278, #5920, #31735, #17417 ) ) ;
#20182 = ORIENTED_EDGE ( 'NONE', *, *, #18158, .F. ) ;
#20183 = DIRECTION ( 'NONE',  ( 0.2756373558169990523, -0.9612616959383188942, 1.479773560108257288E-16 ) ) ;
#20184 = DIRECTION ( 'NONE',  ( -0.000000000000000000, -1.000000000000000000, 0.000000000000000000 ) ) ;
#20185 = DIRECTION ( 'NONE',  ( -1.000000000000000000, -1.101824276508909887E-16, 0.000000000000000000 ) ) ;
#20186 = ORIENTED_EDGE ( 'NONE', *, *, #13601, .T. ) ;
#20187 = CARTESIAN_POINT ( 'NONE',  ( 48.83862994770794330, 28.04118040159426428, 48.17861352429476796 ) ) ;
#20188 = ORIENTED_EDGE ( 'NONE', *, *, #29046, .T. ) ;
#20189 = CARTESIAN_POINT ( 'NONE',  ( 21.09785597605720753, -5.098646251524523443, 47.04930799450052348 ) ) ;
#20190 = CARTESIAN_POINT ( 'NONE',  ( -40.50720532202722524, 7.584939507552746818, 59.44930799450051495 ) ) ;
#20191 = ADVANCED_FACE ( 'NONE', ( #11950 ), #24920, .F. ) ;
#20192 = DIRECTION ( 'NONE',  ( 0.4848096202463430537, 0.8746197071393926326, -1.125439520643636483E-16 ) ) ;
#20193 = CIRCLE ( 'NONE', #22274, 0.2000000000000057288 ) ;
#20194 =( BOUNDED_CURVE ( )  B_SPLINE_CURVE ( 3, ( #30845, #961, #28542, #26062 ),
 .UNSPECIFIED., .F., .F. ) 
 B_SPLINE_CURVE_WITH_KNOTS ( ( 4, 4 ),
 ( 1.099063246724954146, 1.220321128156879320 ),
 .UNSPECIFIED. ) 
 CURVE ( )  GEOMETRIC_REPRESENTATION_ITEM ( )  RATIONAL_B_SPLINE_CURVE ( ( 1.000000000000000000, 0.9987750858034805113, 0.9987750858034805113, 1.000000000000000000 ) ) 
 REPRESENTATION_ITEM ( '' )  );
#20195 = CIRCLE ( 'NONE', #5000, 1.200000000000003064 ) ;
#20196 = CIRCLE ( 'NONE', #24389, 0.1250000000000001110 ) ;
#20197 = CIRCLE ( 'NONE', #20722, 12.52641737965279489 ) ;
#20198 = ORIENTED_EDGE ( 'NONE', *, *, #32405, .F. ) ;
#20199 = ADVANCED_FACE ( 'NONE', ( #32469 ), #7525, .F. ) ;
#20200 = EDGE_CURVE ( 'NONE', #21395, #11200, #8758, .T. ) ;
#20201 = ORIENTED_EDGE ( 'NONE', *, *, #1801, .F. ) ;
#20202 = EDGE_CURVE ( 'NONE', #20095, #17152, #30615, .T. ) ;
#20203 = DIRECTION ( 'NONE',  ( -1.101824276508909887E-16, 1.000000000000000000, -0.000000000000000000 ) ) ;
#20204 = CARTESIAN_POINT ( 'NONE',  ( 21.09785597605719332, 25.56454579224779167, 47.04930799450051637 ) ) ;
#20205 = CARTESIAN_POINT ( 'NONE',  ( 48.83862994770794330, 27.34118040159426499, 48.17861352429476796 ) ) ;
#20206 = ORIENTED_EDGE ( 'NONE', *, *, #22250, .F. ) ;
#20207 = DIRECTION ( 'NONE',  ( -0.000000000000000000, -1.000000000000000000, 0.000000000000000000 ) ) ;
#20208 = DIRECTION ( 'NONE',  ( 0.000000000000000000, 0.000000000000000000, -1.000000000000000000 ) ) ;
#20209 = CARTESIAN_POINT ( 'NONE',  ( 47.63716429968717136, 27.49696019071910769, 49.58068632438585155 ) ) ;
#20210 = CARTESIAN_POINT ( 'NONE',  ( 21.09992658989239089, 25.09143805560860940, 47.04930799450051637 ) ) ;
#20211 = DIRECTION ( 'NONE',  ( 7.588956326749211550E-18, -4.206627182996911684E-18, 1.000000000000000000 ) ) ;
#20212 = CARTESIAN_POINT ( 'NONE',  ( 21.09992658989238734, 38.56284415653841791, 47.04930799450051637 ) ) ;
#20213 = CARTESIAN_POINT ( 'NONE',  ( -40.59307409811868439, 7.534955591098723815, 60.26126833232958546 ) ) ;
#20214 = DIRECTION ( 'NONE',  ( 0.3428121700606640565, 0.6184495258776567805, 0.7071067811865474617 ) ) ;
#20215 = CARTESIAN_POINT ( 'NONE',  ( 49.00637973737335074, 20.36454579224780304, 50.79063624159320511 ) ) ;
#20216 = ORIENTED_EDGE ( 'NONE', *, *, #3249, .T. ) ;
#20217 = VERTEX_POINT ( 'NONE', #8127 ) ;
#20218 = CARTESIAN_POINT ( 'NONE',  ( 8.823575513742490273, 15.24673779880127356, 46.72789464899623368 ) ) ;
#20219 = VECTOR ( 'NONE', #391, 1000.000000000000000 ) ;
#20220 = PRESENTATION_LAYER_ASSIGNMENT (  '', '', ( #14473 ) ) ;
#20221 = CARTESIAN_POINT ( 'NONE',  ( 46.71168188241476571, 25.16454579224780019, 44.57931415454905988 ) ) ;
#20222 = EDGE_CURVE ( 'NONE', #6305, #26270, #10343, .T. ) ;
#20223 = DIRECTION ( 'NONE',  ( 2.779292025043186357E-18, -1.288349127009862211E-17, 1.000000000000000000 ) ) ;
#20224 = CARTESIAN_POINT ( 'NONE',  ( 50.24465560486001436, 7.198184577528759398, 97.74814760920997969 ) ) ;
#20225 = EDGE_LOOP ( 'NONE', ( #30842, #28259 ) ) ;
#20226 = CARTESIAN_POINT ( 'NONE',  ( 21.09992658989238734, 32.09143805560860585, 47.04930799450051637 ) ) ;
#20227 = DIRECTION ( 'NONE',  ( -6.722685822323786766E-17, 1.000000000000000000, -0.000000000000000000 ) ) ;
#20228 = CARTESIAN_POINT ( 'NONE',  ( -43.64647580959332629, 1.256990871545142774, 53.64930799450051779 ) ) ;
#20229 = VERTEX_POINT ( 'NONE', #18123 ) ;
#20230 = ORIENTED_EDGE ( 'NONE', *, *, #29455, .T. ) ;
#20231 = CARTESIAN_POINT ( 'NONE',  ( -38.36853489569023168, 7.065850718397948427, 62.04930799450052348 ) ) ;
#20232 = CARTESIAN_POINT ( 'NONE',  ( 45.35708200440645044, 28.39118040159425860, 45.92000246470679770 ) ) ;
#20233 = ADVANCED_FACE ( 'NONE', ( #29682 ), #9656, .F. ) ;
#20234 = EDGE_CURVE ( 'NONE', #5971, #20242, #24472, .T. ) ;
#20235 = DIRECTION ( 'NONE',  ( 0.000000000000000000, 0.000000000000000000, -1.000000000000000000 ) ) ;
#20236 = DIRECTION ( 'NONE',  ( -0.9612616959383221138, -0.2756373558169876170, 1.387778780781420432E-13 ) ) ;
#20237 = DIRECTION ( 'NONE',  ( -1.000000000000000000, -0.000000000000000000, -0.000000000000000000 ) ) ;
#20238 = EDGE_LOOP ( 'NONE', ( #8359, #14588 ) ) ;
#20239 = EDGE_CURVE ( 'NONE', #30184, #23467, #7718, .T. ) ;
#20240 = DIRECTION ( 'NONE',  ( -1.000000000000000000, 0.000000000000000000, 0.000000000000000000 ) ) ;
#20241 = AXIS2_PLACEMENT_3D ( 'NONE', #18871, #9204, #12324 ) ;
#20242 = VERTEX_POINT ( 'NONE', #24752 ) ;
#20243 = CARTESIAN_POINT ( 'NONE',  ( -9.728297238921257417, -5.935454207752202116, 107.7511683020618278 ) ) ;
#20244 = EDGE_LOOP ( 'NONE', ( #10813, #7924, #14311, #24878 ) ) ;
#20245 = DIRECTION ( 'NONE',  ( 0.000000000000000000, -0.000000000000000000, -1.000000000000000000 ) ) ;
#20246 = ORIENTED_EDGE ( 'NONE', *, *, #10857, .T. ) ;
#20247 = DIRECTION ( 'NONE',  ( 0.000000000000000000, -0.000000000000000000, -1.000000000000000000 ) ) ;
#20248 = FACE_OUTER_BOUND ( 'NONE', #25559, .T. ) ;
#20249 = ADVANCED_FACE ( 'NONE', ( #19650 ), #29196, .T. ) ;
#20250 = DIRECTION ( 'NONE',  ( -1.000000000000000000, 0.000000000000000000, 0.000000000000000000 ) ) ;
#20251 = DIRECTION ( 'NONE',  ( -1.000000000000000000, -0.000000000000000000, -3.491481338843133355E-15 ) ) ;
#20252 = ORIENTED_EDGE ( 'NONE', *, *, #31090, .T. ) ;
#20253 = DIRECTION ( 'NONE',  ( -1.101824276508909887E-16, 1.000000000000000000, -0.000000000000000000 ) ) ;
#20254 = CARTESIAN_POINT ( 'NONE',  ( -9.917836216733666888, -5.936701049740607417, -13.57771993733065408 ) ) ;
#20255 = DIRECTION ( 'NONE',  ( -1.224646799147353207E-16, -1.349345573449484691E-32, 1.000000000000000000 ) ) ;
#20256 = EDGE_CURVE ( 'NONE', #19350, #11589, #1788, .T. ) ;
#20257 = CARTESIAN_POINT ( 'NONE',  ( 21.09785597605720753, 13.78276522714992147, 47.04930799450052348 ) ) ;
#20258 = DIRECTION ( 'NONE',  ( -1.000000000000000000, 0.000000000000000000, 0.000000000000000000 ) ) ;
#20259 = ORIENTED_EDGE ( 'NONE', *, *, #17533, .T. ) ;
#20260 = CARTESIAN_POINT ( 'NONE',  ( 21.09785597605719332, 14.77459629858661572, 47.04930799450051637 ) ) ;
#20261 = ORIENTED_EDGE ( 'NONE', *, *, #25532, .T. ) ;
#20262 = CARTESIAN_POINT ( 'NONE',  ( -10.00793156682730611, -5.936611295272323119, -12.50776140503650247 ) ) ;
#20263 = DIRECTION ( 'NONE',  ( 1.000000000000000000, -0.000000000000000000, -0.000000000000000000 ) ) ;
#20264 = EDGE_CURVE ( 'NONE', #18076, #14754, #31254, .T. ) ;
#20265 = CARTESIAN_POINT ( 'NONE',  ( 21.09785597605719332, 15.06454579224778456, 47.04930799450051637 ) ) ;
#20266 = EDGE_CURVE ( 'NONE', #18233, #14305, #22907, .T. ) ;
#20267 = CARTESIAN_POINT ( 'NONE',  ( 21.09785597605719332, 25.56454579224780232, -32.16074251183835031 ) ) ;
#20268 = EDGE_CURVE ( 'NONE', #8613, #16662, #12974, .T. ) ;
#20269 = ORIENTED_EDGE ( 'NONE', *, *, #2641, .F. ) ;
#20270 = DIRECTION ( 'NONE',  ( -0.000000000000000000, -1.000000000000000000, -0.000000000000000000 ) ) ;
#20271 = ORIENTED_EDGE ( 'NONE', *, *, #12318, .T. ) ;
#20272 = CIRCLE ( 'NONE', #9791, 54.29999999999999716 ) ;
#20273 = ORIENTED_EDGE ( 'NONE', *, *, #27122, .T. ) ;
#20274 = EDGE_CURVE ( 'NONE', #21967, #8138, #9278, .T. ) ;
#20275 = CARTESIAN_POINT ( 'NONE',  ( -9.728297238921253864, -5.935454207752203892, 107.6877921759662371 ) ) ;
#20276 = CARTESIAN_POINT ( 'NONE',  ( -39.58809650894544774, 2.596771453999702661, 48.34930799450052064 ) ) ;
#20277 = AXIS2_PLACEMENT_3D ( 'NONE', #15832, #6296, #13380 ) ;
#20278 = ORIENTED_EDGE ( 'NONE', *, *, #5406, .F. ) ;
#20279 = ORIENTED_EDGE ( 'NONE', *, *, #7161, .T. ) ;
#20280 = DIRECTION ( 'NONE',  ( -1.000000000000000000, 0.000000000000000000, 0.000000000000000000 ) ) ;
#20281 = DIRECTION ( 'NONE',  ( -1.000000000000000000, 0.000000000000000000, 0.000000000000000000 ) ) ;
#20282 = CARTESIAN_POINT ( 'NONE',  ( -33.09327977158311285, -0.7531705753110401469, 80.50456572937015665 ) ) ;
#20283 = EDGE_CURVE ( 'NONE', #7154, #26331, #17136, .T. ) ;
#20284 = CARTESIAN_POINT ( 'NONE',  ( -41.63422246745999189, 11.51531537899137447, 57.95249952744806166 ) ) ;
#20285 = ORIENTED_EDGE ( 'NONE', *, *, #28636, .F. ) ;
#20286 = EDGE_LOOP ( 'NONE', ( #13801, #6175, #24360, #19088 ) ) ;
#20287 = DIRECTION ( 'NONE',  ( -0.000000000000000000, -1.000000000000000000, 0.000000000000000000 ) ) ;
#20288 = CARTESIAN_POINT ( 'NONE',  ( 80.51541434188031587, -5.922252862938464091, 15.78525142915797019 ) ) ;
#20289 = ORIENTED_EDGE ( 'NONE', *, *, #26689, .T. ) ;
#20290 = CARTESIAN_POINT ( 'NONE',  ( 47.26459061581830667, 23.10527865767145173, 46.48657494263439816 ) ) ;
#20291 = EDGE_CURVE ( 'NONE', #31745, #19168, #2993, .T. ) ;
#20292 = CARTESIAN_POINT ( 'NONE',  ( 21.09785597605720753, -5.098646251524523443, 47.04930799450052348 ) ) ;
#20293 = LINE ( 'NONE', #25720, #24636 ) ;
#20294 = DIRECTION ( 'NONE',  ( 0.3435019893673572078, -0.6546536707079771977, 0.6733757901270577273 ) ) ;
#20295 = CARTESIAN_POINT ( 'NONE',  ( 49.49063479933183629, 29.41291119454914593, 47.17357720316391578 ) ) ;
#20296 = PLANE ( 'NONE',  #12664 ) ;
#20297 = DIRECTION ( 'NONE',  ( -1.000000000000000000, 0.000000000000000000, 0.000000000000000000 ) ) ;
#20298 = ORIENTED_EDGE ( 'NONE', *, *, #13597, .F. ) ;
#20299 = VERTEX_POINT ( 'NONE', #733 ) ;
#20300 = ADVANCED_FACE ( 'NONE', ( #30770 ), #28952, .T. ) ;
#20301 = CIRCLE ( 'NONE', #23448, 0.09999999999999815981 ) ;
#20302 = CARTESIAN_POINT ( 'NONE',  ( 46.96819297411687444, 28.29253733014355632, 49.54594323136014822 ) ) ;
#20303 = ADVANCED_FACE ( 'NONE', ( #16302 ), #3670, .T. ) ;
#20304 = ORIENTED_EDGE ( 'NONE', *, *, #29480, .T. ) ;
#20305 = AXIS2_PLACEMENT_3D ( 'NONE', #19381, #11610, #29006 ) ;
#20306 = ORIENTED_EDGE ( 'NONE', *, *, #22036, .T. ) ;
#20307 = DIRECTION ( 'NONE',  ( -1.000000000000000000, 0.000000000000000000, 0.000000000000000000 ) ) ;
#20308 = TOROIDAL_SURFACE ( 'NONE', #29213, 46.67448298906162307, 0.7000000000000006217 ) ;
#20309 = TOROIDAL_SURFACE ( 'NONE', #29767, 12.40141737965286239, 0.1250000000000005551 ) ;
#20310 = ORIENTED_EDGE ( 'NONE', *, *, #4793, .T. ) ;
#20311 = AXIS2_PLACEMENT_3D ( 'NONE', #10269, #30610, #729 ) ;
#20312 = CONICAL_SURFACE ( 'NONE', #14050, 55.69429210806286079, 1.269872874662818729 ) ;
#20313 = B_SPLINE_SURFACE_WITH_KNOTS ( 'NONE', 3, 1, ( 
 ( #28519, #1248 ),
 ( #8328, #3552 ),
 ( #13578, #20638 ),
 ( #5704, #18325 ) ),
 .UNSPECIFIED., .F., .F., .F.,
 ( 4, 4 ),
 ( 2, 2 ),
 ( 0.9911194921636460320, 1.000000000000000000 ),
 ( 0.000000000000000000, 1.000000000000000000 ),
 .UNSPECIFIED. ) ;
#20314 = ORIENTED_EDGE ( 'NONE', *, *, #13669, .F. ) ;
#20315 = CARTESIAN_POINT ( 'NONE',  ( -9.728297238921257417, -5.935454207752202116, 107.6607613508313648 ) ) ;
#20316 = EDGE_LOOP ( 'NONE', ( #8219, #9575, #25000, #22334 ) ) ;
#20317 = CARTESIAN_POINT ( 'NONE',  ( -40.73091736380679606, 9.483895492497156354, 38.64930799450052490 ) ) ;
#20318 = DIRECTION ( 'NONE',  ( 1.000000000000000000, 0.000000000000000000, 0.000000000000000000 ) ) ;
#20319 = LINE ( 'NONE', #18505, #19009 ) ;
#20320 = CARTESIAN_POINT ( 'NONE',  ( 45.79384627280941089, 27.07957786121581734, 49.05938063676249072 ) ) ;
#20321 = EDGE_LOOP ( 'NONE', ( #12624, #15461, #22174, #24720 ) ) ;
#20322 = VECTOR ( 'NONE', #8055, 1000.000000000000000 ) ;
#20323 = EDGE_LOOP ( 'NONE', ( #31483, #14204, #225, #22090, #4055 ) ) ;
#20324 = CARTESIAN_POINT ( 'NONE',  ( 21.09785597605720753, 14.86454579224779948, 47.04930799450052348 ) ) ;
#20325 = TOROIDAL_SURFACE ( 'NONE', #11954, 12.40141737965287660, 0.1250000000000007772 ) ;
#20326 = ORIENTED_EDGE ( 'NONE', *, *, #18612, .F. ) ;
#20327 = CARTESIAN_POINT ( 'NONE',  ( 48.34748475735720774, 24.70653309617948423, 49.49898713858203791 ) ) ;
#20328 = CARTESIAN_POINT ( 'NONE',  ( 21.09785597605720042, -14.54791319078308653, 47.04930799450051637 ) ) ;
#20329 = CARTESIAN_POINT ( 'NONE',  ( -38.36853489569023168, 7.065850718397949315, 32.14930799450051779 ) ) ;
#20330 = AXIS2_PLACEMENT_3D ( 'NONE', #2540, #18270, #22554 ) ;
#20331 = AXIS2_PLACEMENT_3D ( 'NONE', #30092, #15464, #15145 ) ;
#20332 = CARTESIAN_POINT ( 'NONE',  ( -36.18493864628602807, 8.798967949527998655, 60.44930799450051495 ) ) ;
#20333 = CARTESIAN_POINT ( 'NONE',  ( -24.39879438348332386, 13.78276522714992147, 47.04930799450052348 ) ) ;
#20334 = CONTEXT_DEPENDENT_SHAPE_REPRESENTATION ( #3437, #2238 ) ;
#20335 = ORIENTED_EDGE ( 'NONE', *, *, #17828, .F. ) ;
#20336 = FACE_OUTER_BOUND ( 'NONE', #22716, .T. ) ;
#20337 = DIRECTION ( 'NONE',  ( -0.000000000000000000, -1.000000000000000000, -0.000000000000000000 ) ) ;
#20338 = EDGE_CURVE ( 'NONE', #23854, #3483, #6140, .T. ) ;
#20339 = AXIS2_PLACEMENT_3D ( 'NONE', #14484, #31716, #24478 ) ;
#20340 = LINE ( 'NONE', #3098, #15678 ) ;
#20341 = CARTESIAN_POINT ( 'NONE',  ( 46.00908685603033632, 27.63284706826092929, 44.91496614357595263 ) ) ;
#20342 = ORIENTED_EDGE ( 'NONE', *, *, #13354, .T. ) ;
#20343 = DIRECTION ( 'NONE',  ( 0.000000000000000000, -0.000000000000000000, -1.000000000000000000 ) ) ;
#20344 = DIRECTION ( 'NONE',  ( -0.000000000000000000, -1.000000000000000000, -0.000000000000000000 ) ) ;
#20345 = DIRECTION ( 'NONE',  ( -1.000000000000000000, 0.000000000000000000, 0.000000000000000000 ) ) ;
#20346 = VECTOR ( 'NONE', #8104, 1000.000000000000114 ) ;
#20347 = AXIS2_PLACEMENT_3D ( 'NONE', #21888, #6804, #31436 ) ;
#20348 = AXIS2_PLACEMENT_3D ( 'NONE', #12499, #27746, #7568 ) ;
#20349 = ORIENTED_EDGE ( 'NONE', *, *, #12358, .T. ) ;
#20350 = AXIS2_PLACEMENT_3D ( 'NONE', #21331, #30735, #23493 ) ;
#20351 = AXIS2_PLACEMENT_3D ( 'NONE', #25886, #775, #13424 ) ;
#20352 = ORIENTED_EDGE ( 'NONE', *, *, #5461, .T. ) ;
#20353 = DIRECTION ( 'NONE',  ( -1.000000000000000000, -1.101824276508909764E-16, 0.000000000000000000 ) ) ;
#20354 = CARTESIAN_POINT ( 'NONE',  ( -45.02407702159366920, -5.625351695555422360, 52.97525428799637126 ) ) ;
#20355 = CARTESIAN_POINT ( 'NONE',  ( 48.82187354100420151, 22.88065857334294861, 46.16985335424439540 ) ) ;
#20356 = VECTOR ( 'NONE', #11033, 1000.000000000000000 ) ;
#20357 = ORIENTED_EDGE ( 'NONE', *, *, #18080, .F. ) ;
#20358 = FACE_OUTER_BOUND ( 'NONE', #29159, .T. ) ;
#20359 = CARTESIAN_POINT ( 'NONE',  ( -40.16174044770769314, 7.468546898574135895, 60.54930799450051637 ) ) ;
#20360 = CARTESIAN_POINT ( 'NONE',  ( 44.87087493598345134, 27.35322093266652033, 48.18533415931919706 ) ) ;
#20361 = DIRECTION ( 'NONE',  ( -1.101824276508909887E-16, 1.000000000000000000, -0.000000000000000000 ) ) ;
#20362 = FACE_OUTER_BOUND ( 'NONE', #3573, .T. ) ;
#20363 = FACE_OUTER_BOUND ( 'NONE', #172, .T. ) ;
#20364 = DIRECTION ( 'NONE',  ( -0.000000000000000000, -1.000000000000000000, 0.000000000000000000 ) ) ;
#20365 = CYLINDRICAL_SURFACE ( 'NONE', #28379, 27.49999999999999289 ) ;
#20366 = CARTESIAN_POINT ( 'NONE',  ( 8.823509210239581790, 31.84164230456639544, 47.04930799450051637 ) ) ;
#20367 = LINE ( 'NONE', #15610, #525 ) ;
#20368 = CARTESIAN_POINT ( 'NONE',  ( 21.09785597605719332, 30.56454579224779522, 47.04930799450051637 ) ) ;
#20369 = VERTEX_POINT ( 'NONE', #10909 ) ;
#20370 = ORIENTED_EDGE ( 'NONE', *, *, #26793, .F. ) ;
#20371 = DIRECTION ( 'NONE',  ( -0.000000000000000000, -1.000000000000000000, 0.000000000000000000 ) ) ;
#20372 = VECTOR ( 'NONE', #9837, 1000.000000000000000 ) ;
#20373 = CARTESIAN_POINT ( 'NONE',  ( 21.09992658989238734, 38.56284415653841791, 47.04930799450051637 ) ) ;
#20374 = CARTESIAN_POINT ( 'NONE',  ( 49.59034552300744281, 29.16454579224780019, 47.24294646780535345 ) ) ;
#20375 = AXIS2_PLACEMENT_3D ( 'NONE', #20598, #8291, #742 ) ;
#20376 = AXIS2_PLACEMENT_3D ( 'NONE', #812, #28874, #16384 ) ;
#20377 = EDGE_CURVE ( 'NONE', #663, #25220, #14532, .T. ) ;
#20378 = DIRECTION ( 'NONE',  ( -1.000000000000000000, -1.101824276508909887E-16, 0.000000000000000000 ) ) ;
#20379 = EDGE_CURVE ( 'NONE', #24621, #23072, #26568, .T. ) ;
#20380 = EDGE_CURVE ( 'NONE', #3892, #5653, #5602, .T. ) ;
#20381 = ORIENTED_EDGE ( 'NONE', *, *, #22484, .F. ) ;
#20382 = SHAPE_REPRESENTATION ( 'MAT-060', ( #23901, #31239, #14488, #16551, #29670, #21268, #17077, #7129, #13954, #25476, #11323, #30734 ), #29153 ) ;
#20383 = CARTESIAN_POINT ( 'NONE',  ( 21.09785597605719332, 25.56454579224779877, 47.04930799450051637 ) ) ;
#20384 = CARTESIAN_POINT ( 'NONE',  ( 48.50303063523655567, 22.99884124225578574, 47.12228595530052644 ) ) ;
#20385 = DIRECTION ( 'NONE',  ( -0.000000000000000000, -1.000000000000000000, -9.698999007525318993E-17 ) ) ;
#20386 = ORIENTED_EDGE ( 'NONE', *, *, #18192, .T. ) ;
#20387 = ORIENTED_EDGE ( 'NONE', *, *, #11379, .F. ) ;
#20388 = DIRECTION ( 'NONE',  ( -0.000000000000000000, -1.000000000000000000, 0.000000000000000000 ) ) ;
#20389 = EDGE_CURVE ( 'NONE', #17607, #24037, #11387, .T. ) ;
#20390 = CARTESIAN_POINT ( 'NONE',  ( 48.18662509608405031, 27.28284706826093142, 49.18364984542562013 ) ) ;
#20391 = CARTESIAN_POINT ( 'NONE',  ( 45.79384627280941089, 28.47957786121581591, 49.05938063676249072 ) ) ;
#20392 = VECTOR ( 'NONE', #29190, 1000.000000000000227 ) ;
#20393 = DIRECTION ( 'NONE',  ( 0.9986540920324801229, 6.158269594508761132E-17, 0.05186525298099653458 ) ) ;
#20394 = DIRECTION ( 'NONE',  ( -1.000000000000000000, 0.000000000000000000, 0.000000000000000000 ) ) ;
#20395 = EDGE_LOOP ( 'NONE', ( #2237, #23250, #13201, #22083, #11427, #31301 ) ) ;
#20396 = DIRECTION ( 'NONE',  ( 1.234978253042719660E-16, -1.000000000000000000, -1.109335647967047851E-31 ) ) ;
#20397 = AXIS2_PLACEMENT_3D ( 'NONE', #6648, #6972, #29292 ) ;
#20398 = TOROIDAL_SURFACE ( 'NONE', #22502, 12.61792373059897088, 0.1249999999999973216 ) ;
#20399 = ORIENTED_EDGE ( 'NONE', *, *, #15814, .F. ) ;
#20400 = CYLINDRICAL_SURFACE ( 'NONE', #746, 19.99999999999999645 ) ;
#20401 = LINE ( 'NONE', #30434, #30828 ) ;
#20402 = ADVANCED_FACE ( 'NONE', ( #21060 ), #31412, .T. ) ;
#20403 = EDGE_CURVE ( 'NONE', #6908, #272, #9795, .T. ) ;
#20404 = CIRCLE ( 'NONE', #30916, 0.1000000000000014905 ) ;
#20405 = ORIENTED_EDGE ( 'NONE', *, *, #7721, .F. ) ;
#20406 = VECTOR ( 'NONE', #8922, 1000.000000000000114 ) ;
#20407 = CARTESIAN_POINT ( 'NONE',  ( -40.09211399732166115, 9.667069410243957606, 38.64930799450052490 ) ) ;
#20408 = DIRECTION ( 'NONE',  ( 0.6184495258776510074, -0.3428121700606679423, 0.7071067811865505703 ) ) ;
#20409 = DIRECTION ( 'NONE',  ( -1.000000000000000000, 0.000000000000000000, 0.000000000000000000 ) ) ;
#20410 = CIRCLE ( 'NONE', #1039, 12.62506659569710266 ) ;
#20411 = DIRECTION ( 'NONE',  ( -1.101824276508909887E-16, 1.000000000000000000, -0.000000000000000000 ) ) ;
#20412 = CARTESIAN_POINT ( 'NONE',  ( 21.09785597605720042, -14.04221034894631615, 47.04930799450051637 ) ) ;
#20413 = ORIENTED_EDGE ( 'NONE', *, *, #10127, .F. ) ;
#20414 = AXIS2_PLACEMENT_3D ( 'NONE', #5987, #8920, #3674 ) ;
#20415 = LINE ( 'NONE', #12895, #20219 ) ;
#20416 = CARTESIAN_POINT ( 'NONE',  ( 48.37020515026796375, 24.86454579224779593, 49.54352682589573220 ) ) ;
#20417 = CARTESIAN_POINT ( 'NONE',  ( 21.09992658989239089, 27.96664230456639899, 47.04930799450051637 ) ) ;
#20418 = LINE ( 'NONE', #15182, #12463 ) ;
#20419 = CARTESIAN_POINT ( 'NONE',  ( 47.22751897799751220, 26.41988759933319031, 44.55267275764142454 ) ) ;
#20420 = ORIENTED_EDGE ( 'NONE', *, *, #30472, .T. ) ;
#20421 = FACE_OUTER_BOUND ( 'NONE', #7509, .T. ) ;
#20422 = DIRECTION ( 'NONE',  ( 0.2756373558169954996, -0.9612616959383200044, 2.463803012461673974E-31 ) ) ;
#20423 = ORIENTED_EDGE ( 'NONE', *, *, #2408, .T. ) ;
#20424 = DIRECTION ( 'NONE',  ( -0.4848096202463429982, -0.8746197071393925215, -9.920727850371698576E-18 ) ) ;
#20425 = EDGE_CURVE ( 'NONE', #6336, #28788, #32346, .T. ) ;
#20426 = CARTESIAN_POINT ( 'NONE',  ( 21.09785597605719332, 24.86454579224779948, 86.74871914086746472 ) ) ;
#20427 = TOROIDAL_SURFACE ( 'NONE', #24623, 12.40141737965282687, 0.1250000000000004718 ) ;
#20428 = CYLINDRICAL_SURFACE ( 'NONE', #25660, 0.1000000000000006301 ) ;
#20429 = DIRECTION ( 'NONE',  ( 0.5442436726714893203, 6.721291001053903893E-17, -0.8389271868029124501 ) ) ;
#20430 = VERTEX_POINT ( 'NONE', #31892 ) ;
#20431 = CARTESIAN_POINT ( 'NONE',  ( 21.09785597605719332, -5.986312001189870280, 47.04930799450051637 ) ) ;
#20432 = ORIENTED_EDGE ( 'NONE', *, *, #21260, .T. ) ;
#20433 = CIRCLE ( 'NONE', #26215, 12.36707279061065101 ) ;
#20434 = ORIENTED_EDGE ( 'NONE', *, *, #12952, .T. ) ;
#20435 = CIRCLE ( 'NONE', #29364, 12.62506659569710266 ) ;
#20436 = EDGE_CURVE ( 'NONE', #4732, #15249, #16783, .T. ) ;
#20437 = AXIS2_PLACEMENT_3D ( 'NONE', #31324, #1123, #21130 ) ;
#20438 = CIRCLE ( 'NONE', #14147, 1.899999999999999023 ) ;
#20439 = ADVANCED_FACE ( 'NONE', ( #26961 ), #2016, .F. ) ;
#20440 = CARTESIAN_POINT ( 'NONE',  ( 51.99049785380602628, -5.936920032134866076, -13.40664378015324232 ) ) ;
#20441 = CARTESIAN_POINT ( 'NONE',  ( -9.728297238921257417, -5.935454207752202116, 107.6607613508313648 ) ) ;
#20442 = CARTESIAN_POINT ( 'NONE',  ( 81.46980107077142463, -5.937394852768786535, 15.98100540722295015 ) ) ;
#20443 = EDGE_CURVE ( 'NONE', #14267, #1229, #8230, .T. ) ;
#20444 = TOROIDAL_SURFACE ( 'NONE', #28842, 12.40141737965280733, 0.1250000000000013878 ) ;
#20445 = EDGE_CURVE ( 'NONE', #3912, #30065, #888, .T. ) ;
#20446 = EDGE_LOOP ( 'NONE', ( #17811, #14025, #10670, #21072 ) ) ;
#20447 = VERTEX_POINT ( 'NONE', #16461 ) ;
#20448 = EDGE_CURVE ( 'NONE', #14608, #29845, #16593, .T. ) ;
#20449 = CARTESIAN_POINT ( 'NONE',  ( 21.09785597605719687, 24.56454579224780232, 7.349896848133565364 ) ) ;
#20450 = CARTESIAN_POINT ( 'NONE',  ( -35.75861581459462002, -4.595165398174183125, 80.20204475166471525 ) ) ;
#20451 = CARTESIAN_POINT ( 'NONE',  ( -40.60722745863126448, 9.415333058485023443, 35.49072935073782986 ) ) ;
#20452 = ORIENTED_EDGE ( 'NONE', *, *, #23084, .F. ) ;
#20453 = DIRECTION ( 'NONE',  ( 0.4544104193609903586, 0.000000000000000000, 0.8907924397839087627 ) ) ;
#20454 = DIRECTION ( 'NONE',  ( -1.000000000000000000, -1.101824276508910010E-16, 0.000000000000000000 ) ) ;
#20455 = CARTESIAN_POINT ( 'NONE',  ( 33.50134396954523908, 27.34164230456639544, 47.04930799450051637 ) ) ;
#20456 = DIRECTION ( 'NONE',  ( -1.101824276508909887E-16, 1.000000000000000000, -0.000000000000000000 ) ) ;
#20457 = ORIENTED_EDGE ( 'NONE', *, *, #8060, .T. ) ;
#20458 = DIRECTION ( 'NONE',  ( 0.000000000000000000, 0.000000000000000000, -1.000000000000000000 ) ) ;
#20459 = CIRCLE ( 'NONE', #26736, 0.1250000000000001110 ) ;
#20460 = AXIS2_PLACEMENT_3D ( 'NONE', #10121, #24435, #22744 ) ;
#20461 = CARTESIAN_POINT ( 'NONE',  ( 48.34748475735720064, 25.57255849996392172, 49.49898713858203791 ) ) ;
#20462 = CARTESIAN_POINT ( 'NONE',  ( -43.64073206722599707, 1.267352857069779848, 39.54930799450052348 ) ) ;
#20463 = DIRECTION ( 'NONE',  ( -1.000000000000000000, -1.101824276508909887E-16, 0.000000000000000000 ) ) ;
#20464 = CARTESIAN_POINT ( 'NONE',  ( 46.00908685603034343, 25.44624452788248448, 44.91496614357595263 ) ) ;
#20465 = AXIS2_PLACEMENT_3D ( 'NONE', #5252, #15261, #12812 ) ;
#20466 = DIRECTION ( 'NONE',  ( 0.8746197071393925215, -0.4848096202463429982, -8.676864087101708112E-18 ) ) ;
#20467 = DIRECTION ( 'NONE',  ( 0.000000000000000000, -0.000000000000000000, -1.000000000000000000 ) ) ;
#20468 = ORIENTED_EDGE ( 'NONE', *, *, #32028, .F. ) ;
#20469 = CIRCLE ( 'NONE', #22020, 36.01080762834750715 ) ;
#20470 = EDGE_CURVE ( 'NONE', #25220, #19861, #9246, .T. ) ;
#20471 = CARTESIAN_POINT ( 'NONE',  ( 21.09785597605719332, 7.237299147902269247, 66.50898490448155087 ) ) ;
#20472 = EDGE_LOOP ( 'NONE', ( #18193, #26129, #28963 ) ) ;
#20473 =( GEOMETRIC_REPRESENTATION_CONTEXT ( 3 ) GLOBAL_UNCERTAINTY_ASSIGNED_CONTEXT ( ( #9132 ) ) GLOBAL_UNIT_ASSIGNED_CONTEXT ( ( #26678, #31612, #24374 ) ) REPRESENTATION_CONTEXT ( 'NONE', 'WORKASPACE' ) );
#20474 = CARTESIAN_POINT ( 'NONE',  ( 45.96182992765472619, 27.30087065737811969, 44.82232689504102296 ) ) ;
#20475 = ORIENTED_EDGE ( 'NONE', *, *, #32056, .T. ) ;
#20476 = ORIENTED_EDGE ( 'NONE', *, *, #224, .F. ) ;
#20477 = DIRECTION ( 'NONE',  ( -1.000000000000000000, -1.101824276508909887E-16, 0.000000000000000000 ) ) ;
#20478 = AXIS2_PLACEMENT_3D ( 'NONE', #25310, #12846, #510 ) ;
#20479 = ORIENTED_EDGE ( 'NONE', *, *, #23207, .T. ) ;
#20480 = EDGE_CURVE ( 'NONE', #21385, #27343, #28165, .T. ) ;
#20481 = CIRCLE ( 'NONE', #28883, 12.36707279061065279 ) ;
#20482 = EDGE_CURVE ( 'NONE', #14283, #112, #23457, .T. ) ;
#20483 = CIRCLE ( 'NONE', #16280, 31.50000000000000000 ) ;
#20484 = VERTEX_POINT ( 'NONE', #26637 ) ;
#20485 = VECTOR ( 'NONE', #3123, 1000.000000000000000 ) ;
#20486 = CARTESIAN_POINT ( 'NONE',  ( -4.902144023942810236, 24.86454579224779948, 49.54930799450078638 ) ) ;
#20487 = TOROIDAL_SURFACE ( 'NONE', #15788, 1.299999999999999822, 0.1000000000000000056 ) ;
#20488 = ADVANCED_FACE ( 'NONE', ( #24668 ), #31838, .F. ) ;
#20489 = EDGE_LOOP ( 'NONE', ( #8374, #5866, #5336, #30405 ) ) ;
#20490 = EDGE_CURVE ( 'NONE', #1152, #23296, #32318, .T. ) ;
#20491 = CARTESIAN_POINT ( 'NONE',  ( 46.33059210211230550, 22.93807716476589675, 45.54522087609679204 ) ) ;
#20492 = DIRECTION ( 'NONE',  ( -1.224646799147353207E-16, -1.349345573449484691E-32, 1.000000000000000000 ) ) ;
#20493 = CARTESIAN_POINT ( 'NONE',  ( 47.09785597605719687, 29.86454579224779948, 47.04930799450078638 ) ) ;
#20494 = CARTESIAN_POINT ( 'NONE',  ( 46.99218062947583974, 28.55956182964376211, 49.08406571254116102 ) ) ;
#20495 = VERTEX_POINT ( 'NONE', #7603 ) ;
#20496 = ORIENTED_EDGE ( 'NONE', *, *, #30948, .F. ) ;
#20497 = CARTESIAN_POINT ( 'NONE',  ( -40.48129536610376533, 8.613360132207176889, 39.54930799450052348 ) ) ;
#20498 = AXIS2_PLACEMENT_3D ( 'NONE', #25468, #19884, #30564 ) ;
#20499 = ORIENTED_EDGE ( 'NONE', *, *, #29698, .F. ) ;
#20500 = DIRECTION ( 'NONE',  ( 0.000000000000000000, 0.000000000000000000, -1.000000000000000000 ) ) ;
#20501 = CARTESIAN_POINT ( 'NONE',  ( 8.482002859293416464, 25.96664230456639899, 47.04930799450051637 ) ) ;
#20502 = DIRECTION ( 'NONE',  ( -1.000000000000000000, 0.000000000000000000, 0.000000000000000000 ) ) ;
#20503 = CARTESIAN_POINT ( 'NONE',  ( -41.13156850465621517, 9.429949956619452678, 38.44930799450052916 ) ) ;
#20504 = CARTESIAN_POINT ( 'NONE',  ( -40.11286833322908052, 2.887657226147511302, 57.04930799450051637 ) ) ;
#20505 = ORIENTED_EDGE ( 'NONE', *, *, #16843, .T. ) ;
#20506 = CYLINDRICAL_SURFACE ( 'NONE', #18685, 2.500000000000002220 ) ;
#20507 = CARTESIAN_POINT ( 'NONE',  ( -42.47434154250543514, 4.196643200812633978, 37.04930799450052348 ) ) ;
#20508 = DIRECTION ( 'NONE',  ( -0.000000000000000000, -1.000000000000000000, 0.000000000000000000 ) ) ;
#20509 = LINE ( 'NONE', #6068, #20322 ) ;
#20510 = AXIS2_PLACEMENT_3D ( 'NONE', #5178, #7801, #7148 ) ;
#20511 = VERTEX_POINT ( 'NONE', #17764 ) ;
#20512 = CARTESIAN_POINT ( 'NONE',  ( 8.474859994195286461, 25.84143805560860940, 47.04930799450051637 ) ) ;
#20513 = VECTOR ( 'NONE', #28458, 1000.000000000000000 ) ;
#20514 = DIRECTION ( 'NONE',  ( -0.2756373558169973870, 0.9612616959383193382, 1.315048337272770435E-17 ) ) ;
#20515 = CIRCLE ( 'NONE', #20437, 0.7928932188134575343 ) ;
#20516 = CARTESIAN_POINT ( 'NONE',  ( 21.09785597605720753, 14.86454579224779948, 47.04930799450052348 ) ) ;
#20517 = ORIENTED_EDGE ( 'NONE', *, *, #31083, .T. ) ;
#20518 = AXIS2_PLACEMENT_3D ( 'NONE', #6492, #26347, #16817 ) ;
#20519 = AXIS2_PLACEMENT_3D ( 'NONE', #7017, #27192, #7344 ) ;
#20520 = VERTEX_POINT ( 'NONE', #22520 ) ;
#20521 = ORIENTED_EDGE ( 'NONE', *, *, #15481, .F. ) ;
#20522 = CARTESIAN_POINT ( 'NONE',  ( 21.09992658989239089, 27.34164230456639544, 47.04930799450051637 ) ) ;
#20523 = CARTESIAN_POINT ( 'NONE',  ( 21.09785597605720753, 17.16474120167318418, 47.04930799450052348 ) ) ;
#20524 = LINE ( 'NONE', #5762, #28832 ) ;
#20525 = EDGE_CURVE ( 'NONE', #28530, #6416, #22849, .T. ) ;
#20526 = ORIENTED_EDGE ( 'NONE', *, *, #27389, .T. ) ;
#20527 = CIRCLE ( 'NONE', #23153, 3.699999999999994849 ) ;
#20528 = EDGE_CURVE ( 'NONE', #23463, #21709, #23954, .T. ) ;
#20529 = EDGE_CURVE ( 'NONE', #19824, #5228, #8771, .T. ) ;
#20530 = DIRECTION ( 'NONE',  ( -6.722685822323786766E-17, 1.000000000000000000, -0.000000000000000000 ) ) ;
#20531 = AXIS2_PLACEMENT_3D ( 'NONE', #12706, #32229, #14993 ) ;
#20532 = PLANE ( 'NONE',  #26985 ) ;
#20533 = DIRECTION ( 'NONE',  ( 0.000000000000000000, 0.000000000000000000, -1.000000000000000000 ) ) ;
#20534 = DIRECTION ( 'NONE',  ( -0.9612616959383207815, -0.2756373558169926685, -8.795445018804289444E-19 ) ) ;
#20535 = DIRECTION ( 'NONE',  ( 0.000000000000000000, -0.000000000000000000, -1.000000000000000000 ) ) ;
#20536 = DIRECTION ( 'NONE',  ( -1.101824276508909887E-16, 1.000000000000000000, -0.000000000000000000 ) ) ;
#20537 = DIRECTION ( 'NONE',  ( -0.000000000000000000, 1.000000000000000000, 0.000000000000000000 ) ) ;
#20538 = CARTESIAN_POINT ( 'NONE',  ( -40.49096175631598271, 7.521145078229855230, 53.94930799450052206 ) ) ;
#20539 = DIRECTION ( 'NONE',  ( 2.946248497964555786E-19, 3.001156285468303092E-19, 1.000000000000000000 ) ) ;
#20540 = CARTESIAN_POINT ( 'NONE',  ( 42.05836384037805686, 11.91446173404583853, 98.83287304499684467 ) ) ;
#20541 = DIRECTION ( 'NONE',  ( 0.2530443915477140204, -0.8824706660164525207, 0.3965022818682459316 ) ) ;
#20542 = ORIENTED_EDGE ( 'NONE', *, *, #1777, .F. ) ;
#20543 = EDGE_LOOP ( 'NONE', ( #18151, #10124, #31556, #19440 ) ) ;
#20544 = CARTESIAN_POINT ( 'NONE',  ( 21.09785597605719687, 44.99492099041257376, 69.69066552443730700 ) ) ;
#20545 = CIRCLE ( 'NONE', #12719, 0.09999999999999795164 ) ;
#20546 = CARTESIAN_POINT ( 'NONE',  ( 47.98183884068953375, 25.10658484134872381, 44.68358619858262415 ) ) ;
#20547 = FACE_OUTER_BOUND ( 'NONE', #2379, .T. ) ;
#20548 = ORIENTED_EDGE ( 'NONE', *, *, #2984, .T. ) ;
#20549 = CARTESIAN_POINT ( 'NONE',  ( 21.09785597605720753, 13.66454579224780019, 47.04930799450052348 ) ) ;
#20550 = CARTESIAN_POINT ( 'NONE',  ( 21.09785597605719332, 7.881678200673685630, 47.04930799450051637 ) ) ;
#20551 = CARTESIAN_POINT ( 'NONE',  ( 21.09992658989239089, 26.59164230456639899, 47.04930799450051637 ) ) ;
#20552 = ORIENTED_EDGE ( 'NONE', *, *, #16438, .T. ) ;
#20553 = EDGE_LOOP ( 'NONE', ( #24152, #18495, #27845, #16007 ) ) ;
#20554 = CARTESIAN_POINT ( 'NONE',  ( 46.99023568444673060, 25.82451373492760283, 49.12151524109405898 ) ) ;
#20555 = CARTESIAN_POINT ( 'NONE',  ( 45.35708200440645044, 29.70457786121581378, 45.92000246470679770 ) ) ;
#20556 = CIRCLE ( 'NONE', #12174, 2.500000000000002220 ) ;
#20557 = CARTESIAN_POINT ( 'NONE',  ( -39.40147288705622941, -5.935926662576402890, 77.96005242632439547 ) ) ;
#20558 = VECTOR ( 'NONE', #16385, 1000.000000000000000 ) ;
#20559 = ORIENTED_EDGE ( 'NONE', *, *, #122, .F. ) ;
#20560 = CARTESIAN_POINT ( 'NONE',  ( 21.09785597605719332, 11.92558985988973852, 47.04930799450051637 ) ) ;
#20561 = DIRECTION ( 'NONE',  ( -1.000000000000000000, 0.000000000000000000, 0.000000000000000000 ) ) ;
#20562 = ADVANCED_FACE ( 'NONE', ( #524 ), #20308, .F. ) ;
#20563 = VERTEX_POINT ( 'NONE', #17272 ) ;
#20564 = EDGE_CURVE ( 'NONE', #11017, #7677, #21340, .T. ) ;
#20565 = EDGE_CURVE ( 'NONE', #9081, #2041, #2506, .T. ) ;
#20566 = AXIS2_PLACEMENT_3D ( 'NONE', #23328, #10707, #25625 ) ;
#20567 = EDGE_CURVE ( 'NONE', #6740, #18076, #27294, .T. ) ;
#20568 = EDGE_CURVE ( 'NONE', #27923, #104, #30787, .T. ) ;
#20569 = CARTESIAN_POINT ( 'NONE',  ( 48.23388202445966044, 26.95087065737812182, 49.27628909396054979 ) ) ;
#20571 = CARTESIAN_POINT ( 'NONE',  ( 44.99489604499470374, 22.84434098701873594, 46.61610178023796891 ) ) ;
#20570 = CIRCLE ( 'NONE', #18485, 55.85791022362053582 ) ;
#20572 = EDGE_CURVE ( 'NONE', #3738, #7332, #30413, .T. ) ;
#20573 = AXIS2_PLACEMENT_3D ( 'NONE', #17345, #2574, #27364 ) ;
#20574 = ORIENTED_EDGE ( 'NONE', *, *, #30218, .T. ) ;
#20575 = DIRECTION ( 'NONE',  ( 0.3428121700606595046, 0.6184495258776487869, 0.7071067811865566766 ) ) ;
#20576 = DIRECTION ( 'NONE',  ( -1.000000000000000000, 0.000000000000000000, 0.000000000000000000 ) ) ;
#20577 = TOROIDAL_SURFACE ( 'NONE', #29517, 38.50000000000000000, 0.9999999999999974465 ) ;
#20578 =( BOUNDED_CURVE ( )  B_SPLINE_CURVE ( 2, ( #7964, #15978, #25985, #3497, #13525, #4593, #9076, #11375, #12320, #26474, #24782, #19850, #11220, #22147, #22317, #32180, #16609, #24003, #18909, #24618, #23842, #14783, #1358, #14616, #2300, #32341, #6456, #16455, #3664, #7224, #2138, #13690, #9851, #6290, #9692, #14007, #21365, #21208, #31248, #29101, #19686, #29881, #13845, #12156, #28773, #8911, #7397, #26313, #17393, #8749, #23691, #1193, #1519, #31406, #19069, #17224, #29714, #16295, #11540, #27238, #26630, #18743, #3826, #31570, #28943, #3986, #4766, #21532, #6616, #4928, #10678, #30533, #10182, #28064, #27735, #5253, #5576, #15262, #15574, #15422, #20017 ),
 .UNSPECIFIED., .F., .F. ) 
 B_SPLINE_CURVE_WITH_KNOTS ( ( 3, 2, 2, 2, 2, 2, 2, 2, 2, 2, 2, 2, 2, 2, 2, 2, 2, 2, 2, 2, 2, 2, 2, 2, 2, 2, 2, 2, 2, 2, 2, 2, 2, 2, 2, 2, 2, 2, 2, 2, 3 ),
 ( 0.04723643264279250159, 0.04761904761904761640, 0.07142857142857142461, 0.09523809523809523281, 0.1190476190476190410, 0.1428571428571428492, 0.1666666666666666574, 0.1904761904761904656, 0.2142857142857142738, 0.2380952380952381098, 0.2619047619047619180, 0.2857142857142856984, 0.3095238095238095344, 0.3333333333333333148, 0.3571428571428571508, 0.3809523809523809312, 0.4047619047619047672, 0.4285714285714285476, 0.4523809523809523836, 0.4761904761904762196, 0.5000000000000000000, 0.5238095238095238360, 0.5476190476190476719, 0.5714285714285713969, 0.5952380952380951218, 0.6190476190476190688, 0.6428571428571429047, 0.6666666666666666297, 0.6904761904761904656, 0.7142857142857143016, 0.7380952380952381375, 0.7619047619047618625, 0.7857142857142856984, 0.8095238095238095344, 0.8333333333333333703, 0.8571428571428570953, 0.8809523809523809312, 0.9047619047619047672, 0.9285714285714286031, 0.9523809523809523281, 0.9642857142857166330 ),
 .UNSPECIFIED. ) 
 CURVE ( )  GEOMETRIC_REPRESENTATION_ITEM ( )  RATIONAL_B_SPLINE_CURVE ( ( 0.9957632973360193152, 0.9978470511481081218, 1.000000000000000000, 0.8660254037844387076, 1.000000000000000000, 0.8660254037844387076, 1.000000000000000000, 0.8660254037844387076, 1.000000000000000000, 0.8660254037844387076, 1.000000000000000000, 0.8660254037844387076, 1.000000000000000000, 0.8660254037844387076, 1.000000000000000000, 0.8660254037844387076, 1.000000000000000000, 0.8660254037844387076, 1.000000000000000000, 0.8660254037844387076, 1.000000000000000000, 0.8660254037844387076, 1.000000000000000000, 0.8660254037844387076, 1.000000000000000000, 0.8660254037844387076, 1.000000000000000000, 0.8660254037844387076, 1.000000000000000000, 0.8660254037844387076, 1.000000000000000000, 0.8660254037844387076, 1.000000000000000000, 0.8660254037844387076, 1.000000000000000000, 0.8660254037844387076, 1.000000000000000000, 0.8660254037844387076, 1.000000000000000000, 0.8660254037844387076, 1.000000000000000000, 0.8660254037844387076, 1.000000000000000000, 0.8660254037844387076, 1.000000000000000000, 0.8660254037844387076, 1.000000000000000000, 0.8660254037844387076, 1.000000000000000000, 0.8660254037844387076, 1.000000000000000000, 0.8660254037844387076, 1.000000000000000000, 0.8660254037844387076, 1.000000000000000000, 0.8660254037844387076, 1.000000000000000000, 0.8660254037844387076, 1.000000000000000000, 0.8660254037844387076, 1.000000000000000000, 0.8660254037844387076, 1.000000000000000000, 0.8660254037844387076, 1.000000000000000000, 0.8660254037844387076, 1.000000000000000000, 0.8660254037844387076, 1.000000000000000000, 0.8660254037844387076, 1.000000000000000000, 0.8660254037844387076, 1.000000000000000000, 0.8660254037844387076, 1.000000000000000000, 0.8660254037844387076, 1.000000000000000000, 0.8660254037844387076, 1.000000000000000000, 0.9330127018922058646, 0.9330127018922192983 ) ) 
 REPRESENTATION_ITEM ( '' )  );
#20579 = LINE ( 'NONE', #3169, #32041 ) ;
#20580 = DIRECTION ( 'NONE',  ( -1.000000000000000000, 0.000000000000000000, 0.000000000000000000 ) ) ;
#20581 = VERTEX_POINT ( 'NONE', #363 ) ;
#20582 = DIRECTION ( 'NONE',  ( 0.4848096202463424986, 0.8746197071393928546, -2.220446049250312834E-16 ) ) ;
#20583 = CARTESIAN_POINT ( 'NONE',  ( 8.482002859293801933, 31.46664230456641675, 47.04930799450051637 ) ) ;
#20584 = CARTESIAN_POINT ( 'NONE',  ( -38.41701585771487260, 6.978388747684010518, 62.04930799450052348 ) ) ;
#20585 = DIRECTION ( 'NONE',  ( -0.2756373558169973870, 0.9612616959383193382, 1.315048337272770280E-17 ) ) ;
#20586 = CARTESIAN_POINT ( 'NONE',  ( -40.50410981870283678, 7.604537000166497585, 38.76008276981544753 ) ) ;
#20587 = VERTEX_POINT ( 'NONE', #29932 ) ;
#20588 = DIRECTION ( 'NONE',  ( -0.000000000000000000, -0.000000000000000000, 1.000000000000000000 ) ) ;
#20589 = FACE_OUTER_BOUND ( 'NONE', #30887, .T. ) ;
#20590 = FACE_OUTER_BOUND ( 'NONE', #26820, .T. ) ;
#20591 = ORIENTED_EDGE ( 'NONE', *, *, #298, .T. ) ;
#20592 = LINE ( 'NONE', #15348, #3116 ) ;
#20593 = PLANE ( 'NONE',  #9392 ) ;
#20594 = DIRECTION ( 'NONE',  ( 0.000000000000000000, 0.000000000000000000, 1.000000000000000000 ) ) ;
#20595 = CARTESIAN_POINT ( 'NONE',  ( 21.09785597605720042, -16.73545420775220194, -31.45069200549948363 ) ) ;
#20596 = TOROIDAL_SURFACE ( 'NONE', #6441, 17.50000000000000000, 1.999999999999998224 ) ;
#20597 = ORIENTED_EDGE ( 'NONE', *, *, #13398, .T. ) ;
#20598 = CARTESIAN_POINT ( 'NONE',  ( 67.49616587369396825, 13.78442380691147839, 47.04930799450051637 ) ) ;
#20599 = ORIENTED_EDGE ( 'NONE', *, *, #4418, .T. ) ;
#20600 = CIRCLE ( 'NONE', #8056, 0.5000000000000004441 ) ;
#20601 = ADVANCED_FACE ( 'NONE', ( #2674 ), #15077, .F. ) ;
#20602 = ORIENTED_EDGE ( 'NONE', *, *, #8665, .F. ) ;
#20603 = AXIS2_PLACEMENT_3D ( 'NONE', #23860, #26813, #26327 ) ;
#20604 = CIRCLE ( 'NONE', #6452, 0.1250000000000001110 ) ;
#20605 = ADVANCED_FACE ( 'NONE', ( #12705 ), #904, .F. ) ;
#20606 = CARTESIAN_POINT ( 'NONE',  ( 47.22751897799751220, 27.81988759933318889, 44.55267275764142454 ) ) ;
#20607 = LINE ( 'NONE', #22905, #25717 ) ;
#20608 = DIRECTION ( 'NONE',  ( -1.101824276508909887E-16, 1.000000000000000000, -0.000000000000000000 ) ) ;
#20609 = EDGE_CURVE ( 'NONE', #2889, #16322, #20827, .T. ) ;
#20610 = ORIENTED_EDGE ( 'NONE', *, *, #31312, .F. ) ;
#20611 = FACE_OUTER_BOUND ( 'NONE', #12717, .T. ) ;
#20612 = ORIENTED_EDGE ( 'NONE', *, *, #15263, .T. ) ;
#20613 = AXIS2_PLACEMENT_3D ( 'NONE', #13263, #13418, #8005 ) ;
#20614 = CARTESIAN_POINT ( 'NONE',  ( 45.97377588299919893, 23.04411619146718238, 46.99092872297675427 ) ) ;
#20615 = DIRECTION ( 'NONE',  ( -0.000000000000000000, -1.000000000000000000, 0.000000000000000000 ) ) ;
#20616 = CARTESIAN_POINT ( 'NONE',  ( -31.54987825820634839, 11.92645443048831488, 67.99310208698472024 ) ) ;
#20617 = TOROIDAL_SURFACE ( 'NONE', #2279, 26.49999999999999645, 0.9999999999999956701 ) ;
#20618 = DIRECTION ( 'NONE',  ( -1.000000000000000000, 0.000000000000000000, 0.000000000000000000 ) ) ;
#20619 = VERTEX_POINT ( 'NONE', #13014 ) ;
#20620 = DIRECTION ( 'NONE',  ( -1.101824276508909887E-16, 1.000000000000000000, -0.000000000000000000 ) ) ;
#20621 = ORIENTED_EDGE ( 'NONE', *, *, #18043, .T. ) ;
#20622 = DIRECTION ( 'NONE',  ( 1.177206059073821606E-16, -0.2756373558169902815, 0.9612616959383214477 ) ) ;
#20623 = CARTESIAN_POINT ( 'NONE',  ( 8.698509210239576461, 31.34164230456639544, 47.04930799450051637 ) ) ;
#20624 = EDGE_LOOP ( 'NONE', ( #25714, #16826, #23209, #13747 ) ) ;
#20625 = CARTESIAN_POINT ( 'NONE',  ( 47.25101359556892078, 23.12036939723557083, 46.81322240026007364 ) ) ;
#20626 = CARTESIAN_POINT ( 'NONE',  ( 81.58903466081247302, -5.935454061169748385, 15.93786273650362872 ) ) ;
#20627 = CARTESIAN_POINT ( 'NONE',  ( 8.482002859293396924, 24.21664230456639899, 47.04930799450051637 ) ) ;
#20628 = DIRECTION ( 'NONE',  ( -1.000000000000000000, -1.101824276508909887E-16, 0.000000000000000000 ) ) ;
#20629 = CIRCLE ( 'NONE', #14876, 45.93251711706293605 ) ;
#20630 = CARTESIAN_POINT ( 'NONE',  ( -18.90214402394280313, 14.86454579224779948, 47.04930799450052348 ) ) ;
#20631 = AXIS2_PLACEMENT_3D ( 'NONE', #18886, #26290, #13824 ) ;
#20632 = AXIS2_PLACEMENT_3D ( 'NONE', #7685, #32467, #2908 ) ;
#20633 = DIRECTION ( 'NONE',  ( -1.101824276508909887E-16, 1.000000000000000000, -0.000000000000000000 ) ) ;
#20634 = CARTESIAN_POINT ( 'NONE',  ( -40.68293647075807229, 6.808040729367104582, 34.57337564942579178 ) ) ;
#20635 = ORIENTED_EDGE ( 'NONE', *, *, #10278, .F. ) ;
#20636 = CARTESIAN_POINT ( 'NONE',  ( 21.09785597605720042, -16.03545420775220265, 47.04930799450051637 ) ) ;
#20637 = EDGE_CURVE ( 'NONE', #29330, #1073, #18717, .T. ) ;
#20638 = CARTESIAN_POINT ( 'NONE',  ( -9.925114359954182675, -5.937449718911893548, -13.32263710021335612 ) ) ;
#20639 = ORIENTED_EDGE ( 'NONE', *, *, #8407, .F. ) ;
#20640 = ORIENTED_EDGE ( 'NONE', *, *, #31304, .T. ) ;
#20641 = CARTESIAN_POINT ( 'NONE',  ( -42.26497471389478733, 14.66834543456875117, 55.08207028713757580 ) ) ;
#20642 = EDGE_CURVE ( 'NONE', #15058, #19572, #22933, .T. ) ;
#20643 = UNCERTAINTY_MEASURE_WITH_UNIT (LENGTH_MEASURE( 1.000000000000000082E-05 ), #5776, 'distance_accuracy_value', 'NONE');
#20644 = ADVANCED_FACE ( 'NONE', ( #19898 ), #6156, .T. ) ;
#20645 = VERTEX_POINT ( 'NONE', #15947 ) ;
#20646 = CIRCLE ( 'NONE', #13828, 12.62506659569710266 ) ;
#20647 = CIRCLE ( 'NONE', #14887, 0.09999999999999836797 ) ;
#20648 = ORIENTED_EDGE ( 'NONE', *, *, #29691, .F. ) ;
#20649 = DIRECTION ( 'NONE',  ( -0.000000000000000000, -1.000000000000000000, 0.000000000000000000 ) ) ;
#20650 = EDGE_CURVE ( 'NONE', #13584, #2858, #21022, .T. ) ;
#20651 = VERTEX_POINT ( 'NONE', #5949 ) ;
#20652 = CARTESIAN_POINT ( 'NONE',  ( 48.73394074504988538, 22.89977464660286444, 47.94256374451057212 ) ) ;
#20653 = CARTESIAN_POINT ( 'NONE',  ( 21.09785597605718621, -13.49020584019834601, -11.04286022428629188 ) ) ;
#20654 = CARTESIAN_POINT ( 'NONE',  ( 21.09785597605719687, 47.56454579224779877, 28.18735555590595609 ) ) ;
#20655 = CARTESIAN_POINT ( 'NONE',  ( 46.02876340639226527, 26.86789516297709568, 44.95353858666495483 ) ) ;
#20656 = ORIENTED_EDGE ( 'NONE', *, *, #9216, .T. ) ;
#20657 = EDGE_LOOP ( 'NONE', ( #11270, #9482, #30639, #29511 ) ) ;
#20658 = VERTEX_POINT ( 'NONE', #8566 ) ;
#20659 = DIRECTION ( 'NONE',  ( -0.8746197071393895239, 0.4848096202463481053, 0.000000000000000000 ) ) ;
#20660 = DIRECTION ( 'NONE',  ( -0.9612616959383200044, -0.2756373558169956106, -8.795445018804684260E-19 ) ) ;
#20661 = DIRECTION ( 'NONE',  ( 0.8389271868029106738, 0.000000000000000000, 0.5442436726714922068 ) ) ;
#20662 = AXIS2_PLACEMENT_3D ( 'NONE', #21687, #9228, #4302 ) ;
#20663 = CARTESIAN_POINT ( 'NONE',  ( 21.09785597605720397, -16.43545420775217281, 132.0493079945005377 ) ) ;
#20664 = DIRECTION ( 'NONE',  ( -1.000000000000000000, 0.000000000000000000, 0.000000000000000000 ) ) ;
#20665 = EDGE_CURVE ( 'NONE', #5065, #25423, #28698, .T. ) ;
#20666 = AXIS2_PLACEMENT_3D ( 'NONE', #10783, #20775, #17660 ) ;
#20667 = EDGE_LOOP ( 'NONE', ( #25531, #9516, #8715, #15515 ) ) ;
#20668 = DIRECTION ( 'NONE',  ( -1.000000000000000000, 0.000000000000000000, 0.000000000000000000 ) ) ;
#20669 = CARTESIAN_POINT ( 'NONE',  ( 33.71785032049098874, 30.46664230456641675, 47.04930799450051637 ) ) ;
#20670 = EDGE_CURVE ( 'NONE', #1027, #23957, #22388, .T. ) ;
#20671 = AXIS2_PLACEMENT_3D ( 'NONE', #6756, #16754, #22 ) ;
#20672 = CARTESIAN_POINT ( 'NONE',  ( -9.880265915727269643, -5.935454337261168334, 107.5563424404352872 ) ) ;
#20673 = CARTESIAN_POINT ( 'NONE',  ( 48.40186567930497574, 25.41618040159426783, 45.03923535223908203 ) ) ;
#20674 = EDGE_LOOP ( 'NONE', ( #27492, #9645, #17023, #23829 ) ) ;
#20675 = CARTESIAN_POINT ( 'NONE',  ( -41.94956971822180947, 3.905757428664828890, 47.04930799450051637 ) ) ;
#20676 = CARTESIAN_POINT ( 'NONE',  ( 47.09785597605719687, 29.86454579224779948, 47.04930799450078638 ) ) ;
#20677 = B_SPLINE_CURVE_WITH_KNOTS ( 'NONE', 3,
 ( #26285, #1486, #3792, #13817, #1327, #9210, #11348, #19201, #4113, #31541, #3959, #21674, #21335, #9046, #29228, #29066, #28918, #6587, #6742, #16581, #16740, #26767, #31698, #24137, #1655, #32020, #7237, #24628, #29566, #1977, #11998, #32190, #17232, #9542 ),
 .UNSPECIFIED., .F., .F.,
 ( 4, 2, 2, 2, 2, 2, 2, 2, 2, 2, 2, 2, 2, 2, 2, 2, 4 ),
 ( 0.000000000000000000, 0.03124999999999995837, 0.06249999999999994449, 0.09374999999999993061, 0.1249999999999999167, 0.1562499999999998890, 0.1874999999999998890, 0.2187499999999998612, 0.2499999999999998890, 0.2812499999999998890, 0.3124999999999998890, 0.3437499999999999445, 0.3749999999999999445, 0.4062499999999999445, 0.4374999999999999445, 0.4687500000000000000, 0.5000000000000000000 ),
 .UNSPECIFIED. ) ;
#20678 = EDGE_CURVE ( 'NONE', #8602, #26085, #27133, .T. ) ;
#20679 = ADVANCED_FACE ( 'NONE', ( #11192 ), #11035, .F. ) ;
#20680 = ORIENTED_EDGE ( 'NONE', *, *, #4783, .T. ) ;
#20681 = VERTEX_POINT ( 'NONE', #5618 ) ;
#20682 = ORIENTED_EDGE ( 'NONE', *, *, #25696, .T. ) ;
#20683 = FACE_OUTER_BOUND ( 'NONE', #28909, .T. ) ;
#20684 = CARTESIAN_POINT ( 'NONE',  ( -0.9021440239427926944, 14.86454579224779948, 47.04930799450052348 ) ) ;
#20686 = DIRECTION ( 'NONE',  ( -0.000000000000000000, -1.000000000000000000, 0.000000000000000000 ) ) ;
#20685 = CIRCLE ( 'NONE', #12866, 12.62506659569710266 ) ;
#20687 = AXIS2_PLACEMENT_3D ( 'NONE', #22656, #7413, #17567 ) ;
#20688 = AXIS2_PLACEMENT_3D ( 'NONE', #18499, #28371, #23112 ) ;
#20689 = ORIENTED_EDGE ( 'NONE', *, *, #7123, .F. ) ;
#20690 = CARTESIAN_POINT ( 'NONE',  ( 6.626556088358251273, -13.30632128221581389, -6.978462942695593085 ) ) ;
#20691 = CARTESIAN_POINT ( 'NONE',  ( -39.67555847965937943, 2.645252416024337361, 47.04930799450051637 ) ) ;
#20692 = CARTESIAN_POINT ( 'NONE',  ( -39.58809650894544774, 2.596771453999702661, 49.04930799450051637 ) ) ;
#20693 = FACE_OUTER_BOUND ( 'NONE', #10553, .T. ) ;
#20694 = DIRECTION ( 'NONE',  ( -0.2756373558169974980, 0.9612616959383193382, 1.315048337272770589E-17 ) ) ;
#20695 = CARTESIAN_POINT ( 'NONE',  ( -41.88090303775678080, 13.82677487427665497, 60.54930799450051637 ) ) ;
#20696 = CARTESIAN_POINT ( 'NONE',  ( -14.40214402394279780, 14.86454579224779948, 47.04930799450052348 ) ) ;
#20697 = CARTESIAN_POINT ( 'NONE',  ( 21.09992658989239089, 27.09164230456639899, 47.04930799450051637 ) ) ;
#20698 = DIRECTION ( 'NONE',  ( -1.101824276508909887E-16, 1.000000000000000000, -0.000000000000000000 ) ) ;
#20699 = CARTESIAN_POINT ( 'NONE',  ( 42.88478197795839719, 11.83483724345210142, 98.53854327536406288 ) ) ;
#20700 = EDGE_CURVE ( 'NONE', #1803, #10259, #8255, .T. ) ;
#20701 = CARTESIAN_POINT ( 'NONE',  ( -42.38687957179150345, 4.148162238788004608, 55.84930799450052064 ) ) ;
#20702 = SURFACE_SIDE_STYLE ('',( #8714 ) ) ;
#20703 = EDGE_LOOP ( 'NONE', ( #4163, #14300, #25756, #15566 ) ) ;
#20704 = VERTEX_POINT ( 'NONE', #26114 ) ;
#20705 = DIRECTION ( 'NONE',  ( -1.000000000000000000, 0.000000000000000000, 0.000000000000000000 ) ) ;
#20706 = LINE ( 'NONE', #27776, #9870 ) ;
#20707 = ADVANCED_FACE ( 'NONE', ( #8092 ), #3011, .T. ) ;
#20708 = FACE_OUTER_BOUND ( 'NONE', #6854, .T. ) ;
#20709 = AXIS2_PLACEMENT_3D ( 'NONE', #6196, #6682, #6524 ) ;
#20710 = VERTEX_POINT ( 'NONE', #1011 ) ;
#20711 = DIRECTION ( 'NONE',  ( 0.2756373558169926685, -0.9612616959383207815, -1.315048337272770743E-17 ) ) ;
#20712 = CARTESIAN_POINT ( 'NONE',  ( 33.46699938050304013, 25.96183152705960140, 47.04930799450051637 ) ) ;
#20713 = ORIENTED_EDGE ( 'NONE', *, *, #3134, .T. ) ;
#20715 = TOROIDAL_SURFACE ( 'NONE', #6560, 12.61792373059898864, 0.1249999999999962669 ) ;
#20714 = CARTESIAN_POINT ( 'NONE',  ( 33.46699938050304013, 26.72145308207318948, 47.04930799450050927 ) ) ;
#20716 = CARTESIAN_POINT ( 'NONE',  ( 48.83862994770794330, 26.64118040159426570, 48.17861352429476796 ) ) ;
#20717 = AXIS2_PLACEMENT_3D ( 'NONE', #8635, #23724, #11260 ) ;
#20718 = AXIS2_PLACEMENT_3D ( 'NONE', #32418, #9442, #9603 ) ;
#20719 = CARTESIAN_POINT ( 'NONE',  ( 46.00908685603034343, 27.54624452788248590, 44.91496614357595263 ) ) ;
#20720 = EDGE_CURVE ( 'NONE', #28434, #28996, #1164, .T. ) ;
#20721 = CARTESIAN_POINT ( 'NONE',  ( -34.77292974153792215, 11.39147729100211670, 52.68251853679213070 ) ) ;
#20722 = AXIS2_PLACEMENT_3D ( 'NONE', #15016, #10412, #12229 ) ;
#20723 = EDGE_LOOP ( 'NONE', ( #21833, #6471, #14922, #5331 ) ) ;
#20724 = DIRECTION ( 'NONE',  ( -1.101824276508909887E-16, 1.000000000000000000, -0.000000000000000000 ) ) ;
#20725 = DIRECTION ( 'NONE',  ( 8.659560562355194168E-17, 0.7071067811865260344, -0.7071067811865690000 ) ) ;
#20726 = ORIENTED_EDGE ( 'NONE', *, *, #20425, .T. ) ;
#20727 = AXIS2_PLACEMENT_3D ( 'NONE', #6363, #4050, #29168 ) ;
#20728 = DIRECTION ( 'NONE',  ( -0.4848096202463645921, -0.8746197071393805311, 0.000000000000000000 ) ) ;
#20729 = CARTESIAN_POINT ( 'NONE',  ( 47.09785597605719687, 23.12036939723557083, 47.04930799450080059 ) ) ;
#20730 = AXIS2_PLACEMENT_3D ( 'NONE', #14983, #10222, #29754 ) ;
#20731 = LINE ( 'NONE', #2077, #27351 ) ;
#20732 =( GEOMETRIC_REPRESENTATION_CONTEXT ( 3 ) GLOBAL_UNCERTAINTY_ASSIGNED_CONTEXT ( ( #14386 ) ) GLOBAL_UNIT_ASSIGNED_CONTEXT ( ( #27772, #10376, #22350 ) ) REPRESENTATION_CONTEXT ( 'NONE', 'WORKASPACE' ) );
#20733 = ORIENTED_EDGE ( 'NONE', *, *, #437, .T. ) ;
#20734 = CARTESIAN_POINT ( 'NONE',  ( -40.61178118339597631, 9.038025460530262123, 56.14611646155296398 ) ) ;
#20735 = VECTOR ( 'NONE', #6765, 1000.000000000000000 ) ;
#20736 = CARTESIAN_POINT ( 'NONE',  ( -40.20068974435373121, 7.604379238274955100, 60.14930799450051779 ) ) ;
#20737 = DIRECTION ( 'NONE',  ( 0.4848096202463645921, 0.8746197071393805311, 0.000000000000000000 ) ) ;
#20738 = CARTESIAN_POINT ( 'NONE',  ( -3.124322268014796844, 11.18949478403750142, 98.72270311105292251 ) ) ;
#20739 = CARTESIAN_POINT ( 'NONE',  ( 21.09992658989238734, 31.71183152705962272, 47.04930799450051637 ) ) ;
#20740 = EDGE_LOOP ( 'NONE', ( #16589, #12947, #10622, #24146 ) ) ;
#20741 = CARTESIAN_POINT ( 'NONE',  ( 46.42154359715483736, 22.84434098701873950, 45.01148816392849739 ) ) ;
#20742 = CARTESIAN_POINT ( 'NONE',  ( -41.13156850465621517, 9.429949956619452678, 35.64930799450052490 ) ) ;
#20743 = CYLINDRICAL_SURFACE ( 'NONE', #962, 1.042135311067126979 ) ;
#20744 = CARTESIAN_POINT ( 'NONE',  ( -39.58809650894544774, 2.596771453999702661, 47.04930799450051637 ) ) ;
#20745 = AXIS2_PLACEMENT_3D ( 'NONE', #3364, #15680, #18614 ) ;
#20746 = DIRECTION ( 'NONE',  ( 0.000000000000000000, 0.000000000000000000, 1.000000000000000000 ) ) ;
#20747 = ORIENTED_EDGE ( 'NONE', *, *, #23515, .F. ) ;
#20748 = CARTESIAN_POINT ( 'NONE',  ( 47.14446097802335345, 29.60550614078797693, 44.99079124510692651 ) ) ;
#20749 = FACE_OUTER_BOUND ( 'NONE', #16866, .T. ) ;
#20750 = CARTESIAN_POINT ( 'NONE',  ( -40.53913548601165218, 7.333497694771939024, 60.31640775708849844 ) ) ;
#20751 = ORIENTED_EDGE ( 'NONE', *, *, #2718, .T. ) ;
#20752 = DIRECTION ( 'NONE',  ( -1.000000000000000000, 0.000000000000000000, 0.000000000000000000 ) ) ;
#20753 = DIRECTION ( 'NONE',  ( -0.6797146636928615981, -0.1949050434465267045, -0.7071067811865529018 ) ) ;
#20754 = DIRECTION ( 'NONE',  ( -1.000000000000000000, 0.000000000000000000, 0.000000000000000000 ) ) ;
#20755 = EDGE_CURVE ( 'NONE', #25773, #4682, #31331, .T. ) ;
#20756 = CARTESIAN_POINT ( 'NONE',  ( 54.78407068788227008, -1.823725651226680400, -7.696569431702434905 ) ) ;
#20757 = EDGE_CURVE ( 'NONE', #17347, #9190, #13184, .T. ) ;
#20758 = ADVANCED_FACE ( 'NONE', ( #31218 ), #21873, .T. ) ;
#20759 = ORIENTED_EDGE ( 'NONE', *, *, #2813, .T. ) ;
#20760 = ADVANCED_FACE ( 'NONE', ( #8247 ), #10884, .F. ) ;
#20761 = CARTESIAN_POINT ( 'NONE',  ( -40.52669582637187062, 7.652910973922025129, 60.15421819779515289 ) ) ;
#20762 = ORIENTED_EDGE ( 'NONE', *, *, #19844, .F. ) ;
#20763 = ADVANCED_FACE ( 'NONE', ( #18234 ), #28267, .T. ) ;
#20764 = CIRCLE ( 'NONE', #8718, 1.003191532947548925 ) ;
#20765 = STYLED_ITEM ( 'NONE', ( #1317 ), #18649 ) ;
#20766 = ORIENTED_EDGE ( 'NONE', *, *, #1512, .F. ) ;
#20767 =( BOUNDED_CURVE ( )  B_SPLINE_CURVE ( 3, ( #24659, #29751, #15611, #685 ),
 .UNSPECIFIED., .F., .F. ) 
 B_SPLINE_CURVE_WITH_KNOTS ( ( 4, 4 ),
 ( 1.558418845015053044E-14, 1.570796326794891673 ),
 .UNSPECIFIED. ) 
 CURVE ( )  GEOMETRIC_REPRESENTATION_ITEM ( )  RATIONAL_B_SPLINE_CURVE ( ( 1.000000000000000000, 0.8047378541243698225, 0.8047378541243698225, 1.000000000000000000 ) ) 
 REPRESENTATION_ITEM ( '' )  );
#20768 = LINE ( 'NONE', #16159, #27568 ) ;
#20769 = CARTESIAN_POINT ( 'NONE',  ( -36.34052844068784083, -5.745355918706371412, 78.84831695185476974 ) ) ;
#20770 = CARTESIAN_POINT ( 'NONE',  ( 81.72575882806418690, -5.935340315990521809, 15.93528473569102566 ) ) ;
#20771 = ORIENTED_EDGE ( 'NONE', *, *, #7201, .F. ) ;
#20772 = CARTESIAN_POINT ( 'NONE',  ( 81.63175399755476747, -5.935454207809698346, 78.02743327247107175 ) ) ;
#20773 = ORIENTED_EDGE ( 'NONE', *, *, #14682, .F. ) ;
#20774 = CYLINDRICAL_SURFACE ( 'NONE', #26694, 12.62506659569710443 ) ;
#20775 = DIRECTION ( 'NONE',  ( 0.8746197071393926326, -0.4848096202463430537, -8.676864087101709653E-18 ) ) ;
#20776 = CARTESIAN_POINT ( 'NONE',  ( -30.67097509423727786, 6.595730531473362745, 76.60775000090053766 ) ) ;
#20777 = EDGE_CURVE ( 'NONE', #12577, #25082, #5107, .T. ) ;
#20778 = EDGE_LOOP ( 'NONE', ( #8551, #26019, #1751, #15645 ) ) ;
#20779 = DIRECTION ( 'NONE',  ( -1.000000000000000000, 0.000000000000000000, 0.000000000000000000 ) ) ;
#20780 = VERTEX_POINT ( 'NONE', #23498 ) ;
#20781 = CARTESIAN_POINT ( 'NONE',  ( 21.09785597605720753, -13.64309448858209528, 105.9390803697710339 ) ) ;
#20783 = DIRECTION ( 'NONE',  ( 0.000000000000000000, 0.000000000000000000, -1.000000000000000000 ) ) ;
#20782 = VECTOR ( 'NONE', #1609, 1000.000000000000114 ) ;
#20784 = VERTEX_POINT ( 'NONE', #3470 ) ;
#20785 = DIRECTION ( 'NONE',  ( 0.000000000000000000, 0.000000000000000000, -1.000000000000000000 ) ) ;
#20786 = CARTESIAN_POINT ( 'NONE',  ( 81.56333945993378620, -5.935454207834600204, 15.93786612339379083 ) ) ;
#20787 = CARTESIAN_POINT ( 'NONE',  ( -39.67555847965937943, 2.645252416024337361, 47.04930799450051637 ) ) ;
#20788 = CARTESIAN_POINT ( 'NONE',  ( -40.75848109938849717, 9.580021662090986823, 35.54930799450052348 ) ) ;
#20789 = CARTESIAN_POINT ( 'NONE',  ( 48.40186567930498285, 25.32957786121582089, 45.03923535223908203 ) ) ;
#20790 = ORIENTED_EDGE ( 'NONE', *, *, #6448, .F. ) ;
#20791 = CARTESIAN_POINT ( 'NONE',  ( -43.64073206722599707, 1.267352857069779848, 39.44930799450052916 ) ) ;
#20792 = CARTESIAN_POINT ( 'NONE',  ( -40.59768508530252973, 7.003142309053439263, 35.04175310890629902 ) ) ;
#20793 = VERTEX_POINT ( 'NONE', #29227 ) ;
#20794 = DIRECTION ( 'NONE',  ( -0.000000000000000000, -1.000000000000000000, 0.000000000000000000 ) ) ;
#20795 = AXIS2_PLACEMENT_3D ( 'NONE', #24643, #19710, #22004 ) ;
#20796 = LINE ( 'NONE', #30984, #17439 ) ;
#20797 = ADVANCED_FACE ( 'NONE', ( #21831 ), #19764, .T. ) ;
#20798 = ADVANCED_FACE ( 'NONE', ( #9541 ), #4112, .F. ) ;
#20799 = EDGE_LOOP ( 'NONE', ( #8564, #12599, #6897, #6958 ) ) ;
#20800 = EDGE_CURVE ( 'NONE', #31909, #29041, #2130, .T. ) ;
#20801 = ORIENTED_EDGE ( 'NONE', *, *, #20892, .F. ) ;
#20802 = CARTESIAN_POINT ( 'NONE',  ( -12.63022165813546849, -2.878806504921737730, 102.4552866314799218 ) ) ;
#20803 = ADVANCED_FACE ( 'NONE', ( #11997 ), #29065, .T. ) ;
#20804 = EDGE_LOOP ( 'NONE', ( #27465, #22612, #25659, #15960 ) ) ;
#20805 = AXIS2_PLACEMENT_3D ( 'NONE', #7360, #4729, #29522 ) ;
#20806 = ORIENTED_EDGE ( 'NONE', *, *, #31627, .T. ) ;
#20807 = CARTESIAN_POINT ( 'NONE',  ( 8.474859994195286461, 27.34143805560860940, 47.04930799450051637 ) ) ;
#20808 = AXIS2_PLACEMENT_3D ( 'NONE', #14372, #11410, #6816 ) ;
#20809 = VERTEX_POINT ( 'NONE', #32018 ) ;
#20810 = DIRECTION ( 'NONE',  ( -0.2756373558170044369, 0.9612616959383173398, 1.315048337272769818E-17 ) ) ;
#20811 = CARTESIAN_POINT ( 'NONE',  ( 48.14727188781975542, 19.96454579224779380, 49.10650501410607660 ) ) ;
#20812 = DIRECTION ( 'NONE',  ( -1.000000000000000000, -1.101824276508909887E-16, 0.000000000000000000 ) ) ;
#20813 = CARTESIAN_POINT ( 'NONE',  ( 45.38854177497844944, 27.62622849631042499, 45.94041160078741370 ) ) ;
#20814 = EDGE_CURVE ( 'NONE', #25945, #11226, #27649, .T. ) ;
#20815 = ORIENTED_EDGE ( 'NONE', *, *, #10044, .T. ) ;
#20816 = ORIENTED_EDGE ( 'NONE', *, *, #7573, .T. ) ;
#20817 = CARTESIAN_POINT ( 'NONE',  ( 33.72499318558949710, 29.84143805560861296, 47.04930799450051637 ) ) ;
#20818 = EDGE_CURVE ( 'NONE', #26923, #3283, #4602, .T. ) ;
#20819 = ORIENTED_EDGE ( 'NONE', *, *, #13642, .T. ) ;
#20820 = DIRECTION ( 'NONE',  ( -0.000000000000000000, -1.000000000000000000, 0.000000000000000000 ) ) ;
#20821 = CARTESIAN_POINT ( 'NONE',  ( -40.02996145527347949, 7.371774464818581230, 60.41996114768177506 ) ) ;
#20822 = AXIS2_PLACEMENT_3D ( 'NONE', #18973, #27027, #29499 ) ;
#20823 = FACE_OUTER_BOUND ( 'NONE', #27875, .T. ) ;
#20824 = DIRECTION ( 'NONE',  ( 0.000000000000000000, 0.000000000000000000, -1.000000000000000000 ) ) ;
#20825 = ORIENTED_EDGE ( 'NONE', *, *, #13208, .T. ) ;
#20826 = DIRECTION ( 'NONE',  ( -0.8746197071393925215, 0.4848096202463429982, 8.676864087101709653E-18 ) ) ;
#20827 = CIRCLE ( 'NONE', #19243, 0.1000000000000018235 ) ;
#20828 = CARTESIAN_POINT ( 'NONE',  ( 21.09992658989239089, 29.09164230456639899, 47.04930799450051637 ) ) ;
#20829 = PLANE ( 'NONE',  #23548 ) ;
#20830 = DIRECTION ( 'NONE',  ( -1.101824276508909887E-16, 1.000000000000000000, -0.000000000000000000 ) ) ;
#20831 = AXIS2_PLACEMENT_3D ( 'NONE', #13219, #7797, #18271 ) ;
#20832 = VERTEX_POINT ( 'NONE', #18877 ) ;
#20833 = DIRECTION ( 'NONE',  ( -0.000000000000000000, 1.000000000000000000, -0.000000000000000000 ) ) ;
#20834 = CARTESIAN_POINT ( 'NONE',  ( -40.57832939096746827, 7.446916270396702231, 53.86067862812341644 ) ) ;
#20835 = EDGE_CURVE ( 'NONE', #28214, #19781, #23980, .T. ) ;
#20836 = APPLICATION_CONTEXT ( 'automotive_design' ) ;
#20837 = ORIENTED_EDGE ( 'NONE', *, *, #17792, .F. ) ;
#20838 = ORIENTED_EDGE ( 'NONE', *, *, #936, .T. ) ;
#20839 = ORIENTED_EDGE ( 'NONE', *, *, #22374, .F. ) ;
#20840 = EDGE_CURVE ( 'NONE', #4855, #17564, #26607, .T. ) ;
#20841 = FACE_OUTER_BOUND ( 'NONE', #11133, .T. ) ;
#20842 = PLANE ( 'NONE',  #7864 ) ;
#20843 = VECTOR ( 'NONE', #4933, 1000.000000000000227 ) ;
#20844 = EDGE_CURVE ( 'NONE', #8655, #7408, #19815, .T. ) ;
#20845 = ORIENTED_EDGE ( 'NONE', *, *, #20448, .T. ) ;
#20846 = DIRECTION ( 'NONE',  ( 0.000000000000000000, 0.000000000000000000, -1.000000000000000000 ) ) ;
#20847 = CIRCLE ( 'NONE', #16139, 0.1250000000000001110 ) ;
#20848 = CARTESIAN_POINT ( 'NONE',  ( 81.47236153510795020, -5.936967987714544037, 16.00176942158120141 ) ) ;
#20849 = FACE_OUTER_BOUND ( 'NONE', #8980, .T. ) ;
#20850 = EDGE_CURVE ( 'NONE', #12194, #2898, #8022, .T. ) ;
#20851 = ORIENTED_EDGE ( 'NONE', *, *, #29021, .T. ) ;
#20852 = CARTESIAN_POINT ( 'NONE',  ( -40.11286833322907341, 2.887657226147507306, 37.04930799450052348 ) ) ;
#20853 = EDGE_CURVE ( 'NONE', #11589, #22710, #13686, .T. ) ;
#20854 = EDGE_LOOP ( 'NONE', ( #14148, #26854, #31779, #29427 ) ) ;
#20855 = CARTESIAN_POINT ( 'NONE',  ( 45.96182992765472619, 27.30087065737811969, 44.82232689504102296 ) ) ;
#20856 = EDGE_CURVE ( 'NONE', #18541, #9841, #8528, .T. ) ;
#20857 = DIRECTION ( 'NONE',  ( -1.000000000000000000, 0.000000000000000000, 0.000000000000000000 ) ) ;
#20858 = DIRECTION ( 'NONE',  ( 0.000000000000000000, 0.000000000000000000, 1.000000000000000000 ) ) ;
#20859 = DIRECTION ( 'NONE',  ( -1.000000000000000000, 0.000000000000000000, 0.000000000000000000 ) ) ;
#20860 = CARTESIAN_POINT ( 'NONE',  ( 46.71168188241476571, 25.16454579224780019, 44.57931415454905988 ) ) ;
#20861 = FACE_OUTER_BOUND ( 'NONE', #25809, .T. ) ;
#20862 = EDGE_LOOP ( 'NONE', ( #2478, #13429, #5105, #31277 ) ) ;
#20863 = ORIENTED_EDGE ( 'NONE', *, *, #17045, .F. ) ;
#20864 = CARTESIAN_POINT ( 'NONE',  ( 49.06850489496600431, -13.30632128221581212, 95.48546547976138754 ) ) ;
#20865 = CARTESIAN_POINT ( 'NONE',  ( 21.09785597605719332, 24.86454579224779948, 75.54930799450052348 ) ) ;
#20866 = ORIENTED_EDGE ( 'NONE', *, *, #19696, .T. ) ;
#20867 = DIRECTION ( 'NONE',  ( 0.000000000000000000, 0.000000000000000000, 1.000000000000000000 ) ) ;
#20868 = CARTESIAN_POINT ( 'NONE',  ( 48.23388202445966044, 28.22822092656774373, 49.27628909396054979 ) ) ;
#20869 = ORIENTED_EDGE ( 'NONE', *, *, #20565, .T. ) ;
#20870 = CARTESIAN_POINT ( 'NONE',  ( 45.73035263060504718, 27.93954579807170546, 44.36855633853329550 ) ) ;
#20871 = ADVANCED_FACE ( 'NONE', ( #13307 ), #4609, .T. ) ;
#20872 = CARTESIAN_POINT ( 'NONE',  ( 48.83862994770794330, 27.95457786121581734, 48.17861352429476796 ) ) ;
#20873 = CIRCLE ( 'NONE', #25583, 31.00000000000000000 ) ;
#20874 = CARTESIAN_POINT ( 'NONE',  ( -39.50399991082505124, -5.935463013562887191, 77.87581693445018516 ) ) ;
#20875 = AXIS2_PLACEMENT_3D ( 'NONE', #16297, #18590, #10904 ) ;
#20876 = AXIS2_PLACEMENT_3D ( 'NONE', #8325, #18322, #5876 ) ;
#20877 = AXIS2_PLACEMENT_3D ( 'NONE', #4303, #12014, #32040 ) ;
#20878 = ORIENTED_EDGE ( 'NONE', *, *, #12545, .F. ) ;
#20879 = EDGE_CURVE ( 'NONE', #10718, #27541, #18209, .T. ) ;
#20880 = DIRECTION ( 'NONE',  ( -1.101824276508909887E-16, 1.000000000000000000, -0.000000000000000000 ) ) ;
#20881 = DIRECTION ( 'NONE',  ( 0.9612616959383205595, 0.2756373558169932236, -1.660411357259282445E-16 ) ) ;
#20882 = ADVANCED_FACE ( 'NONE', ( #25762 ), #25597, .F. ) ;
#20883 = EDGE_LOOP ( 'NONE', ( #31106, #30994, #12215, #13749 ) ) ;
#20884 = DIRECTION ( 'NONE',  ( -0.6184495258776593340, 0.3428121700606657773, 0.7071067811865443531 ) ) ;
#20885 = CARTESIAN_POINT ( 'NONE',  ( 21.09785597605719332, 17.36451738380053555, 47.04930799450051637 ) ) ;
#20886 = DIRECTION ( 'NONE',  ( -0.03087013654144218910, 0.1076569600579696390, 0.9937087166876367172 ) ) ;
#20887 = VECTOR ( 'NONE', #19346, 1000.000000000000000 ) ;
#20888 = EDGE_CURVE ( 'NONE', #11938, #7606, #8801, .T. ) ;
#20889 = CIRCLE ( 'NONE', #30863, 19.21451602543517367 ) ;
#20890 = EDGE_LOOP ( 'NONE', ( #5260, #8871, #22495, #18924 ) ) ;
#20891 = CARTESIAN_POINT ( 'NONE',  ( -41.02113223168485234, 7.230835263863472306, 39.54930799450052348 ) ) ;
#20892 = EDGE_CURVE ( 'NONE', #22237, #10875, #32391, .T. ) ;
#20893 = AXIS2_PLACEMENT_3D ( 'NONE', #26110, #11499, #3954 ) ;
#20894 = CARTESIAN_POINT ( 'NONE',  ( 47.34331760472088746, 10.07047442526145531, 97.52091674703079605 ) ) ;
#20895 = DIRECTION ( 'NONE',  ( -0.8746197071393805311, 0.4848096202463645921, 8.676864087101954631E-18 ) ) ;
#20896 = CARTESIAN_POINT ( 'NONE',  ( 0.1373481117363317960, 11.91446173404583853, -4.734257055995808372 ) ) ;
#20897 = VERTEX_POINT ( 'NONE', #23137 ) ;
#20898 = CARTESIAN_POINT ( 'NONE',  ( 46.84209603737756566, 23.10527845304106620, 46.54793520446708044 ) ) ;
#20899 = CARTESIAN_POINT ( 'NONE',  ( 21.09785597605720753, -5.098646251524523443, 47.04930799450052348 ) ) ;
#20900 = FACE_OUTER_BOUND ( 'NONE', #26548, .T. ) ;
#20901 = CARTESIAN_POINT ( 'NONE',  ( -40.13633318854532916, 6.906174383240056613, 34.55842931802699525 ) ) ;
#20902 = AXIS2_PLACEMENT_3D ( 'NONE', #27943, #3308, #25949 ) ;
#20903 = CARTESIAN_POINT ( 'NONE',  ( 76.74774710317745985, -3.218976025669015417, 80.73895664570260067 ) ) ;
#20904 = ORIENTED_EDGE ( 'NONE', *, *, #32359, .T. ) ;
#20905 = DIRECTION ( 'NONE',  ( -1.000000000000000000, 0.000000000000000000, 0.000000000000000000 ) ) ;
#20906 = DIRECTION ( 'NONE',  ( 0.9612616959383205595, 0.2756373558169932236, -1.660411357259282445E-16 ) ) ;
#20907 = CARTESIAN_POINT ( 'NONE',  ( -40.17244512953781310, 6.931285263614340941, 39.54930799450052348 ) ) ;
#20908 = EDGE_LOOP ( 'NONE', ( #2234, #1093, #3942, #19546 ) ) ;
#20909 = DIRECTION ( 'NONE',  ( -2.779292025043186357E-18, 1.288349127009862211E-17, -1.000000000000000000 ) ) ;
#20910 = LINE ( 'NONE', #30937, #15191 ) ;
#20911 = DIRECTION ( 'NONE',  ( 0.000000000000000000, 0.000000000000000000, 1.000000000000000000 ) ) ;
#20912 = CARTESIAN_POINT ( 'NONE',  ( -41.13768170161382898, 11.26524684725914227, 38.19144330556764544 ) ) ;
#20913 = ORIENTED_EDGE ( 'NONE', *, *, #19059, .T. ) ;
#20914 = DIRECTION ( 'NONE',  ( 0.000000000000000000, 1.000000000000000000, -0.000000000000000000 ) ) ;
#20915 = ORIENTED_EDGE ( 'NONE', *, *, #11930, .T. ) ;
#20916 = AXIS2_PLACEMENT_3D ( 'NONE', #14925, #24938, #24770 ) ;
#20917 = AXIS2_PLACEMENT_3D ( 'NONE', #4411, #2551, #20112 ) ;
#20918 = ORIENTED_EDGE ( 'NONE', *, *, #23858, .T. ) ;
#20919 = CIRCLE ( 'NONE', #26690, 13.81487396812510937 ) ;
#20920 = CIRCLE ( 'NONE', #22574, 12.36707279061065279 ) ;
#20921 = CARTESIAN_POINT ( 'NONE',  ( 48.83059987400640978, 27.55948166895303686, 48.97189179988552610 ) ) ;
#20922 = DIRECTION ( 'NONE',  ( -0.2756373558169932236, 0.9612616959383205595, -2.271050992151962865E-31 ) ) ;
#20923 = CARTESIAN_POINT ( 'NONE',  ( 48.23388202445966044, 26.12822092656774586, 49.27628909396054979 ) ) ;
#20924 = EDGE_CURVE ( 'NONE', #9190, #5852, #20509, .T. ) ;
#20925 = ORIENTED_EDGE ( 'NONE', *, *, #8766, .F. ) ;
#20926 = LINE ( 'NONE', #18464, #23471 ) ;
#20927 = ORIENTED_EDGE ( 'NONE', *, *, #20564, .T. ) ;
#20928 = ADVANCED_FACE ( 'NONE', ( #8692 ), #23623, .F. ) ;
#20929 = DIRECTION ( 'NONE',  ( -1.000000000000000000, 0.000000000000000000, 0.000000000000000000 ) ) ;
#20930 = DIRECTION ( 'NONE',  ( -1.101824276508909887E-16, 1.000000000000000000, -0.000000000000000000 ) ) ;
#20931 = DIRECTION ( 'NONE',  ( 0.000000000000000000, 0.000000000000000000, -1.000000000000000000 ) ) ;
#20932 = DIRECTION ( 'NONE',  ( -1.101824276508909887E-16, 1.000000000000000000, -0.000000000000000000 ) ) ;
#20933 = VERTEX_POINT ( 'NONE', #23940 ) ;
#20934 = FACE_OUTER_BOUND ( 'NONE', #13588, .T. ) ;
#20935 = CARTESIAN_POINT ( 'NONE',  ( -4.902144023942810236, 25.56454579224779877, 47.04930799450078638 ) ) ;
#20936 = FACE_OUTER_BOUND ( 'NONE', #9625, .T. ) ;
#20937 = CARTESIAN_POINT ( 'NONE',  ( 21.09785597605719332, 30.56454579224779522, 60.24930799450052632 ) ) ;
#20938 = CIRCLE ( 'NONE', #12017, 12.36707279061065101 ) ;
#20939 = ORIENTED_EDGE ( 'NONE', *, *, #8890, .T. ) ;
#20940 = DIRECTION ( 'NONE',  ( -1.000000000000000000, 0.000000000000000000, 0.000000000000000000 ) ) ;
#20941 = AXIS2_PLACEMENT_3D ( 'NONE', #17805, #5181, #15189 ) ;
#20942 = FACE_OUTER_BOUND ( 'NONE', #23646, .T. ) ;
#20943 = FACE_OUTER_BOUND ( 'NONE', #20799, .T. ) ;
#20944 = DIRECTION ( 'NONE',  ( 0.000000000000000000, 0.000000000000000000, -1.000000000000000000 ) ) ;
#20945 = CARTESIAN_POINT ( 'NONE',  ( 33.72499318558949710, 31.84184655352418503, 47.04930799450051637 ) ) ;
#20946 = VERTEX_POINT ( 'NONE', #23776 ) ;
#20947 = CARTESIAN_POINT ( 'NONE',  ( 48.50303063523655567, 22.99884124225578574, 47.12228595530052644 ) ) ;
#20948 = CARTESIAN_POINT ( 'NONE',  ( -40.56019413908506266, 7.186695055018779144, 35.29694535755109541 ) ) ;
#20949 = ORIENTED_EDGE ( 'NONE', *, *, #3259, .T. ) ;
#20950 = DIRECTION ( 'NONE',  ( -1.224646799147353207E-16, 0.000000000000000000, -1.000000000000000000 ) ) ;
#20951 = CIRCLE ( 'NONE', #4170, 0.09999999999999886757 ) ;
#20952 = CARTESIAN_POINT ( 'NONE',  ( 8.482002859293402253, 24.71664230456639899, 47.04930799450051637 ) ) ;
#20953 = EDGE_LOOP ( 'NONE', ( #32432, #16236 ) ) ;
#20954 = ORIENTED_EDGE ( 'NONE', *, *, #21181, .F. ) ;
#20955 = CARTESIAN_POINT ( 'NONE',  ( -12.34210598815197812, -0.7249253372050598054, 101.2314873363451966 ) ) ;
#20956 = CIRCLE ( 'NONE', #9435, 0.1000000000000028644 ) ;
#20957 = ORIENTED_EDGE ( 'NONE', *, *, #13898, .T. ) ;
#20958 = VECTOR ( 'NONE', #8434, 1000.000000000000114 ) ;
#20959 = ORIENTED_EDGE ( 'NONE', *, *, #24470, .F. ) ;
#20960 = CARTESIAN_POINT ( 'NONE',  ( 80.77181806311267565, 5.388785998227650254, 16.47908017486096099 ) ) ;
#20961 = CIRCLE ( 'NONE', #28831, 12.36707279061065101 ) ;
#20962 = CIRCLE ( 'NONE', #7894, 12.27641737965288371 ) ;
#20963 = ORIENTED_EDGE ( 'NONE', *, *, #30871, .T. ) ;
#20964 = EDGE_CURVE ( 'NONE', #16293, #18953, #10392, .T. ) ;
#20965 = SPHERICAL_SURFACE ( 'NONE', #978, 0.1000000000000000056 ) ;
#20966 = EDGE_CURVE ( 'NONE', #1894, #8733, #4076, .T. ) ;
#20967 = AXIS2_PLACEMENT_3D ( 'NONE', #20091, #721, #27484 ) ;
#20968 = FACE_OUTER_BOUND ( 'NONE', #24602, .T. ) ;
#20969 = DIRECTION ( 'NONE',  ( 0.000000000000000000, 0.000000000000000000, -1.000000000000000000 ) ) ;
#20970 = ADVANCED_FACE ( 'NONE', ( #31665 ), #15091, .F. ) ;
#20971 = EDGE_CURVE ( 'NONE', #25738, #15396, #29356, .T. ) ;
#20972 = CARTESIAN_POINT ( 'NONE',  ( 46.99218062947583974, 25.75956182964376495, 49.08406571254116102 ) ) ;
#20973 = AXIS2_PLACEMENT_3D ( 'NONE', #14051, #19112, #24047 ) ;
#20974 = AXIS2_PLACEMENT_3D ( 'NONE', #31222, #8883, #10879 ) ;
#20975 = ORIENTED_EDGE ( 'NONE', *, *, #6774, .F. ) ;
#20976 = ORIENTED_EDGE ( 'NONE', *, *, #21150, .F. ) ;
#20977 = ORIENTED_EDGE ( 'NONE', *, *, #14864, .F. ) ;
#20978 = CARTESIAN_POINT ( 'NONE',  ( 43.71041224836975658, 11.69686719848734313, 99.14099691200772213 ) ) ;
#20979 = CARTESIAN_POINT ( 'NONE',  ( 53.55890038120063679, -5.379633064793138963, 104.8034930254145252 ) ) ;
#20980 = CARTESIAN_POINT ( 'NONE',  ( 7.596071960694297687, 16.03967147762301693, 47.04930799450052348 ) ) ;
#20981 = DIRECTION ( 'NONE',  ( -1.000000000000000000, 0.000000000000000000, 0.000000000000000000 ) ) ;
#20982 = DIRECTION ( 'NONE',  ( 1.000000000000000000, 0.000000000000000000, 0.000000000000000000 ) ) ;
#20983 = ITEM_DEFINED_TRANSFORMATION ( 'NONE', 'NONE', #17077,  #8172 ) ;
#20984 = ORIENTED_EDGE ( 'NONE', *, *, #18189, .T. ) ;
#20985 = CARTESIAN_POINT ( 'NONE',  ( 8.474859994195286461, 23.84184655352419213, 47.04930799450051637 ) ) ;
#20986 = CARTESIAN_POINT ( 'NONE',  ( -32.52043329404533267, -1.482047863521116060, 13.42356643302901453 ) ) ;
#20987 = AXIS2_PLACEMENT_3D ( 'NONE', #9236, #21201, #26792 ) ;
#20988 = CARTESIAN_POINT ( 'NONE',  ( -40.15599670534037102, 7.478908884098767196, 35.39279590939684539 ) ) ;
#20989 = CARTESIAN_POINT ( 'NONE',  ( 21.09785597605719332, -16.43545420775217281, 47.04930799450051637 ) ) ;
#20990 = CARTESIAN_POINT ( 'NONE',  ( 48.04075769285628894, 25.18284706826092290, 48.89770225776209145 ) ) ;
#20991 = ORIENTED_EDGE ( 'NONE', *, *, #6994, .T. ) ;
#20992 = DIRECTION ( 'NONE',  ( -0.4848096202463429427, -0.8746197071393925215, 2.352477780477436787E-16 ) ) ;
#20993 = LINE ( 'NONE', #3276, #7274 ) ;
#20994 = TOROIDAL_SURFACE ( 'NONE', #26762, 55.59552431147871232, 1.000000000000000000 ) ;
#20995 = VERTEX_POINT ( 'NONE', #28879 ) ;
#20996 = AXIS2_PLACEMENT_3D ( 'NONE', #16725, #1967, #4592 ) ;
#20997 = ADVANCED_FACE ( 'NONE', ( #18839 ), #27145, .T. ) ;
#20998 = AXIS2_PLACEMENT_3D ( 'NONE', #23416, #10796, #13098 ) ;
#20999 = ORIENTED_EDGE ( 'NONE', *, *, #17668, .T. ) ;
#21000 = DIRECTION ( 'NONE',  ( -0.9612616959383194493, -0.2756373558169974980, -8.795445018804946186E-19 ) ) ;
#21001 = CARTESIAN_POINT ( 'NONE',  ( 75.19785597605721250, 14.36454579224779948, 47.04930799450052348 ) ) ;
#21002 = ORIENTED_EDGE ( 'NONE', *, *, #12836, .T. ) ;
#21003 = CARTESIAN_POINT ( 'NONE',  ( 6.626556088358270813, -13.30632128221581212, 101.0770789316966329 ) ) ;
#21004 = CARTESIAN_POINT ( 'NONE',  ( 21.09785597605720042, -13.68834655544033652, -8.644984113562347972 ) ) ;
#21005 = EDGE_CURVE ( 'NONE', #8194, #29763, #21364, .T. ) ;
#21006 = VERTEX_POINT ( 'NONE', #11803 ) ;
#21007 = LINE ( 'NONE', #23956, #5487 ) ;
#21008 = ORIENTED_EDGE ( 'NONE', *, *, #12647, .T. ) ;
#21009 = LINE ( 'NONE', #3456, #6036 ) ;
#21010 = DIRECTION ( 'NONE',  ( 0.000000000000000000, -1.000000000000000000, 0.000000000000000000 ) ) ;
#21011 = DIRECTION ( 'NONE',  ( -0.000000000000000000, -1.000000000000000000, 0.000000000000000000 ) ) ;
#21012 = CARTESIAN_POINT ( 'NONE',  ( 48.14727188781975542, 22.80400562401890241, 49.10650501410607660 ) ) ;
#21013 = AXIS2_PLACEMENT_3D ( 'NONE', #27202, #10309, #7843 ) ;
#21014 = AXIS2_PLACEMENT_3D ( 'NONE', #31403, #6125, #23998 ) ;
#21015 = VERTEX_POINT ( 'NONE', #19330 ) ;
#21016 = VERTEX_POINT ( 'NONE', #24098 ) ;
#21017 = CARTESIAN_POINT ( 'NONE',  ( -40.05987053574653345, 7.506472619680471858, 35.90717268343339441 ) ) ;
#21018 = CIRCLE ( 'NONE', #21921, 12.62506659569710266 ) ;
#21019 = CARTESIAN_POINT ( 'NONE',  ( 21.09785597605720753, 14.36454579224779948, 47.04930799450052348 ) ) ;
#21020 = CARTESIAN_POINT ( 'NONE',  ( 21.09785597605720753, 14.86454579224779948, 47.04930799450052348 ) ) ;
#21021 = EDGE_LOOP ( 'NONE', ( #1277, #28513, #6062, #24741 ) ) ;
#21022 = LINE ( 'NONE', #25798, #3526 ) ;
#21023 = CARTESIAN_POINT ( 'NONE',  ( 21.09785597605719332, 30.56454579224779522, 18.54930799450051282 ) ) ;
#21024 = EDGE_CURVE ( 'NONE', #7765, #7100, #26729, .T. ) ;
#21025 = ORIENTED_EDGE ( 'NONE', *, *, #8746, .F. ) ;
#21026 = CYLINDRICAL_SURFACE ( 'NONE', #28327, 0.1000000000000006301 ) ;
#21027 = CARTESIAN_POINT ( 'NONE',  ( 50.10320668408830613, 29.10621246473837331, 47.20539118556276037 ) ) ;
#21028 = CIRCLE ( 'NONE', #2694, 0.09999999999999904798 ) ;
#21029 = EDGE_CURVE ( 'NONE', #8460, #13336, #9842, .T. ) ;
#21030 = CARTESIAN_POINT ( 'NONE',  ( -39.43067640719859668, -5.935531758779752032, 77.98141296025164593 ) ) ;
#21031 = ADVANCED_FACE ( 'NONE', ( #26245 ), #19003, .T. ) ;
#21032 = EDGE_CURVE ( 'NONE', #17658, #16985, #28194, .T. ) ;
#21033 = VERTEX_POINT ( 'NONE', #21304 ) ;
#21034 = AXIS2_PLACEMENT_3D ( 'NONE', #5014, #2704, #10104 ) ;
#21035 = AXIS2_PLACEMENT_3D ( 'NONE', #8488, #14056, #28990 ) ;
#21036 = COLOUR_RGB ( '',0.7921568627450980005, 0.8196078431372548767, 0.9333333333333333481 ) ;
#21037 = CARTESIAN_POINT ( 'NONE',  ( 21.09992658989239089, 28.84164230456639544, 47.04930799450051637 ) ) ;
#21038 = DIRECTION ( 'NONE',  ( -0.000000000000000000, -1.000000000000000000, 0.000000000000000000 ) ) ;
#21039 = ORIENTED_EDGE ( 'NONE', *, *, #13760, .F. ) ;
#21040 = CARTESIAN_POINT ( 'NONE',  ( 21.09785597605720397, -16.43545420775217281, -37.95069200549950494 ) ) ;
#21041 = DIRECTION ( 'NONE',  ( 8.659560562354932858E-17, -0.7071067811865474617, 0.7071067811865474617 ) ) ;
#21042 = ADVANCED_FACE ( 'NONE', ( #4249 ), #14032, .T. ) ;
#21043 = AXIS2_PLACEMENT_3D ( 'NONE', #20697, #30725, #18667 ) ;
#21044 = DIRECTION ( 'NONE',  ( -0.8746197071393790878, 0.4848096202463673676, 1.277302113040196197E-17 ) ) ;
#21045 = VERTEX_POINT ( 'NONE', #21463 ) ;
#21046 = DIRECTION ( 'NONE',  ( 0.000000000000000000, 0.000000000000000000, 1.000000000000000000 ) ) ;
#21047 = CARTESIAN_POINT ( 'NONE',  ( -12.90214402394279603, 14.86454579224779948, 47.04930799450052348 ) ) ;
#21048 = DIRECTION ( 'NONE',  ( -1.000000000000000000, 0.000000000000000000, 0.000000000000000000 ) ) ;
#21049 = FACE_OUTER_BOUND ( 'NONE', #17547, .T. ) ;
#21050 = DIRECTION ( 'NONE',  ( 0.000000000000000000, 0.000000000000000000, 1.000000000000000000 ) ) ;
#21051 = ORIENTED_EDGE ( 'NONE', *, *, #29353, .F. ) ;
#21052 = DIRECTION ( 'NONE',  ( -1.000000000000000000, 0.000000000000000000, 0.000000000000000000 ) ) ;
#21053 = DIRECTION ( 'NONE',  ( -1.000000000000000000, 0.000000000000000000, 0.000000000000000000 ) ) ;
#21054 = CARTESIAN_POINT ( 'NONE',  ( -40.38311397581032480, 8.599301472032985671, 34.60485935866290674 ) ) ;
#21055 = DIRECTION ( 'NONE',  ( 0.000000000000000000, -0.000000000000000000, -1.000000000000000000 ) ) ;
#21056 = CIRCLE ( 'NONE', #24203, 0.1250000000000001110 ) ;
#21057 = CARTESIAN_POINT ( 'NONE',  ( 79.40776106085759523, -5.721341737285999152, 78.89649703355206611 ) ) ;
#21058 = ORIENTED_EDGE ( 'NONE', *, *, #9830, .T. ) ;
#21059 = AXIS2_PLACEMENT_3D ( 'NONE', #10109, #25198, #24709 ) ;
#21060 = FACE_OUTER_BOUND ( 'NONE', #31646, .T. ) ;
#21061 = CARTESIAN_POINT ( 'NONE',  ( 49.70065004996131819, 24.90951171049934842, 46.59606017514272480 ) ) ;
#21062 = CARTESIAN_POINT ( 'NONE',  ( -58.11219453028166981, -15.93545420775219945, 47.04930799450023926 ) ) ;
#21063 = EDGE_CURVE ( 'NONE', #13529, #25136, #21635, .T. ) ;
#21064 = VERTEX_POINT ( 'NONE', #1784 ) ;
#21065 = DIRECTION ( 'NONE',  ( -1.101824276508909887E-16, 1.000000000000000000, -0.000000000000000000 ) ) ;
#21066 = DIRECTION ( 'NONE',  ( -1.000000000000000000, -1.101824276508909887E-16, 0.000000000000000000 ) ) ;
#21067 = DIRECTION ( 'NONE',  ( -0.000000000000000000, -1.000000000000000000, -0.000000000000000000 ) ) ;
#21068 = ADVANCED_FACE ( 'NONE', ( #21798 ), #9330, .T. ) ;
#21069 = DIRECTION ( 'NONE',  ( 0.000000000000000000, 0.000000000000000000, -1.000000000000000000 ) ) ;
#21070 = ORIENTED_EDGE ( 'NONE', *, *, #31836, .T. ) ;
#21071 = CARTESIAN_POINT ( 'NONE',  ( 73.74367965647046219, 11.91444431924556113, 26.08837878683308986 ) ) ;
#21072 = ORIENTED_EDGE ( 'NONE', *, *, #10951, .F. ) ;
#21073 = AXIS2_PLACEMENT_3D ( 'NONE', #5821, #2863, #17958 ) ;
#21074 = ADVANCED_FACE ( 'NONE', ( #26013 ), #16163, .T. ) ;
#21075 = ORIENTED_EDGE ( 'NONE', *, *, #22871, .T. ) ;
#21076 = EDGE_CURVE ( 'NONE', #9745, #24444, #11892, .T. ) ;
#21077 = AXIS2_PLACEMENT_3D ( 'NONE', #8868, #18866, #1965 ) ;
#21078 = CIRCLE ( 'NONE', #19509, 25.50000000000000355 ) ;
#21079 = TOROIDAL_SURFACE ( 'NONE', #17411, 12.40141737965283575, 0.1250000000000000278 ) ;
#21080 = DIRECTION ( 'NONE',  ( -1.101824276508909887E-16, 1.000000000000000000, -0.000000000000000000 ) ) ;
#21081 = DIRECTION ( 'NONE',  ( -1.101824276508909887E-16, 1.000000000000000000, -0.000000000000000000 ) ) ;
#21082 = CARTESIAN_POINT ( 'NONE',  ( 45.96182992765471909, 27.17822092656774302, 44.82232689504102296 ) ) ;
#21083 = ORIENTED_EDGE ( 'NONE', *, *, #24064, .T. ) ;
#21084 = DIRECTION ( 'NONE',  ( 0.000000000000000000, 0.000000000000000000, -1.000000000000000000 ) ) ;
#21085 = ORIENTED_EDGE ( 'NONE', *, *, #9574, .T. ) ;
#21086 = CARTESIAN_POINT ( 'NONE',  ( -6.402144023942783591, 13.86454579224779948, 47.04930799450052348 ) ) ;
#21087 = DIRECTION ( 'NONE',  ( 0.000000000000000000, 0.000000000000000000, -1.000000000000000000 ) ) ;
#21088 = CARTESIAN_POINT ( 'NONE',  ( 21.09992658989239089, 24.59143805560860940, 47.04930799450051637 ) ) ;
#21089 = VERTEX_POINT ( 'NONE', #1072 ) ;
#21090 = CARTESIAN_POINT ( 'NONE',  ( 33.50134396954523197, 28.34164230456639544, 47.04930799450051637 ) ) ;
#21091 = VERTEX_POINT ( 'NONE', #8150 ) ;
#21092 = DIRECTION ( 'NONE',  ( -0.1651779284337430986, 0.9862637841664557703, 1.316559855253201822E-17 ) ) ;
#21093 = CARTESIAN_POINT ( 'NONE',  ( -42.38351229602917414, 14.72295342448899191, 60.54930799450051637 ) ) ;
#21094 = ORIENTED_EDGE ( 'NONE', *, *, #9121, .T. ) ;
#21095 = CARTESIAN_POINT ( 'NONE',  ( 47.18886224597662249, 22.92747281079970278, 45.29700218990083016 ) ) ;
#21096 = CARTESIAN_POINT ( 'NONE',  ( -42.66751614955960292, 15.14923148629343430, 38.44930799450052916 ) ) ;
#21097 = DIRECTION ( 'NONE',  ( -1.000000000000000000, 0.000000000000000000, -1.224646799147353207E-16 ) ) ;
#21098 = DIRECTION ( 'NONE',  ( -1.101824276508909887E-16, 1.000000000000000000, -0.000000000000000000 ) ) ;
#21099 = TOROIDAL_SURFACE ( 'NONE', #2765, 46.39830989763677849, 0.4000000000000020206 ) ;
#21100 = CARTESIAN_POINT ( 'NONE',  ( 21.09785597605719332, 25.76454579224779806, 47.04930799450051637 ) ) ;
#21101 = ORIENTED_EDGE ( 'NONE', *, *, #20844, .F. ) ;
#21102 = DIRECTION ( 'NONE',  ( -1.000000000000000000, 0.000000000000000000, 0.000000000000000000 ) ) ;
#21103 = CARTESIAN_POINT ( 'NONE',  ( -40.62121046050739892, 6.937850113510459771, 34.96172641100285716 ) ) ;
#21104 = CIRCLE ( 'NONE', #661, 0.1250000000000001110 ) ;
#21105 = ADVANCED_FACE ( 'NONE', ( #6320 ), #26087, .T. ) ;
#21106 = ORIENTED_EDGE ( 'NONE', *, *, #4826, .F. ) ;
#21107 = CARTESIAN_POINT ( 'NONE',  ( -42.03703168893574116, 3.954238390689463145, 47.04930799450051637 ) ) ;
#21108 = CARTESIAN_POINT ( 'NONE',  ( -39.58809650894544774, 2.596771453999702661, 45.84930799450051353 ) ) ;
#21109 = ORIENTED_EDGE ( 'NONE', *, *, #15587, .F. ) ;
#21110 = AXIS2_PLACEMENT_3D ( 'NONE', #7487, #2874, #14874 ) ;
#21111 = ORIENTED_EDGE ( 'NONE', *, *, #23430, .F. ) ;
#21112 = EDGE_CURVE ( 'NONE', #30194, #32106, #3693, .T. ) ;
#21113 = ORIENTED_EDGE ( 'NONE', *, *, #28074, .F. ) ;
#21114 = AXIS2_PLACEMENT_3D ( 'NONE', #8355, #8682, #20502 ) ;
#21115 = VERTEX_POINT ( 'NONE', #11100 ) ;
#21116 = CIRCLE ( 'NONE', #9615, 12.36707279061065101 ) ;
#21117 = CARTESIAN_POINT ( 'NONE',  ( -41.30594480120427647, 10.40086789971898895, 36.63067884439899302 ) ) ;
#21118 = ORIENTED_EDGE ( 'NONE', *, *, #15453, .T. ) ;
#21119 = CARTESIAN_POINT ( 'NONE',  ( 48.78406556707242459, 22.93807716476589675, 47.13688154746047587 ) ) ;
#21120 = CIRCLE ( 'NONE', #6992, 0.1000000000000008660 ) ;
#21121 = AXIS2_PLACEMENT_3D ( 'NONE', #26884, #21625, #4397 ) ;
#21122 = DIRECTION ( 'NONE',  ( -0.000000000000000000, -1.000000000000000000, 0.000000000000000000 ) ) ;
#21123 = DIRECTION ( 'NONE',  ( -1.000000000000000000, 0.000000000000000000, 0.000000000000000000 ) ) ;
#21124 = CARTESIAN_POINT ( 'NONE',  ( 46.99218062947583974, 27.15956182964376708, 49.08406571254116102 ) ) ;
#21125 = ORIENTED_EDGE ( 'NONE', *, *, #30401, .T. ) ;
#21126 = EDGE_LOOP ( 'NONE', ( #18013, #29909, #12362, #2020 ) ) ;
#21127 = FACE_OUTER_BOUND ( 'NONE', #25161, .T. ) ;
#21128 = ORIENTED_EDGE ( 'NONE', *, *, #20114, .T. ) ;
#21129 = CARTESIAN_POINT ( 'NONE',  ( -40.47677217214096146, 7.509199159542113478, 38.76965595547781618 ) ) ;
#21130 = DIRECTION ( 'NONE',  ( -0.2756373558169954996, 0.9612616959383198934, 8.751359879570023769E-15 ) ) ;
#21131 = DIRECTION ( 'NONE',  ( 0.000000000000000000, 0.000000000000000000, 1.000000000000000000 ) ) ;
#21132 = CARTESIAN_POINT ( 'NONE',  ( -1.514700296255377054, 11.69686719848734313, -5.042380923006707150 ) ) ;
#21133 = CARTESIAN_POINT ( 'NONE',  ( 21.09992658989238734, 38.56284415653841791, 47.04930799450051637 ) ) ;
#21134 = ORIENTED_EDGE ( 'NONE', *, *, #22890, .T. ) ;
#21135 = LINE ( 'NONE', #29347, #24456 ) ;
#21136 = CARTESIAN_POINT ( 'NONE',  ( -40.46271621608484281, 3.081581074246047436, 47.04930799450051637 ) ) ;
#21137 = CARTESIAN_POINT ( 'NONE',  ( -42.47434154250544225, 4.196643200812637531, 57.04930799450051637 ) ) ;
#21138 = CARTESIAN_POINT ( 'NONE',  ( 47.09785597605719687, 23.12036939723557083, 47.04930799450080059 ) ) ;
#21139 = DIRECTION ( 'NONE',  ( -1.101824276508909887E-16, 1.000000000000000000, -0.000000000000000000 ) ) ;
#21140 = CIRCLE ( 'NONE', #22728, 1.199999999999999734 ) ;
#21141 = VERTEX_POINT ( 'NONE', #3206 ) ;
#21142 = DIRECTION ( 'NONE',  ( -0.000000000000000000, -1.000000000000000000, 0.000000000000000000 ) ) ;
#21143 = EDGE_LOOP ( 'NONE', ( #23024, #26495 ) ) ;
#21144 = DIRECTION ( 'NONE',  ( -1.000000000000000000, 0.000000000000000000, 2.775557561562888984E-15 ) ) ;
#21145 = EDGE_CURVE ( 'NONE', #22098, #29646, #29781, .T. ) ;
#21146 = TOROIDAL_SURFACE ( 'NONE', #27963, 1.142135311067127068, 0.1000000000000000056 ) ;
#21147 = EDGE_LOOP ( 'NONE', ( #13990, #28142 ) ) ;
#21148 = ADVANCED_FACE ( 'NONE', ( #20611 ), #1460, .T. ) ;
#21149 = ADVANCED_FACE ( 'NONE', ( #16008 ), #31118, .F. ) ;
#21150 = EDGE_CURVE ( 'NONE', #6661, #27983, #21713, .T. ) ;
#21151 = CIRCLE ( 'NONE', #11728, 54.30000000000000426 ) ;
#21152 = EDGE_CURVE ( 'NONE', #4576, #27738, #906, .T. ) ;
#21153 = EDGE_LOOP ( 'NONE', ( #23148, #22741 ) ) ;
#21154 = DIRECTION ( 'NONE',  ( 0.000000000000000000, 1.000000000000000000, 0.000000000000000000 ) ) ;
#21155 = DIRECTION ( 'NONE',  ( 0.000000000000000000, 0.000000000000000000, -1.000000000000000000 ) ) ;
#21156 = CYLINDRICAL_SURFACE ( 'NONE', #14684, 12.36707279061065101 ) ;
#21157 = VERTEX_POINT ( 'NONE', #28808 ) ;
#21158 = AXIS2_PLACEMENT_3D ( 'NONE', #9032, #6899, #26272 ) ;
#21159 = CARTESIAN_POINT ( 'NONE',  ( -20.95081142018943510, -13.30632128221581389, 83.93193429851628196 ) ) ;
#21160 = CARTESIAN_POINT ( 'NONE',  ( -36.17322415754387066, 10.41998892282475531, 42.00358830701785706 ) ) ;
#21161 = CARTESIAN_POINT ( 'NONE',  ( 33.37634396954520355, 30.84164230456639544, 47.04930799450051637 ) ) ;
#21162 = VERTEX_POINT ( 'NONE', #20772 ) ;
#21163 = DIRECTION ( 'NONE',  ( -1.000000000000000000, 0.000000000000000000, 0.000000000000000000 ) ) ;
#21164 = ORIENTED_EDGE ( 'NONE', *, *, #30903, .T. ) ;
#21165 = DIRECTION ( 'NONE',  ( -3.551608010268815105E-15, 0.000000000000000000, 1.000000000000000000 ) ) ;
#21166 = CARTESIAN_POINT ( 'NONE',  ( 48.02750443086935661, 29.17693647873863583, 44.73249073240486240 ) ) ;
#21167 = CARTESIAN_POINT ( 'NONE',  ( -40.68533706394653393, 6.798065515868073838, 34.62231845625134241 ) ) ;
#21168 = ORIENTED_EDGE ( 'NONE', *, *, #9717, .F. ) ;
#21169 = EDGE_LOOP ( 'NONE', ( #27744, #7206, #1628, #23248 ) ) ;
#21170 = EDGE_CURVE ( 'NONE', #26283, #1375, #19259, .T. ) ;
#21171 = CARTESIAN_POINT ( 'NONE',  ( 24.75079866426202813, -13.30632128221581034, 102.8621610177830519 ) ) ;
#21172 = DIRECTION ( 'NONE',  ( -1.344306794811909066E-16, 1.000000000000000000, -1.759793992609925531E-18 ) ) ;
#21173 = CYLINDRICAL_SURFACE ( 'NONE', #30341, 12.36707279061065101 ) ;
#21174 = ORIENTED_EDGE ( 'NONE', *, *, #6448, .T. ) ;
#21175 = CARTESIAN_POINT ( 'NONE',  ( -39.64148344771002286, 7.657122216028891870, 61.94930799450052206 ) ) ;
#21176 = CARTESIAN_POINT ( 'NONE',  ( 21.09785597605719332, 39.33406896771847983, 47.04930799450051637 ) ) ;
#21177 = EDGE_LOOP ( 'NONE', ( #12886, #25406, #21111 ) ) ;
#21178 = DIRECTION ( 'NONE',  ( 0.000000000000000000, 0.000000000000000000, -1.000000000000000000 ) ) ;
#21179 = CARTESIAN_POINT ( 'NONE',  ( 48.73570333863616355, 28.52287913140503761, 44.52463952959527660 ) ) ;
#21180 = LINE ( 'NONE', #1661, #27449 ) ;
#21181 = EDGE_CURVE ( 'NONE', #30637, #28530, #20926, .T. ) ;
#21182 = CIRCLE ( 'NONE', #8616, 12.27641737965281976 ) ;
#21183 = EDGE_CURVE ( 'NONE', #5658, #3050, #1983, .T. ) ;
#21184 = AXIS2_PLACEMENT_3D ( 'NONE', #8865, #3947, #13966 ) ;
#21185 = VECTOR ( 'NONE', #9800, 1000.000000000000000 ) ;
#21186 = ADVANCED_FACE ( 'NONE', ( #28491 ), #13037, .F. ) ;
#21187 = AXIS2_PLACEMENT_3D ( 'NONE', #10629, #20620, #30646 ) ;
#21188 = TOROIDAL_SURFACE ( 'NONE', #16487, 1.899999999999999467, 0.1000000000000000056 ) ;
#21189 = AXIS2_PLACEMENT_3D ( 'NONE', #7084, #9552, #6920 ) ;
#21190 = EDGE_LOOP ( 'NONE', ( #3488, #12037 ) ) ;
#21191 = CARTESIAN_POINT ( 'NONE',  ( 21.09785597605719332, 44.06454579224779877, 47.04930799450051637 ) ) ;
#21192 = DIRECTION ( 'NONE',  ( 0.000000000000000000, 0.000000000000000000, -1.000000000000000000 ) ) ;
#21193 = CYLINDRICAL_SURFACE ( 'NONE', #23774, 0.1000000000000028644 ) ;
#21194 = ORIENTED_EDGE ( 'NONE', *, *, #226, .T. ) ;
#21195 = CARTESIAN_POINT ( 'NONE',  ( 21.09992658989239089, 29.84184655352422411, 47.04930799450051637 ) ) ;
#21196 = CARTESIAN_POINT ( 'NONE',  ( -40.10456357475989364, 7.631942973856654433, 60.14930799450051779 ) ) ;
#21197 = CARTESIAN_POINT ( 'NONE',  ( 21.09992658989238734, 32.55121380581068991, 47.04930799450051637 ) ) ;
#21198 = VERTEX_POINT ( 'NONE', #5632 ) ;
#21199 = DIRECTION ( 'NONE',  ( 0.6797146636928687036, 0.1949050434465272041, -0.7071067811865459074 ) ) ;
#21200 = LINE ( 'NONE', #18261, #7353 ) ;
#21201 = DIRECTION ( 'NONE',  ( 0.8746197071393926326, -0.4848096202463430537, -8.676864087101709653E-18 ) ) ;
#21202 = CARTESIAN_POINT ( 'NONE',  ( 21.09785597605718976, 7.237299147902269247, 27.58963108451947832 ) ) ;
#21203 = AXIS2_PLACEMENT_3D ( 'NONE', #12186, #22181, #27444 ) ;
#21204 =( LENGTH_UNIT ( ) NAMED_UNIT ( * ) SI_UNIT ( .MILLI., .METRE. ) );
#21205 = ORIENTED_EDGE ( 'NONE', *, *, #20482, .T. ) ;
#21206 = ADVANCED_FACE ( 'NONE', ( #18097 ), #15636, .T. ) ;
#21207 = CARTESIAN_POINT ( 'NONE',  ( 21.09785597605720753, 14.86454579224779948, 47.04930799450052348 ) ) ;
#21208 = CARTESIAN_POINT ( 'NONE',  ( 46.00908685603033632, 27.54624452788248590, 44.91496614357595263 ) ) ;
#21209 = CIRCLE ( 'NONE', #22282, 0.09999999999999904798 ) ;
#21210 = EDGE_CURVE ( 'NONE', #1803, #7874, #5151, .T. ) ;
#21211 = VECTOR ( 'NONE', #20251, 1000.000000000000000 ) ;
#21212 = DIRECTION ( 'NONE',  ( 0.000000000000000000, 0.000000000000000000, -1.000000000000000000 ) ) ;
#21213 = CARTESIAN_POINT ( 'NONE',  ( -40.11264481937005399, 6.813248423021981637, 34.63680500816278141 ) ) ;
#21214 = VECTOR ( 'NONE', #27885, 1000.000000000000000 ) ;
#21215 = DIRECTION ( 'NONE',  ( 0.000000000000000000, 0.000000000000000000, -1.000000000000000000 ) ) ;
#21216 = ORIENTED_EDGE ( 'NONE', *, *, #5594, .F. ) ;
#21217 = CARTESIAN_POINT ( 'NONE',  ( 48.39288112930642427, 29.59930898745696126, 45.41613349220816076 ) ) ;
#21218 = FACE_OUTER_BOUND ( 'NONE', #17460, .T. ) ;
#21219 = DIRECTION ( 'NONE',  ( 0.000000000000000000, -1.000000000000000000, 0.000000000000000000 ) ) ;
#21220 = ORIENTED_EDGE ( 'NONE', *, *, #21032, .T. ) ;
#21221 = CARTESIAN_POINT ( 'NONE',  ( 33.50134396954523908, 27.59164230456639544, 47.04930799450051637 ) ) ;
#21222 = CARTESIAN_POINT ( 'NONE',  ( 21.09992658989239089, 29.71183152705961561, 47.04930799450051637 ) ) ;
#21223 = DIRECTION ( 'NONE',  ( -1.101824276508909887E-16, 1.000000000000000000, -0.000000000000000000 ) ) ;
#21224 = CARTESIAN_POINT ( 'NONE',  ( 50.84778885652602298, 6.325917197325531482, -4.782011712722074925 ) ) ;
#21225 = ORIENTED_EDGE ( 'NONE', *, *, #16033, .F. ) ;
#21226 = DIRECTION ( 'NONE',  ( -1.000000000000000000, 0.000000000000000000, 0.000000000000000000 ) ) ;
#21227 = VERTEX_POINT ( 'NONE', #22866 ) ;
#21228 = EDGE_CURVE ( 'NONE', #460, #4539, #17726, .T. ) ;
#21229 = ORIENTED_EDGE ( 'NONE', *, *, #23311, .F. ) ;
#21230 = AXIS2_PLACEMENT_3D ( 'NONE', #25419, #3412, #10328 ) ;
#21231 =( BOUNDED_SURFACE ( )  B_SPLINE_SURFACE ( 3, 2, ( 
 ( #3817, #31242, #8589 ),
 ( #8902, #5973, #26465 ),
 ( #3334, #6283, #11369 ),
 ( #18904, #5813, #28607 ) ),
 .UNSPECIFIED., .F., .F., .F. ) 
 B_SPLINE_SURFACE_WITH_KNOTS ( ( 4, 4 ),
 ( 3, 3 ),
 ( 1.510941981261796796, 1.570796326794896558 ),
 ( 0.000000000000000000, 1.000000000000000000 ),
 .UNSPECIFIED. ) 
 GEOMETRIC_REPRESENTATION_ITEM ( )  RATIONAL_B_SPLINE_SURFACE ( (
 ( 1.000000000000000000, 0.7219065546282052992, 1.000000000000000000),
 ( 1.000000000000000000, 0.7170297040967862356, 1.000000000000000000),
 ( 1.000000000000000000, 0.7120946502353998619, 1.000000000000000000),
 ( 1.000000000000000000, 0.7071067811865515695, 1.000000000000000000) ) ) 
 REPRESENTATION_ITEM ( '' )  SURFACE ( )  );
#21232 = AXIS2_PLACEMENT_3D ( 'NONE', #9526, #14779, #14938 ) ;
#21233 = CIRCLE ( 'NONE', #20730, 12.62506659569710443 ) ;
#21234 = AXIS2_PLACEMENT_3D ( 'NONE', #20412, #28141, #5335 ) ;
#21235 = CIRCLE ( 'NONE', #1853, 0.1000000000000032530 ) ;
#21236 = ADVANCED_FACE ( 'NONE', ( #5478 ), #30838, .T. ) ;
#21237 = DIRECTION ( 'NONE',  ( 0.4848096202463673121, 0.8746197071393789768, 0.000000000000000000 ) ) ;
#21238 = CARTESIAN_POINT ( 'NONE',  ( -33.34250707380372347, -2.843755992669095622, 80.78322013955785508 ) ) ;
#21239 = CARTESIAN_POINT ( 'NONE',  ( 21.09785597605720753, 14.86454579224779948, 47.04930799450052348 ) ) ;
#21240 = ADVANCED_FACE ( 'NONE', ( #2520 ), #25494, .T. ) ;
#21241 = VECTOR ( 'NONE', #4747, 1000.000000000000000 ) ;
#21242 = VERTEX_POINT ( 'NONE', #7621 ) ;
#21243 = DIRECTION ( 'NONE',  ( -7.588956326749211550E-18, 4.206627182996911684E-18, -1.000000000000000000 ) ) ;
#21244 = EDGE_LOOP ( 'NONE', ( #31458, #11896 ) ) ;
#21245 = DIRECTION ( 'NONE',  ( 0.000000000000000000, 0.000000000000000000, -1.000000000000000000 ) ) ;
#21246 = DIRECTION ( 'NONE',  ( -0.000000000000000000, -1.000000000000000000, 0.000000000000000000 ) ) ;
#21247 = CARTESIAN_POINT ( 'NONE',  ( 33.46699938050304013, 38.56284415653841791, 47.04930799450051637 ) ) ;
#21248 = ORIENTED_EDGE ( 'NONE', *, *, #25008, .T. ) ;
#21249 = EDGE_CURVE ( 'NONE', #1796, #18652, #4636, .T. ) ;
#21250 = DIRECTION ( 'NONE',  ( 0.000000000000000000, 0.000000000000000000, -1.000000000000000000 ) ) ;
#21251 = DIRECTION ( 'NONE',  ( -1.000000000000000000, 0.000000000000000000, 0.000000000000000000 ) ) ;
#21252 = CARTESIAN_POINT ( 'NONE',  ( 21.09785597605719687, 25.13358275951983956, 86.68484420190863204 ) ) ;
#21253 = DIRECTION ( 'NONE',  ( -1.101824276508909887E-16, 1.000000000000000000, -0.000000000000000000 ) ) ;
#21254 = EDGE_CURVE ( 'NONE', #2086, #18205, #16152, .T. ) ;
#21255 = ORIENTED_EDGE ( 'NONE', *, *, #32291, .F. ) ;
#21256 = DIRECTION ( 'NONE',  ( 0.9612616959383193382, 0.2756373558169973870, 8.795445018804928853E-19 ) ) ;
#21257 = CARTESIAN_POINT ( 'NONE',  ( -4.902144023942810236, 25.56454579224779877, 49.54930799450078638 ) ) ;
#21258 = DIRECTION ( 'NONE',  ( -0.000000000000000000, -1.000000000000000000, -0.000000000000000000 ) ) ;
#21259 = DIRECTION ( 'NONE',  ( -1.101824276508909887E-16, 1.000000000000000000, -0.000000000000000000 ) ) ;
#21260 = EDGE_CURVE ( 'NONE', #7293, #26705, #26629, .T. ) ;
#21261 = CARTESIAN_POINT ( 'NONE',  ( 21.09992658989239089, 28.34164230456639544, 47.04930799450051637 ) ) ;
#21262 = EDGE_LOOP ( 'NONE', ( #20413, #8151, #15015, #22056 ) ) ;
#21263 = CARTESIAN_POINT ( 'NONE',  ( 53.59785597605720397, 13.86454579224779948, 47.04930799450051637 ) ) ;
#21264 = CARTESIAN_POINT ( 'NONE',  ( -40.63900869799031312, 6.896661531572857662, 34.99145992875370581 ) ) ;
#21265 = ORIENTED_EDGE ( 'NONE', *, *, #22934, .T. ) ;
#21266 = CARTESIAN_POINT ( 'NONE',  ( -43.80892580335221709, -4.771102634759627925, 41.87060378362927793 ) ) ;
#21267 = CIRCLE ( 'NONE', #18642, 12.36707279061065101 ) ;
#21268 = AXIS2_PLACEMENT_3D ( 'NONE', #4594, #16902, #1478 ) ;
#21269 = CARTESIAN_POINT ( 'NONE',  ( -4.902144023942810236, 30.56554579224779644, 49.54930799450042400 ) ) ;
#21270 = ORIENTED_EDGE ( 'NONE', *, *, #17818, .F. ) ;
#21271 = ORIENTED_EDGE ( 'NONE', *, *, #6116, .T. ) ;
#21272 = ADVANCED_FACE ( 'NONE', ( #10571 ), #28213, .T. ) ;
#21273 = AXIS2_PLACEMENT_3D ( 'NONE', #2372, #22713, #24692 ) ;
#21274 = ORIENTED_EDGE ( 'NONE', *, *, #913, .T. ) ;
#21275 = ORIENTED_EDGE ( 'NONE', *, *, #14449, .F. ) ;
#21276 = EDGE_CURVE ( 'NONE', #12487, #25630, #14595, .T. ) ;
#21277 = DIRECTION ( 'NONE',  ( -1.000000000000000000, 0.000000000000000000, 0.000000000000000000 ) ) ;
#21278 = AXIS2_PLACEMENT_3D ( 'NONE', #13010, #515, #6094 ) ;
#21279 = ADVANCED_FACE ( 'NONE', ( #23020 ), #9344, .T. ) ;
#21280 = VERTEX_POINT ( 'NONE', #2689 ) ;
#21281 = CARTESIAN_POINT ( 'NONE',  ( 47.37889090789306579, 23.12036939723557083, 47.06390358666074292 ) ) ;
#21282 = LINE ( 'NONE', #31315, #9729 ) ;
#21283 = DIRECTION ( 'NONE',  ( 0.000000000000000000, 0.000000000000000000, -1.000000000000000000 ) ) ;
#21284 = CARTESIAN_POINT ( 'NONE',  ( 48.16694854572211426, 29.36119643316632022, 49.14507740233662503 ) ) ;
#21285 = EDGE_LOOP ( 'NONE', ( #21371, #9924, #13337, #13151 ) ) ;
#21286 = VERTEX_POINT ( 'NONE', #32404 ) ;
#21287 = DIRECTION ( 'NONE',  ( -1.101824276508909887E-16, 1.000000000000000000, -0.000000000000000000 ) ) ;
#21288 = ADVANCED_FACE ( 'NONE', ( #28125 ), #17459, .T. ) ;
#21289 = ORIENTED_EDGE ( 'NONE', *, *, #22096, .F. ) ;
#21290 = DIRECTION ( 'NONE',  ( -1.000000000000000000, -1.101824276508910010E-16, 0.000000000000000000 ) ) ;
#21291 = AXIS2_PLACEMENT_3D ( 'NONE', #17936, #22861, #12870 ) ;
#21292 = CYLINDRICAL_SURFACE ( 'NONE', #4204, 0.1000000000000014905 ) ;
#21293 = CARTESIAN_POINT ( 'NONE',  ( -41.23380787120766655, 11.23768311167744294, 37.04930799450052348 ) ) ;
#21294 = DIRECTION ( 'NONE',  ( -0.000000000000000000, -1.000000000000000000, -0.000000000000000000 ) ) ;
#21295 = CARTESIAN_POINT ( 'NONE',  ( 52.94504501510867556, -5.721341737285968065, -11.26059709029990330 ) ) ;
#21296 = FACE_OUTER_BOUND ( 'NONE', #12099, .T. ) ;
#21297 = ORIENTED_EDGE ( 'NONE', *, *, #12460, .F. ) ;
#21298 = CARTESIAN_POINT ( 'NONE',  ( -42.41019933908752648, 14.71530103803245915, 60.54930799450051637 ) ) ;
#21299 = CARTESIAN_POINT ( 'NONE',  ( -40.09211399732166115, 9.667069410243957606, 34.64930799450051779 ) ) ;
#21300 = DIRECTION ( 'NONE',  ( -0.000000000000000000, 1.000000000000000000, -0.000000000000000000 ) ) ;
#21301 = DIRECTION ( 'NONE',  ( 1.000000000000000000, 0.000000000000000000, 0.000000000000000000 ) ) ;
#21302 = DIRECTION ( 'NONE',  ( -1.000000000000000000, -1.101824276508909887E-16, 0.000000000000000000 ) ) ;
#21303 = ORIENTED_EDGE ( 'NONE', *, *, #14764, .T. ) ;
#21304 = CARTESIAN_POINT ( 'NONE',  ( -43.43257085947613660, 1.024086014757300767, 60.44930799450051495 ) ) ;
#21305 = ORIENTED_EDGE ( 'NONE', *, *, #3576, .F. ) ;
#21306 = DIRECTION ( 'NONE',  ( -1.000000000000000000, 0.000000000000000000, 0.000000000000000000 ) ) ;
#21307 = CARTESIAN_POINT ( 'NONE',  ( 8.482002859293437780, 27.96664230456639899, 47.04930799450051637 ) ) ;
#21308 = CIRCLE ( 'NONE', #30232, 0.1000000000000018235 ) ;
#21309 = ORIENTED_EDGE ( 'NONE', *, *, #27022, .F. ) ;
#21310 = CIRCLE ( 'NONE', #296, 31.30000000000002913 ) ;
#21311 = VERTEX_POINT ( 'NONE', #10248 ) ;
#21312 = CARTESIAN_POINT ( 'NONE',  ( 33.46699938050304013, 26.21183152705960140, 47.04930799450051637 ) ) ;
#21313 = CARTESIAN_POINT ( 'NONE',  ( -40.16174044770769314, 7.468546898574136783, 53.64930799450051779 ) ) ;
#21314 = DIRECTION ( 'NONE',  ( -0.000000000000000000, -1.000000000000000000, -0.000000000000000000 ) ) ;
#21315 = ORIENTED_EDGE ( 'NONE', *, *, #31062, .F. ) ;
#21316 = DIRECTION ( 'NONE',  ( -1.000000000000000000, 0.000000000000000000, 0.000000000000000000 ) ) ;
#21317 = DIRECTION ( 'NONE',  ( -1.188208965918165239E-16, -1.880121038077812639E-16, -1.000000000000000000 ) ) ;
#21318 = CARTESIAN_POINT ( 'NONE',  ( 72.45827002609743772, 9.438446991585321300, 20.02200133371455593 ) ) ;
#21319 = AXIS2_PLACEMENT_3D ( 'NONE', #1365, #25834, #882 ) ;
#21320 = ORIENTED_EDGE ( 'NONE', *, *, #21360, .F. ) ;
#21321 = CARTESIAN_POINT ( 'NONE',  ( -40.57832940339291383, 7.446916344587776848, 60.54930799450051637 ) ) ;
#21322 = EDGE_CURVE ( 'NONE', #18056, #26091, #30332, .T. ) ;
#21323 = EDGE_LOOP ( 'NONE', ( #19970, #16972, #2843, #20120 ) ) ;
#21324 = CARTESIAN_POINT ( 'NONE',  ( 21.09785597605720042, -13.59284023713420630, -8.674624342367264873 ) ) ;
#21325 = FACE_OUTER_BOUND ( 'NONE', #2035, .T. ) ;
#21326 = ADVANCED_FACE ( 'NONE', ( #5323 ), #8294, .T. ) ;
#21327 = CARTESIAN_POINT ( 'NONE',  ( -40.41647043964083252, 8.356895951721261540, 59.54930799450050927 ) ) ;
#21328 = EDGE_LOOP ( 'NONE', ( #26193, #19171, #27811, #19478 ) ) ;
#21329 = ORIENTED_EDGE ( 'NONE', *, *, #28793, .T. ) ;
#21330 = CARTESIAN_POINT ( 'NONE',  ( -40.78929413070552101, 0.6853368522271082730, 52.04930799450050927 ) ) ;
#21331 = CARTESIAN_POINT ( 'NONE',  ( 21.09785597605719332, -13.49020584019834601, 47.04930799450051637 ) ) ;
#21332 = CARTESIAN_POINT ( 'NONE',  ( 48.10030433005226769, 29.45850404830353142, 49.01443330185325920 ) ) ;
#21333 = ORIENTED_EDGE ( 'NONE', *, *, #7122, .F. ) ;
#21334 = DIRECTION ( 'NONE',  ( -0.000000000000000000, 1.000000000000000000, -0.000000000000000000 ) ) ;
#21335 = CARTESIAN_POINT ( 'NONE',  ( 73.43141673955736337, -13.74047052604243646, 21.24731629327111193 ) ) ;
#21336 = ORIENTED_EDGE ( 'NONE', *, *, #3852, .F. ) ;
#21337 = CARTESIAN_POINT ( 'NONE',  ( -40.50841487316075273, 7.574651041938937013, 60.23716689141008374 ) ) ;
#21338 = CARTESIAN_POINT ( 'NONE',  ( 45.46000861347822308, 26.77287913140504116, 49.57397645940629616 ) ) ;
#21339 = FACE_OUTER_BOUND ( 'NONE', #12953, .T. ) ;
#21340 = CIRCLE ( 'NONE', #12459, 12.62506659569710266 ) ;
#21341 = CIRCLE ( 'NONE', #14033, 12.50000000000001776 ) ;
#21342 = VERTEX_POINT ( 'NONE', #2841 ) ;
#21343 = AXIS2_PLACEMENT_3D ( 'NONE', #28776, #13528, #10906 ) ;
#21344 = CYLINDRICAL_SURFACE ( 'NONE', #9295, 12.36707279061065101 ) ;
#21345 = CARTESIAN_POINT ( 'NONE',  ( 21.09992658989238734, 38.56284415653841791, 47.04930799450051637 ) ) ;
#21346 = FACE_OUTER_BOUND ( 'NONE', #25833, .T. ) ;
#21347 = CARTESIAN_POINT ( 'NONE',  ( 48.83862994770794330, 28.74118040159426002, 48.17861352429476796 ) ) ;
#21348 = AXIS2_PLACEMENT_3D ( 'NONE', #7625, #23026, #27318 ) ;
#21349 = ORIENTED_EDGE ( 'NONE', *, *, #22971, .T. ) ;
#21350 = DIRECTION ( 'NONE',  ( -0.2756373558169956106, 0.9612616959383197823, 0.000000000000000000 ) ) ;
#21351 = DIRECTION ( 'NONE',  ( -1.000000000000000000, 0.000000000000000000, 0.000000000000000000 ) ) ;
#21352 = CARTESIAN_POINT ( 'NONE',  ( 71.95763425453002071, 6.496515553941713428, 17.40581666385103077 ) ) ;
#21353 = CARTESIAN_POINT ( 'NONE',  ( 47.63716429968717136, 26.79696019071911195, 49.58068632438585155 ) ) ;
#21354 = ADVANCED_FACE ( 'NONE', ( #11203 ), #27170, .F. ) ;
#21355 = CARTESIAN_POINT ( 'NONE',  ( 21.09785597605720753, 13.66454579224780019, 47.04930799450052348 ) ) ;
#21357 = EDGE_CURVE ( 'NONE', #25631, #7606, #15114, .T. ) ;
#21356 = LINE ( 'NONE', #29249, #4738 ) ;
#21358 = EDGE_CURVE ( 'NONE', #27840, #26531, #10923, .T. ) ;
#21359 = FACE_OUTER_BOUND ( 'NONE', #13960, .T. ) ;
#21360 = EDGE_CURVE ( 'NONE', #17357, #3287, #31231, .T. ) ;
#21361 = CARTESIAN_POINT ( 'NONE',  ( -40.57832940339291383, 7.446916344587776848, 60.23882281530426042 ) ) ;
#21362 = EDGE_LOOP ( 'NONE', ( #26400, #9091, #8959, #14908 ) ) ;
#21363 = CARTESIAN_POINT ( 'NONE',  ( 21.09992658989239089, 26.09184655352419213, 47.04930799450051637 ) ) ;
#21365 = CARTESIAN_POINT ( 'NONE',  ( 45.35708200440645044, 27.60457786121581947, 45.92000246470680480 ) ) ;
#21364 = CIRCLE ( 'NONE', #9324, 2.500000000000002220 ) ;
#21366 = AXIS2_PLACEMENT_3D ( 'NONE', #4046, #14072, #11768 ) ;
#21367 = CARTESIAN_POINT ( 'NONE',  ( -40.38222711384413088, 8.611297240477076897, 34.61707255558062002 ) ) ;
#21368 = CARTESIAN_POINT ( 'NONE',  ( 3.597855976057204419, 14.86454579224779948, 47.04930799450052348 ) ) ;
#21369 = AXIS2_PLACEMENT_3D ( 'NONE', #23174, #2824, #30407 ) ;
#21370 = CARTESIAN_POINT ( 'NONE',  ( 21.09785597605719687, 47.94190058235918173, 66.23928994759033628 ) ) ;
#21371 = ORIENTED_EDGE ( 'NONE', *, *, #11433, .F. ) ;
#21372 = DIRECTION ( 'NONE',  ( -1.000000000000000000, 0.000000000000000000, 0.000000000000000000 ) ) ;
#21373 = CARTESIAN_POINT ( 'NONE',  ( 8.474859994195286461, 25.09184655352419213, 47.04930799450051637 ) ) ;
#21374 = DIRECTION ( 'NONE',  ( -2.779292025043186357E-18, 1.288349127009862211E-17, -1.000000000000000000 ) ) ;
#21375 = AXIS2_PLACEMENT_3D ( 'NONE', #16383, #6699, #6871 ) ;
#21376 = ORIENTED_EDGE ( 'NONE', *, *, #29026, .T. ) ;
#21377 = LINE ( 'NONE', #31417, #27790 ) ;
#21378 = DIRECTION ( 'NONE',  ( -0.000000000000000000, -1.000000000000000000, 0.000000000000000000 ) ) ;
#21379 = DIRECTION ( 'NONE',  ( -0.9612616959383202264, -0.2756373558169947779, 3.659346610729174208E-19 ) ) ;
#21380 = AXIS2_PLACEMENT_3D ( 'NONE', #3649, #716, #13204 ) ;
#21381 = DIRECTION ( 'NONE',  ( -1.000000000000000000, 0.000000000000000000, 0.000000000000000000 ) ) ;
#21382 = ORIENTED_EDGE ( 'NONE', *, *, #24984, .F. ) ;
#21383 = CARTESIAN_POINT ( 'NONE',  ( -40.52064652407315748, 7.631814549704944106, 60.17616479600645363 ) ) ;
#21384 = ORIENTED_EDGE ( 'NONE', *, *, #23632, .F. ) ;
#21385 = VERTEX_POINT ( 'NONE', #31070 ) ;
#21386 = ADVANCED_FACE ( 'NONE', ( #8730 ), #13544, .T. ) ;
#21387 = ADVANCED_FACE ( 'NONE', ( #5800 ), #28756, .T. ) ;
#21388 = AXIS2_PLACEMENT_3D ( 'NONE', #24439, #31831, #17051 ) ;
#21389 = AXIS2_PLACEMENT_3D ( 'NONE', #17566, #20344, #4940 ) ;
#21390 = VECTOR ( 'NONE', #29224, 1000.000000000000114 ) ;
#21391 = AXIS2_PLACEMENT_3D ( 'NONE', #13271, #20794, #30817 ) ;
#21392 = CARTESIAN_POINT ( 'NONE',  ( 33.72499318558949710, 24.59143805560860940, 47.04930799450051637 ) ) ;
#21393 = CARTESIAN_POINT ( 'NONE',  ( 21.09992658989238734, 38.56284415653841791, 47.04930799450051637 ) ) ;
#21394 = DIRECTION ( 'NONE',  ( -1.101824276508909887E-16, 1.000000000000000000, -0.000000000000000000 ) ) ;
#21395 = VERTEX_POINT ( 'NONE', #1022 ) ;
#21396 = AXIS2_PLACEMENT_3D ( 'NONE', #17069, #12493, #29888 ) ;
#21397 = DIRECTION ( 'NONE',  ( 0.000000000000000000, 0.000000000000000000, 1.000000000000000000 ) ) ;
#21398 = ORIENTED_EDGE ( 'NONE', *, *, #8992, .T. ) ;
#21399 = DIRECTION ( 'NONE',  ( -0.000000000000000000, -1.000000000000000000, 0.000000000000000000 ) ) ;
#21400 = SURFACE_STYLE_USAGE ( .BOTH. , #1721 ) ;
#21401 = EDGE_CURVE ( 'NONE', #17692, #21567, #4085, .T. ) ;
#21402 = ORIENTED_EDGE ( 'NONE', *, *, #27994, .T. ) ;
#21403 = DIRECTION ( 'NONE',  ( -1.224646799147353207E-16, -1.349345573449484691E-32, 1.000000000000000000 ) ) ;
#21404 = CYLINDRICAL_SURFACE ( 'NONE', #30496, 12.36707279061065279 ) ;
#21405 = FACE_BOUND ( 'NONE', #15241, .T. ) ;
#21406 = CARTESIAN_POINT ( 'NONE',  ( -42.36691375901575185, 13.72999064396537250, 59.48380644099231773 ) ) ;
#21407 = ORIENTED_EDGE ( 'NONE', *, *, #7537, .T. ) ;
#21408 = CARTESIAN_POINT ( 'NONE',  ( 47.32587910665017006, 22.95310733321322516, 45.42502988274431175 ) ) ;
#21409 = FACE_OUTER_BOUND ( 'NONE', #26583, .T. ) ;
#21410 = DIRECTION ( 'NONE',  ( 0.000000000000000000, 1.450913048936738450E-16, -1.000000000000000000 ) ) ;
#21411 = DIRECTION ( 'NONE',  ( -0.000000000000000000, -1.000000000000000000, 0.000000000000000000 ) ) ;
#21412 = CARTESIAN_POINT ( 'NONE',  ( -42.36691375901575185, 13.72999064396537250, 54.61480954800870791 ) ) ;
#21413 = ORIENTED_EDGE ( 'NONE', *, *, #17649, .F. ) ;
#21414 = CARTESIAN_POINT ( 'NONE',  ( -40.01477201457416299, 7.207664580858174297, 35.09860252446828355 ) ) ;
#21415 = DIRECTION ( 'NONE',  ( -0.8746197071393823075, 0.4848096202463614279, 0.000000000000000000 ) ) ;
#21416 = ORIENTED_EDGE ( 'NONE', *, *, #19337, .T. ) ;
#21417 = CARTESIAN_POINT ( 'NONE',  ( -44.22750734272732132, -5.641423040791120336, 41.10178114657359316 ) ) ;
#21418 = CIRCLE ( 'NONE', #9916, 31.29999999999997229 ) ;
#21419 = AXIS2_PLACEMENT_3D ( 'NONE', #9178, #25206, #26896 ) ;
#21420 = CARTESIAN_POINT ( 'NONE',  ( -22.40214402394279247, 13.86454579224779948, 47.04930799450052348 ) ) ;
#21421 = CIRCLE ( 'NONE', #4585, 0.1249999999999983763 ) ;
#21422 = ORIENTED_EDGE ( 'NONE', *, *, #13181, .T. ) ;
#21423 = SHAPE_REPRESENTATION ( 'Membrane', ( #8172 ), #824 ) ;
#21424 = EDGE_CURVE ( 'NONE', #16313, #8568, #13830, .T. ) ;
#21425 = ORIENTED_EDGE ( 'NONE', *, *, #20380, .T. ) ;
#21426 = EDGE_CURVE ( 'NONE', #2250, #24311, #19288, .T. ) ;
#21427 = AXIS2_PLACEMENT_3D ( 'NONE', #16065, #6550, #16543 ) ;
#21428 = VERTEX_POINT ( 'NONE', #10887 ) ;
#21429 = VECTOR ( 'NONE', #23942, 1000.000000000000227 ) ;
#21430 = ADVANCED_FACE ( 'NONE', ( #11358 ), #3643, .F. ) ;
#21431 = EDGE_CURVE ( 'NONE', #11560, #22567, #28364, .T. ) ;
#21432 = EDGE_CURVE ( 'NONE', #10697, #17732, #13198, .T. ) ;
#21433 = CARTESIAN_POINT ( 'NONE',  ( -41.92347351173192749, 13.84990507184044084, 54.57160570446790615 ) ) ;
#21434 =( REPRESENTATION_RELATIONSHIP ('NONE','NONE', #20382, #5723 ) REPRESENTATION_RELATIONSHIP_WITH_TRANSFORMATION ( #3585 )SHAPE_REPRESENTATION_RELATIONSHIP( ) );
#21435 = AXIS2_PLACEMENT_3D ( 'NONE', #31474, #27028, #14076 ) ;
#21436 = VECTOR ( 'NONE', #4983, 1000.000000000000000 ) ;
#21437 = VERTEX_POINT ( 'NONE', #23674 ) ;
#21438 = DIRECTION ( 'NONE',  ( -1.101824276508909887E-16, 1.000000000000000000, -0.000000000000000000 ) ) ;
#21439 = LINE ( 'NONE', #26380, #13090 ) ;
#21440 = DIRECTION ( 'NONE',  ( -0.000000000000000000, -1.000000000000000000, 0.000000000000000000 ) ) ;
#21441 = CARTESIAN_POINT ( 'NONE',  ( 21.09785597605719332, 12.74140866975414887, 47.04930799450051637 ) ) ;
#21442 = CARTESIAN_POINT ( 'NONE',  ( 45.28286642839709231, 28.48619643316631311, 47.97516931882780966 ) ) ;
#21443 = EDGE_CURVE ( 'NONE', #15900, #12078, #7782, .T. ) ;
#21444 = ORIENTED_EDGE ( 'NONE', *, *, #29648, .T. ) ;
#21445 = ORIENTED_EDGE ( 'NONE', *, *, #18427, .T. ) ;
#21446 = CARTESIAN_POINT ( 'NONE',  ( -11.94738134238030014, -4.768257113790713042, -9.054433584172935312 ) ) ;
#21447 = ORIENTED_EDGE ( 'NONE', *, *, #18189, .F. ) ;
#21448 = CARTESIAN_POINT ( 'NONE',  ( 48.81899109467476450, 29.57820558303529168, 45.85849491930559196 ) ) ;
#21449 = CIRCLE ( 'NONE', #26198, 12.27641737965285174 ) ;
#21450 = CARTESIAN_POINT ( 'NONE',  ( -40.46704362897429519, 7.411062716778913817, 38.79847704167570299 ) ) ;
#21451 = FACE_OUTER_BOUND ( 'NONE', #13707, .T. ) ;
#21452 = CARTESIAN_POINT ( 'NONE',  ( -39.58809650894544774, 2.596771453999702661, 47.04930799450051637 ) ) ;
#21453 = CARTESIAN_POINT ( 'NONE',  ( 46.96268396749378127, 28.23121246473837331, 49.65201805493727960 ) ) ;
#21454 = AXIS2_PLACEMENT_3D ( 'NONE', #29194, #26895, #4566 ) ;
#21455 = CARTESIAN_POINT ( 'NONE',  ( 46.46324171377475665, 22.99884124225578574, 48.31483337462398708 ) ) ;
#21456 = CARTESIAN_POINT ( 'NONE',  ( -40.60251150970604073, 6.748447833883063574, 53.64930799450051779 ) ) ;
#21457 = ORIENTED_EDGE ( 'NONE', *, *, #22818, .F. ) ;
#21458 = CARTESIAN_POINT ( 'NONE',  ( 21.09992658989239089, 25.09164230456639899, 47.04930799450051637 ) ) ;
#21459 = DIRECTION ( 'NONE',  ( 0.000000000000000000, 0.000000000000000000, 1.000000000000000000 ) ) ;
#21460 = CYLINDRICAL_SURFACE ( 'NONE', #26209, 0.7928932188134565351 ) ;
#21461 = DIRECTION ( 'NONE',  ( 0.1949050434465275650, -0.6797146636928697028, 0.7071067811865449082 ) ) ;
#21462 = EDGE_LOOP ( 'NONE', ( #13972, #18869, #29440, #11013 ) ) ;
#21463 = CARTESIAN_POINT ( 'NONE',  ( 8.474859994195286461, 30.59184655352422411, 47.04930799450051637 ) ) ;
#21464 = ADVANCED_FACE ( 'NONE', ( #15957 ), #25965, .F. ) ;
#21465 = ORIENTED_EDGE ( 'NONE', *, *, #20041, .F. ) ;
#21466 = CARTESIAN_POINT ( 'NONE',  ( -34.31970563170438737, 11.92558985988973674, 40.04930799450050216 ) ) ;
#21467 = CARTESIAN_POINT ( 'NONE',  ( 41.51205063648687599, 11.92558985988973497, 99.90211174246701376 ) ) ;
#21468 = CIRCLE ( 'NONE', #7330, 0.1000000000000002137 ) ;
#21469 = ADVANCED_FACE ( 'NONE', ( #29080 ), #7249, .F. ) ;
#21470 = ORIENTED_EDGE ( 'NONE', *, *, #27314, .T. ) ;
#21471 = ADVANCED_FACE ( 'NONE', ( #1832 ), #15955, .T. ) ;
#21472 = AXIS2_PLACEMENT_3D ( 'NONE', #19695, #12330, #14792 ) ;
#21473 = AXIS2_PLACEMENT_3D ( 'NONE', #15442, #13155, #6079 ) ;
#21474 = EDGE_CURVE ( 'NONE', #5096, #25136, #26613, .T. ) ;
#21475 = CIRCLE ( 'NONE', #19918, 0.1249999999999983763 ) ;
#21476 = EDGE_LOOP ( 'NONE', ( #6199, #7813, #3153, #19799, #28393, #28386, #5798 ) ) ;
#21477 = AXIS2_PLACEMENT_3D ( 'NONE', #439, #10636, #10467 ) ;
#21478 = CARTESIAN_POINT ( 'NONE',  ( 8.698509210239521394, 25.59164230456639899, 47.04930799450051637 ) ) ;
#21479 = TOROIDAL_SURFACE ( 'NONE', #20974, 78.39999999999999147, 0.1000000000000014350 ) ;
#21480 = DIRECTION ( 'NONE',  ( -1.000000000000000000, 0.000000000000000000, 0.000000000000000000 ) ) ;
#21481 = VERTEX_POINT ( 'NONE', #22003 ) ;
#21482 = CARTESIAN_POINT ( 'NONE',  ( 49.40414881150629611, 19.96454579224779380, 47.16908566558144855 ) ) ;
#21483 = DIRECTION ( 'NONE',  ( -1.000000000000000000, 0.000000000000000000, 0.000000000000000000 ) ) ;
#21484 = CARTESIAN_POINT ( 'NONE',  ( 72.54327431645151592, 8.281585831149239851, 18.82624325624167838 ) ) ;
#21485 = ORIENTED_EDGE ( 'NONE', *, *, #32178, .T. ) ;
#21486 =( LENGTH_UNIT ( ) NAMED_UNIT ( * ) SI_UNIT ( .MILLI., .METRE. ) );
#21487 = VECTOR ( 'NONE', #19558, 1000.000000000000227 ) ;
#21488 = ORIENTED_EDGE ( 'NONE', *, *, #1617, .F. ) ;
#21489 = SPHERICAL_SURFACE ( 'NONE', #25957, 36.51080762834750715 ) ;
#21490 = CARTESIAN_POINT ( 'NONE',  ( 21.09992658989239089, 24.84184655352419213, 47.04930799450051637 ) ) ;
#21491 = CARTESIAN_POINT ( 'NONE',  ( -43.37834615508418068, 1.121909970995877082, 39.44930799450052916 ) ) ;
#21492 = DIRECTION ( 'NONE',  ( 0.9820818503191365290, -1.249000902703301108E-16, -0.1884548733085490424 ) ) ;
#21493 = ORIENTED_EDGE ( 'NONE', *, *, #29944, .T. ) ;
#21494 = ORIENTED_EDGE ( 'NONE', *, *, #2228, .F. ) ;
#21495 = DIRECTION ( 'NONE',  ( -1.101824276508909887E-16, 1.000000000000000000, -0.000000000000000000 ) ) ;
#21496 = CIRCLE ( 'NONE', #18873, 58.70143199044622406 ) ;
#21497 = FACE_OUTER_BOUND ( 'NONE', #24009, .T. ) ;
#21498 = EDGE_LOOP ( 'NONE', ( #23616, #24375, #23777, #26454 ) ) ;
#21499 = CARTESIAN_POINT ( 'NONE',  ( -12.43099670031970838, -1.035104995753983959, -7.280064108657495758 ) ) ;
#21500 = VECTOR ( 'NONE', #30532, 1000.000000000000000 ) ;
#21501 = DIRECTION ( 'NONE',  ( 0.1949050434465252057, -0.6797146636928670382, 0.7071067811865481278 ) ) ;
#21502 = ORIENTED_EDGE ( 'NONE', *, *, #24893, .F. ) ;
#21503 = FACE_OUTER_BOUND ( 'NONE', #19725, .T. ) ;
#21504 = B_SPLINE_CURVE_WITH_KNOTS ( 'NONE', 3,
 ( #7113, #29936, #19578, #19904, #6786, #14997, #16788, #29602, #24674, #31898, #2191, #17277, #26810, #29764, #25002, #21871, #26967, #4326, #24336 ),
 .UNSPECIFIED., .F., .F.,
 ( 4, 3, 3, 3, 3, 3, 4 ),
 ( 3.237246860597884355E-16, 2.715504454938324236E-05, 5.405723342089737831E-05, 9.254577804459618708E-05, 0.0001429137362853355627, 0.0001870166610891571849, 0.0001891372738450128029 ),
 .UNSPECIFIED. ) ;
#21505 = CIRCLE ( 'NONE', #5790, 2.800000000000002043 ) ;
#21506 = CARTESIAN_POINT ( 'NONE',  ( 49.28428300279882990, 29.74787913140503903, 48.46772541801551171 ) ) ;
#21507 = CIRCLE ( 'NONE', #24063, 0.1250000000000001110 ) ;
#21508 = CARTESIAN_POINT ( 'NONE',  ( -40.65762574042817334, 9.591092754368339968, 38.50788663826321567 ) ) ;
#21509 = AXIS2_PLACEMENT_3D ( 'NONE', #10216, #13005, #22837 ) ;
#21510 = ADVANCED_FACE ( 'NONE', ( #14150 ), #32034, .T. ) ;
#21511 = ORIENTED_EDGE ( 'NONE', *, *, #3073, .F. ) ;
#21512 = EDGE_CURVE ( 'NONE', #16648, #15550, #5498, .T. ) ;
#21513 = EDGE_CURVE ( 'NONE', #13855, #19482, #28040, .T. ) ;
#21514 = DIRECTION ( 'NONE',  ( -1.000000000000000000, 0.000000000000000000, 0.000000000000000000 ) ) ;
#21515 = FACE_OUTER_BOUND ( 'NONE', #4036, .T. ) ;
#21516 = DIRECTION ( 'NONE',  ( -0.2743622330404219545, 0.9568148143496242319, -0.09607692814701952744 ) ) ;
#21517 = CARTESIAN_POINT ( 'NONE',  ( 47.20547626766766314, 28.97451373492759075, 44.97710074790751378 ) ) ;
#21518 = AXIS2_PLACEMENT_3D ( 'NONE', #29797, #27330, #5017 ) ;
#21519 = EDGE_LOOP ( 'NONE', ( #7823, #27119, #6827, #23728 ) ) ;
#21520 = AXIS2_PLACEMENT_3D ( 'NONE', #18161, #18006, #31139 ) ;
#21521 = CARTESIAN_POINT ( 'NONE',  ( 21.09785597605719332, 30.56454579224779522, 21.04930799450051282 ) ) ;
#21522 = DIRECTION ( 'NONE',  ( -1.101824276508909887E-16, 1.000000000000000000, -0.000000000000000000 ) ) ;
#21523 = AXIS2_PLACEMENT_3D ( 'NONE', #24207, #3863, #1228 ) ;
#21524 = FACE_BOUND ( 'NONE', #12123, .T. ) ;
#21525 = CARTESIAN_POINT ( 'NONE',  ( -40.02540636251514172, 2.839176264122877047, 57.04930799450051637 ) ) ;
#21526 = CARTESIAN_POINT ( 'NONE',  ( 8.732853799281734553, 38.56284415653841791, 47.04930799450051637 ) ) ;
#21527 = CARTESIAN_POINT ( 'NONE',  ( -22.76726271559795478, -13.74047052604243646, 8.573397087749011547 ) ) ;
#21528 = CARTESIAN_POINT ( 'NONE',  ( 8.474859994195286461, 29.59143805560861296, 47.04930799450051637 ) ) ;
#21529 = DIRECTION ( 'NONE',  ( -1.000000000000000000, 0.000000000000000000, 0.000000000000000000 ) ) ;
#21530 = ORIENTED_EDGE ( 'NONE', *, *, #4528, .F. ) ;
#21531 = CARTESIAN_POINT ( 'NONE',  ( 45.42003181263716272, 22.93807716476589675, 46.80027486889689214 ) ) ;
#21532 = CARTESIAN_POINT ( 'NONE',  ( 48.18662509608405742, 25.79624452788248945, 49.18364984542562013 ) ) ;
#21533 = VECTOR ( 'NONE', #1870, 1000.000000000000000 ) ;
#21534 = CARTESIAN_POINT ( 'NONE',  ( 8.474859994195282908, 38.56284415653841791, 47.04930799450051637 ) ) ;
#21535 = CARTESIAN_POINT ( 'NONE',  ( -18.40214402394279603, 14.86454579224779948, 47.04930799450052348 ) ) ;
#21536 = DIRECTION ( 'NONE',  ( -1.000000000000000000, 0.000000000000000000, 0.000000000000000000 ) ) ;
#21537 = ORIENTED_EDGE ( 'NONE', *, *, #32028, .T. ) ;
#21538 = CARTESIAN_POINT ( 'NONE',  ( -39.56789013741062178, -5.936135285505173442, 77.93152707003946489 ) ) ;
#21539 = CARTESIAN_POINT ( 'NONE',  ( 21.09992658989238734, 38.56284415653841791, 47.04930799450051637 ) ) ;
#21540 = DIRECTION ( 'NONE',  ( 0.8389271868029124501, 1.036056831587903609E-16, 0.5442436726714893203 ) ) ;
#21541 = ORIENTED_EDGE ( 'NONE', *, *, #626, .T. ) ;
#21542 = CARTESIAN_POINT ( 'NONE',  ( -42.38687957179150345, 4.148162238788003719, 57.04930799450051637 ) ) ;
#21543 = DIRECTION ( 'NONE',  ( -1.000000000000000000, -1.101824276508910010E-16, 0.000000000000000000 ) ) ;
#21544 = DIRECTION ( 'NONE',  ( -1.224646799147353207E-16, -1.349345573449484691E-32, 1.000000000000000000 ) ) ;
#21545 = DIRECTION ( 'NONE',  ( -1.000000000000000000, 0.000000000000000000, 0.000000000000000000 ) ) ;
#21546 = VECTOR ( 'NONE', #12072, 1000.000000000000000 ) ;
#21547 = EDGE_LOOP ( 'NONE', ( #2292, #31043, #15914, #16146 ) ) ;
#21548 = CARTESIAN_POINT ( 'NONE',  ( 48.75540398364718442, 22.86454579224779948, 48.16909669137300654 ) ) ;
#21549 = CIRCLE ( 'NONE', #20510, 29.01837281655233269 ) ;
#21550 = ORIENTED_EDGE ( 'NONE', *, *, #6390, .F. ) ;
#21551 = AXIS2_PLACEMENT_3D ( 'NONE', #11535, #19065, #11217 ) ;
#21552 = VECTOR ( 'NONE', #6327, 1000.000000000000000 ) ;
#21553 = EDGE_CURVE ( 'NONE', #9682, #14004, #1807, .T. ) ;
#21554 = ORIENTED_EDGE ( 'NONE', *, *, #20800, .T. ) ;
#21555 = ADVANCED_FACE ( 'NONE', ( #11515 ), #29735, .T. ) ;
#21556 = EDGE_CURVE ( 'NONE', #19811, #23536, #8629, .T. ) ;
#21557 = CIRCLE ( 'NONE', #5975, 12.27641737965286772 ) ;
#21558 = EDGE_CURVE ( 'NONE', #2431, #21817, #9714, .T. ) ;
#21559 = ADVANCED_FACE ( 'NONE', ( #13992, #14479 ), #24471, .F. ) ;
#21560 = CARTESIAN_POINT ( 'NONE',  ( 33.72499318558949000, 38.56284415653841791, 47.04930799450051637 ) ) ;
#21561 = AXIS2_PLACEMENT_3D ( 'NONE', #9809, #12115, #17515 ) ;
#21562 = FACE_OUTER_BOUND ( 'NONE', #12759, .T. ) ;
#21563 = DIRECTION ( 'NONE',  ( -0.000000000000000000, -1.000000000000000000, 0.000000000000000000 ) ) ;
#21564 = DIRECTION ( 'NONE',  ( 0.8746197071393925215, -0.4848096202463429982, -8.676864087101708112E-18 ) ) ;
#21565 = EDGE_LOOP ( 'NONE', ( #20420, #22234, #29902, #7340 ) ) ;
#21566 = DIRECTION ( 'NONE',  ( 0.000000000000000000, 0.000000000000000000, -1.000000000000000000 ) ) ;
#21567 = VERTEX_POINT ( 'NONE', #1499 ) ;
#21568 = TOROIDAL_SURFACE ( 'NONE', #31036, 1.299999999999999822, 0.1000000000000000056 ) ;
#21569 = CIRCLE ( 'NONE', #3243, 12.36707279061065279 ) ;
#21570 = CARTESIAN_POINT ( 'NONE',  ( 8.698509210239548040, 28.09164230456639544, 47.04930799450051637 ) ) ;
#21571 = EDGE_CURVE ( 'NONE', #24849, #18606, #12838, .T. ) ;
#21572 = LINE ( 'NONE', #26179, #1094 ) ;
#21573 = VERTEX_POINT ( 'NONE', #21682 ) ;
#21574 = DIRECTION ( 'NONE',  ( 0.000000000000000000, 0.000000000000000000, -1.000000000000000000 ) ) ;
#21575 = DIRECTION ( 'NONE',  ( -1.101824276508909887E-16, 1.000000000000000000, -0.000000000000000000 ) ) ;
#21576 = DIRECTION ( 'NONE',  ( -1.101824276508909887E-16, 1.000000000000000000, -0.000000000000000000 ) ) ;
#21577 = CARTESIAN_POINT ( 'NONE',  ( -40.58856461370174884, 7.499380836222963254, 53.94930799450052206 ) ) ;
#21578 = ORIENTED_EDGE ( 'NONE', *, *, #2929, .T. ) ;
#21579 = DIRECTION ( 'NONE',  ( -1.101824276508909887E-16, 1.000000000000000000, -0.000000000000000000 ) ) ;
#21580 = DIRECTION ( 'NONE',  ( -1.224646799147353207E-16, 0.000000000000000000, -1.000000000000000000 ) ) ;
#21581 = DIRECTION ( 'NONE',  ( -1.000000000000000000, 0.000000000000000000, 0.000000000000000000 ) ) ;
#21582 = DIRECTION ( 'NONE',  ( -0.000000000000000000, -1.000000000000000000, -0.000000000000000000 ) ) ;
#21583 = FILL_AREA_STYLE_COLOUR ( '', #15233 ) ;
#21584 = EDGE_LOOP ( 'NONE', ( #3881, #12195, #7368, #30669 ) ) ;
#21585 = CARTESIAN_POINT ( 'NONE',  ( -40.16503835899720087, 7.510440877657817538, 35.29832907986742185 ) ) ;
#21586 = CARTESIAN_POINT ( 'NONE',  ( -30.88361648749964772, 11.92558985988973141, 26.60346110398183583 ) ) ;
#21587 = ORIENTED_EDGE ( 'NONE', *, *, #14008, .T. ) ;
#21589 = EDGE_CURVE ( 'NONE', #18870, #2451, #31711, .T. ) ;
#21588 = CARTESIAN_POINT ( 'NONE',  ( 21.09992658989239089, 26.59164230456639899, 47.04930799450051637 ) ) ;
#21590 = CIRCLE ( 'NONE', #4830, 0.1000000000000018235 ) ;
#21591 = DIRECTION ( 'NONE',  ( 0.6797146636928705909, 0.1949050434465292025, -0.7071067811865436870 ) ) ;
#21592 = CIRCLE ( 'NONE', #1748, 12.62506659569710266 ) ;
#21593 = EDGE_LOOP ( 'NONE', ( #9666, #31361, #22525, #26050 ) ) ;
#21594 = ORIENTED_EDGE ( 'NONE', *, *, #16959, .T. ) ;
#21595 = UNCERTAINTY_MEASURE_WITH_UNIT (LENGTH_MEASURE( 1.000000000000000082E-05 ), #17430, 'distance_accuracy_value', 'NONE');
#21596 = AXIS2_PLACEMENT_3D ( 'NONE', #28858, #21287, #30840 ) ;
#21597 = ORIENTED_EDGE ( 'NONE', *, *, #28606, .T. ) ;
#21598 = ADVANCED_FACE ( 'NONE', ( #21515 ), #25411, .T. ) ;
#21599 = AXIS2_PLACEMENT_3D ( 'NONE', #13106, #32475, #15235 ) ;
#21600 = ADVANCED_FACE ( 'NONE', ( #31553 ), #9688, .T. ) ;
#21601 = CARTESIAN_POINT ( 'NONE',  ( 7.896202261960366009, 17.36467600858027183, 47.04930799450052348 ) ) ;
#21602 = VERTEX_POINT ( 'NONE', #9056 ) ;
#21603 = LINE ( 'NONE', #17001, #13221 ) ;
#21604 = AXIS2_PLACEMENT_3D ( 'NONE', #3295, #25943, #16251 ) ;
#21605 = CARTESIAN_POINT ( 'NONE',  ( 21.09785597605720042, 15.06454579224778456, -7.950692005499485404 ) ) ;
#21606 = CARTESIAN_POINT ( 'NONE',  ( 33.50134396954522487, 28.84164230456639544, 47.04930799450051637 ) ) ;
#21607 = LINE ( 'NONE', #31641, #12247 ) ;
#21608 = CIRCLE ( 'NONE', #8539, 12.36707279061065101 ) ;
#21609 = CARTESIAN_POINT ( 'NONE',  ( 45.38854177497844944, 29.76952976649964100, 45.94041160078741370 ) ) ;
#21610 = ORIENTED_EDGE ( 'NONE', *, *, #15045, .F. ) ;
#21611 = CARTESIAN_POINT ( 'NONE',  ( -38.53060556916744162, -5.935485795843228551, 78.00951309620023721 ) ) ;
#21612 = ORIENTED_EDGE ( 'NONE', *, *, #30344, .F. ) ;
#21613 = FACE_OUTER_BOUND ( 'NONE', #5482, .T. ) ;
#21614 = EDGE_LOOP ( 'NONE', ( #16434, #4904, #13277, #11125 ) ) ;
#21617 = EDGE_CURVE ( 'NONE', #1140, #4802, #9665, .T. ) ;
#21616 = VECTOR ( 'NONE', #18630, 1000.000000000000000 ) ;
#21615 = DIRECTION ( 'NONE',  ( -1.000000000000000000, 0.000000000000000000, 0.000000000000000000 ) ) ;
#21618 = CARTESIAN_POINT ( 'NONE',  ( 33.71785032049137953, 24.46664230456639899, 47.04930799450051637 ) ) ;
#21619 = CARTESIAN_POINT ( 'NONE',  ( 21.09785597605719332, -5.986312001188950127, 47.04930799450051637 ) ) ;
#21620 = DIRECTION ( 'NONE',  ( -1.101824276508909887E-16, 1.000000000000000000, -0.000000000000000000 ) ) ;
#21621 = DIRECTION ( 'NONE',  ( 0.000000000000000000, -0.000000000000000000, -1.000000000000000000 ) ) ;
#21622 = CARTESIAN_POINT ( 'NONE',  ( 45.46000861347822308, 25.37287913140504614, 49.57397645940629616 ) ) ;
#21623 = TOROIDAL_SURFACE ( 'NONE', #4342, 12.40141737965284996, 0.1250000000000002776 ) ;
#21624 = CARTESIAN_POINT ( 'NONE',  ( 46.48525799733394592, 23.04411619146717882, 47.99360027521537830 ) ) ;
#21625 = DIRECTION ( 'NONE',  ( -0.000000000000000000, -1.000000000000000000, -0.000000000000000000 ) ) ;
#21626 = EDGE_LOOP ( 'NONE', ( #31246, #29733 ) ) ;
#21627 = CARTESIAN_POINT ( 'NONE',  ( 21.09785597605720753, 17.36467600858027183, 47.04930799450052348 ) ) ;
#21629 = ADVANCED_FACE ( 'NONE', ( #2804 ), #25297, .T. ) ;
#21628 = LINE ( 'NONE', #19651, #23477 ) ;
#21630 = CARTESIAN_POINT ( 'NONE',  ( -40.94655644966159969, 10.23591835516384840, 37.04930799450052348 ) ) ;
#21631 = ADVANCED_FACE ( 'NONE', ( #12342 ), #24343, .T. ) ;
#21632 = DIRECTION ( 'NONE',  ( -0.4848096202463373916, -0.8746197071393956302, -9.920727850371752502E-18 ) ) ;
#21633 = LINE ( 'NONE', #13942, #31945 ) ;
#21634 = ORIENTED_EDGE ( 'NONE', *, *, #29393, .F. ) ;
#21635 = LINE ( 'NONE', #14268, #25580 ) ;
#21636 = VERTEX_POINT ( 'NONE', #2323 ) ;
#21637 = CARTESIAN_POINT ( 'NONE',  ( 67.77233896511883415, 13.66454579224780019, 47.04930799450051637 ) ) ;
#21638 = CYLINDRICAL_SURFACE ( 'NONE', #26685, 12.62506659569710266 ) ;
#21639 = ORIENTED_EDGE ( 'NONE', *, *, #22630, .T. ) ;
#21640 = AXIS2_PLACEMENT_3D ( 'NONE', #18824, #3905, #11454 ) ;
#21641 = AXIS2_PLACEMENT_3D ( 'NONE', #15730, #27890, #23283 ) ;
#21642 = EDGE_CURVE ( 'NONE', #16662, #15784, #28007, .T. ) ;
#21643 = AXIS2_PLACEMENT_3D ( 'NONE', #21875, #13861, #1699 ) ;
#21644 = AXIS2_PLACEMENT_3D ( 'NONE', #160, #319, #18036 ) ;
#21645 = ORIENTED_EDGE ( 'NONE', *, *, #30511, .T. ) ;
#21646 = CARTESIAN_POINT ( 'NONE',  ( 8.474859994195282908, 38.56284415653841791, 47.04930799450051637 ) ) ;
#21647 = DIRECTION ( 'NONE',  ( -1.101824276508909887E-16, 1.000000000000000000, -0.000000000000000000 ) ) ;
#21648 = FACE_OUTER_BOUND ( 'NONE', #2076, .T. ) ;
#21649 = ORIENTED_EDGE ( 'NONE', *, *, #23902, .T. ) ;
#21650 = CARTESIAN_POINT ( 'NONE',  ( 45.96182992765471198, 25.16454579224780019, 44.82232689504101586 ) ) ;
#21651 = CARTESIAN_POINT ( 'NONE',  ( -40.21091586930921125, 6.838981405724005036, 34.54930799450052348 ) ) ;
#21652 = CARTESIAN_POINT ( 'NONE',  ( 76.02014513276924390, -2.123693335316784836, 13.33257895622572065 ) ) ;
#21653 = EDGE_CURVE ( 'NONE', #31740, #25382, #496, .T. ) ;
#21654 = ORIENTED_EDGE ( 'NONE', *, *, #29417, .F. ) ;
#21655 = DIRECTION ( 'NONE',  ( -4.163336342344334660E-15, 0.000000000000000000, 1.000000000000000000 ) ) ;
#21656 = ORIENTED_EDGE ( 'NONE', *, *, #19250, .T. ) ;
#21657 = ADVANCED_FACE ( 'NONE', ( #7902 ), #14920, .T. ) ;
#21658 = DIRECTION ( 'NONE',  ( -0.9612616959383194493, -0.2756373558169972759, -8.795445018804905742E-19 ) ) ;
#21659 = CARTESIAN_POINT ( 'NONE',  ( -42.79701293673568330, 15.60084045232229677, 37.04930799450052348 ) ) ;
#21660 = CIRCLE ( 'NONE', #20613, 12.36707279061065279 ) ;
#21661 = DIRECTION ( 'NONE',  ( -1.101824276508909887E-16, 1.000000000000000000, -0.000000000000000000 ) ) ;
#21662 = DIRECTION ( 'NONE',  ( 0.000000000000000000, 0.000000000000000000, 1.000000000000000000 ) ) ;
#21663 = EDGE_LOOP ( 'NONE', ( #21765, #17615, #293, #9661 ) ) ;
#21664 = ORIENTED_EDGE ( 'NONE', *, *, #17036, .F. ) ;
#21665 = CARTESIAN_POINT ( 'NONE',  ( -35.64882101543633297, 9.925589859889724309, 52.04930799450051637 ) ) ;
#21666 = CARTESIAN_POINT ( 'NONE',  ( -40.02540636251513462, 2.839176264122873050, 37.04930799450052348 ) ) ;
#21667 = ADVANCED_FACE ( 'NONE', ( #10358 ), #24873, .F. ) ;
#21668 = EDGE_CURVE ( 'NONE', #22420, #23989, #29609, .T. ) ;
#21669 = VECTOR ( 'NONE', #13853, 1000.000000000000114 ) ;
#21670 = DIRECTION ( 'NONE',  ( 0.000000000000000000, -1.000000000000000000, 0.000000000000000000 ) ) ;
#21671 = ORIENTED_EDGE ( 'NONE', *, *, #19468, .T. ) ;
#21672 = AXIS2_PLACEMENT_3D ( 'NONE', #26123, #10395, #31064 ) ;
#21673 = CARTESIAN_POINT ( 'NONE',  ( -12.32854732834748468, -0.6709275202869608989, -7.106067055362325746 ) ) ;
#21674 = CARTESIAN_POINT ( 'NONE',  ( 71.62639656063520022, -13.74047052604243646, 17.87036105788319063 ) ) ;
#21675 = CIRCLE ( 'NONE', #24304, 12.62506659569710443 ) ;
#21676 = ORIENTED_EDGE ( 'NONE', *, *, #17597, .F. ) ;
#21677 = CARTESIAN_POINT ( 'NONE',  ( 8.732853799281732776, 32.21183152705962272, 47.04930799450051637 ) ) ;
#21678 = CARTESIAN_POINT ( 'NONE',  ( 21.09785597605719332, 77.37245976740706510, -36.90550222348115028 ) ) ;
#21679 = DIRECTION ( 'NONE',  ( -1.224646799147353207E-16, -1.349345573449484691E-32, 1.000000000000000000 ) ) ;
#21680 = ORIENTED_EDGE ( 'NONE', *, *, #12621, .T. ) ;
#21681 = CARTESIAN_POINT ( 'NONE',  ( -63.90214402394282445, -3.935454207752183020, 52.04930799450050927 ) ) ;
#21682 = CARTESIAN_POINT ( 'NONE',  ( 8.732853799281732776, 23.97145308207319303, 47.04930799450051637 ) ) ;
#21683 = CARTESIAN_POINT ( 'NONE',  ( 21.09785597605719332, 15.24673779880127356, 47.04930799450051637 ) ) ;
#21684 = CARTESIAN_POINT ( 'NONE',  ( 48.18662509608405031, 28.68284706826092290, 49.18364984542562013 ) ) ;
#21685 = ORIENTED_EDGE ( 'NONE', *, *, #14489, .F. ) ;
#21686 = AXIS2_PLACEMENT_3D ( 'NONE', #23897, #16825, #24221 ) ;
#21687 = CARTESIAN_POINT ( 'NONE',  ( 21.09785597605720042, -13.88867167006704939, 47.04930799450051637 ) ) ;
#21688 = DIRECTION ( 'NONE',  ( 0.000000000000000000, -0.000000000000000000, -1.000000000000000000 ) ) ;
#21689 = EDGE_CURVE ( 'NONE', #15249, #23287, #12510, .T. ) ;
#21690 = CARTESIAN_POINT ( 'NONE',  ( 54.70353123047690502, -3.653843372214150786, -7.997390199024978941 ) ) ;
#21691 = EDGE_CURVE ( 'NONE', #20242, #32279, #22126, .T. ) ;
#21692 = CARTESIAN_POINT ( 'NONE',  ( -9.728297238921268075, -5.935454207752198563, 106.7470117857220373 ) ) ;
#21693 = LINE ( 'NONE', #2002, #23176 ) ;
#21694 = DIRECTION ( 'NONE',  ( -1.101824276508909887E-16, 1.000000000000000000, -0.000000000000000000 ) ) ;
#21695 = FACE_OUTER_BOUND ( 'NONE', #28857, .T. ) ;
#21696 = CARTESIAN_POINT ( 'NONE',  ( 45.00053793792376666, 25.25920399681023198, 45.68869892245983522 ) ) ;
#21697 = ORIENTED_EDGE ( 'NONE', *, *, #19784, .F. ) ;
#21698 = CARTESIAN_POINT ( 'NONE',  ( 21.09992658989238734, 38.56284415653841791, 47.04930799450051637 ) ) ;
#21699 = CARTESIAN_POINT ( 'NONE',  ( 48.59452595530246555, 24.93986642951281496, 44.74225815255415739 ) ) ;
#21700 = EDGE_CURVE ( 'NONE', #28686, #19450, #18568, .T. ) ;
#21701 = DIRECTION ( 'NONE',  ( 1.000000000000000000, 0.000000000000000000, 0.000000000000000000 ) ) ;
#21702 = EDGE_CURVE ( 'NONE', #30447, #7753, #32202, .T. ) ;
#21703 = DIRECTION ( 'NONE',  ( 0.000000000000000000, 0.000000000000000000, -1.000000000000000000 ) ) ;
#21704 = ORIENTED_EDGE ( 'NONE', *, *, #13951, .T. ) ;
#21705 = CARTESIAN_POINT ( 'NONE',  ( -38.96025635604169679, 15.13029464144909930, 54.54930799450051637 ) ) ;
#21706 = CARTESIAN_POINT ( 'NONE',  ( -44.54447070791992758, -4.637414085371450945, 41.95757092055643511 ) ) ;
#21707 = DIRECTION ( 'NONE',  ( -1.101824276508909887E-16, 1.000000000000000000, -0.000000000000000000 ) ) ;
#21708 = ORIENTED_EDGE ( 'NONE', *, *, #18018, .T. ) ;
#21709 = VERTEX_POINT ( 'NONE', #22492 ) ;
#21711 = AXIS2_PLACEMENT_3D ( 'NONE', #31122, #18624, #18779 ) ;
#21710 = DIRECTION ( 'NONE',  ( -0.000000000000000000, -1.000000000000000000, 0.000000000000000000 ) ) ;
#21712 = CARTESIAN_POINT ( 'NONE',  ( 33.50134396954522487, 28.59164230456639544, 47.04930799450051637 ) ) ;
#21713 = B_SPLINE_CURVE_WITH_KNOTS ( 'NONE', 3,
 ( #10932, #13553, #755, #13403, #13249, #23239, #592, #1223, #30638, #25703, #23398, #8774 ),
 .UNSPECIFIED., .F., .F.,
 ( 4, 2, 2, 2, 2, 4 ),
 ( 0.0002262585095220170678, 0.001077298125046782578, 0.001928337740571547899, 0.002779377356096313437, 0.003204897163858691327, 0.003630416971621069650 ),
 .UNSPECIFIED. ) ;
#21714 = AXIS2_PLACEMENT_3D ( 'NONE', #24161, #11699, #26948 ) ;
#21715 = CARTESIAN_POINT ( 'NONE',  ( -38.32955388700093380, 6.929907785659376707, 61.94930799450052206 ) ) ;
#21716 = CARTESIAN_POINT ( 'NONE',  ( 21.09785597605720753, -16.03545420775220265, 117.6483275080933169 ) ) ;
#21717 = CIRCLE ( 'NONE', #29055, 0.7905694150420993216 ) ;
#21718 = ORIENTED_EDGE ( 'NONE', *, *, #17874, .F. ) ;
#21719 = CARTESIAN_POINT ( 'NONE',  ( 46.93148653487033073, 29.42016659326356987, 49.29260710712500781 ) ) ;
#21720 = ORIENTED_EDGE ( 'NONE', *, *, #30075, .T. ) ;
#21721 = VERTEX_POINT ( 'NONE', #19871 ) ;
#21722 = CARTESIAN_POINT ( 'NONE',  ( 52.07598125554711999, -5.935454207752202116, 107.6772108465075490 ) ) ;
#21723 = CIRCLE ( 'NONE', #7601, 19.00000000000000000 ) ;
#21724 = FACE_OUTER_BOUND ( 'NONE', #28599, .T. ) ;
#21725 = FACE_OUTER_BOUND ( 'NONE', #30614, .T. ) ;
#21726 = AXIS2_PLACEMENT_3D ( 'NONE', #13330, #13002, #5932 ) ;
#21727 = CARTESIAN_POINT ( 'NONE',  ( 8.698509210239532052, 26.59164230456639899, 47.04930799450051637 ) ) ;
#21728 = CIRCLE ( 'NONE', #12309, 12.27641737965285529 ) ;
#21729 = AXIS2_PLACEMENT_3D ( 'NONE', #2419, #22421, #2573 ) ;
#21730 = ORIENTED_EDGE ( 'NONE', *, *, #3631, .T. ) ;
#21731 = DIRECTION ( 'NONE',  ( -1.000000000000000000, 0.000000000000000000, 0.000000000000000000 ) ) ;
#21732 = ORIENTED_EDGE ( 'NONE', *, *, #26893, .F. ) ;
#21733 = AXIS2_PLACEMENT_3D ( 'NONE', #15555, #628, #10660 ) ;
#21734 = CARTESIAN_POINT ( 'NONE',  ( 21.09992658989239089, 23.84164230456639544, 47.04930799450051637 ) ) ;
#21735 = DIRECTION ( 'NONE',  ( 0.2756373558169932236, -0.9612616959383204485, 1.479773560108267395E-16 ) ) ;
#21736 = DIRECTION ( 'NONE',  ( 1.775804005134407553E-15, 0.000000000000000000, 1.000000000000000000 ) ) ;
#21737 = VERTEX_POINT ( 'NONE', #27754 ) ;
#21738 = CARTESIAN_POINT ( 'NONE',  ( 21.09785597605719332, -19.93545420775220123, 47.04930799450051637 ) ) ;
#21739 = CARTESIAN_POINT ( 'NONE',  ( 21.09992658989239089, 24.21664230456639899, 47.04930799450051637 ) ) ;
#21740 = DIRECTION ( 'NONE',  ( 0.000000000000000000, 0.000000000000000000, -1.000000000000000000 ) ) ;
#21741 = DIRECTION ( 'NONE',  ( -1.101824276508909887E-16, 1.000000000000000000, -0.000000000000000000 ) ) ;
#21742 = ADVANCED_FACE ( 'NONE', ( #29904 ), #22232, .F. ) ;
#21743 = CARTESIAN_POINT ( 'NONE',  ( 33.37634396954518223, 32.34164230456639899, 47.04930799450051637 ) ) ;
#21744 = DIRECTION ( 'NONE',  ( 1.000000000000000000, 0.000000000000000000, 0.000000000000000000 ) ) ;
#21745 = DIRECTION ( 'NONE',  ( 0.000000000000000000, 0.000000000000000000, -1.000000000000000000 ) ) ;
#21746 = DIRECTION ( 'NONE',  ( 0.8907924397839086517, 1.100109291107994064E-16, -0.4544104193609905251 ) ) ;
#21747 = EDGE_CURVE ( 'NONE', #32154, #20897, #26429, .T. ) ;
#21748 = ORIENTED_EDGE ( 'NONE', *, *, #24799, .T. ) ;
#21749 = DIRECTION ( 'NONE',  ( -1.101824276508909887E-16, 1.000000000000000000, -0.000000000000000000 ) ) ;
#21750 = CARTESIAN_POINT ( 'NONE',  ( 8.732853799281734553, 38.56284415653841791, 47.04930799450051637 ) ) ;
#21751 = VERTEX_POINT ( 'NONE', #5278 ) ;
#21752 = CARTESIAN_POINT ( 'NONE',  ( -44.11954960567759088, -5.396560688972869002, 41.42132194764992903 ) ) ;
#21753 = LINE ( 'NONE', #24543, #3819 ) ;
#21754 = ORIENTED_EDGE ( 'NONE', *, *, #18245, .T. ) ;
#21755 = AXIS2_PLACEMENT_3D ( 'NONE', #3567, #947, #11139 ) ;
#21756 = ORIENTED_EDGE ( 'NONE', *, *, #21512, .T. ) ;
#21757 = VECTOR ( 'NONE', #8354, 1000.000000000000000 ) ;
#21758 = CIRCLE ( 'NONE', #11815, 2.000000000000001776 ) ;
#21759 = AXIS2_PLACEMENT_3D ( 'NONE', #22225, #7139, #7304 ) ;
#21760 = AXIS2_PLACEMENT_3D ( 'NONE', #15816, #1188, #13041 ) ;
#21761 = ORIENTED_EDGE ( 'NONE', *, *, #29250, .T. ) ;
#21762 = LINE ( 'NONE', #31783, #14583 ) ;
#21763 = EDGE_CURVE ( 'NONE', #28192, #7248, #10731, .T. ) ;
#21764 = ORIENTED_EDGE ( 'NONE', *, *, #20268, .F. ) ;
#21765 = ORIENTED_EDGE ( 'NONE', *, *, #21029, .F. ) ;
#21766 = DIRECTION ( 'NONE',  ( -1.101824276508909887E-16, 1.000000000000000000, -0.000000000000000000 ) ) ;
#21767 = DIRECTION ( 'NONE',  ( 0.000000000000000000, 0.000000000000000000, -1.000000000000000000 ) ) ;
#21768 = DIRECTION ( 'NONE',  ( 0.000000000000000000, -0.000000000000000000, -1.000000000000000000 ) ) ;
#21769 = CARTESIAN_POINT ( 'NONE',  ( 48.37829923888483563, 27.49452976649965308, 45.07556196625585443 ) ) ;
#21770 = VERTEX_POINT ( 'NONE', #21312 ) ;
#21771 = DIRECTION ( 'NONE',  ( 1.000000000000000000, -0.000000000000000000, -0.000000000000000000 ) ) ;
#21772 = VERTEX_POINT ( 'NONE', #13318 ) ;
#21774 = CARTESIAN_POINT ( 'NONE',  ( -12.63390874224687899, -2.844921901652555540, -7.393120321654669702 ) ) ;
#21773 = TOROIDAL_SURFACE ( 'NONE', #22843, 56.00000000000000000, 1.700000000000000178 ) ;
#21775 =( GEOMETRIC_REPRESENTATION_CONTEXT ( 3 ) GLOBAL_UNCERTAINTY_ASSIGNED_CONTEXT ( ( #3240 ) ) GLOBAL_UNIT_ASSIGNED_CONTEXT ( ( #27118, #16773, #31567 ) ) REPRESENTATION_CONTEXT ( 'NONE', 'WORKASPACE' ) );
#21776 = ORIENTED_EDGE ( 'NONE', *, *, #5761, .T. ) ;
#21777 = CARTESIAN_POINT ( 'NONE',  ( -41.56459318755936749, 7.281738416154046156, 60.44930799450051495 ) ) ;
#21778 = FACE_OUTER_BOUND ( 'NONE', #6164, .T. ) ;
#21779 = DIRECTION ( 'NONE',  ( -1.101824276508909887E-16, 1.000000000000000000, -0.000000000000000000 ) ) ;
#21780 = CARTESIAN_POINT ( 'NONE',  ( 21.09992658989239089, 24.46183152705960140, 47.04930799450051637 ) ) ;
#21781 = DIRECTION ( 'NONE',  ( 0.000000000000000000, -0.000000000000000000, 1.000000000000000000 ) ) ;
#21782 = EDGE_CURVE ( 'NONE', #3066, #3389, #30640, .T. ) ;
#21783 = EDGE_CURVE ( 'NONE', #26975, #29530, #3371, .T. ) ;
#21784 = CARTESIAN_POINT ( 'NONE',  ( 49.41945501136223839, 24.96454579807171470, 45.86501535757901848 ) ) ;
#21785 = EDGE_CURVE ( 'NONE', #31872, #16293, #21717, .T. ) ;
#21786 = DIRECTION ( 'NONE',  ( 0.1949050434465282311, -0.6797146636928674823, -0.7071067811865470176 ) ) ;
#21787 = CARTESIAN_POINT ( 'NONE',  ( 46.82137942583813128, 14.98691807112498964, 46.50732389770341513 ) ) ;
#21788 = EDGE_CURVE ( 'NONE', #3389, #9948, #757, .T. ) ;
#21789 = ORIENTED_EDGE ( 'NONE', *, *, #13362, .F. ) ;
#21790 = CARTESIAN_POINT ( 'NONE',  ( -20.40214402394279603, 14.86454579224779948, 47.04930799450052348 ) ) ;
#21791 = CARTESIAN_POINT ( 'NONE',  ( 21.09785597605719332, 48.06454579224779877, 65.91126043309506599 ) ) ;
#21792 = EDGE_CURVE ( 'NONE', #14642, #1960, #5542, .T. ) ;
#21793 = FACE_OUTER_BOUND ( 'NONE', #28889, .T. ) ;
#21794 = AXIS2_PLACEMENT_3D ( 'NONE', #3201, #5518, #23235 ) ;
#21795 = CARTESIAN_POINT ( 'NONE',  ( 21.09785597605719332, 40.06454579224778456, 59.04930799450051637 ) ) ;
#21796 = FACE_OUTER_BOUND ( 'NONE', #29717, .T. ) ;
#21797 = ORIENTED_EDGE ( 'NONE', *, *, #15559, .T. ) ;
#21798 = FACE_OUTER_BOUND ( 'NONE', #19706, .T. ) ;
#21799 = ORIENTED_EDGE ( 'NONE', *, *, #17977, .T. ) ;
#21800 = DIRECTION ( 'NONE',  ( -1.000000000000000000, 0.000000000000000000, 0.000000000000000000 ) ) ;
#21801 = FACE_OUTER_BOUND ( 'NONE', #3378, .T. ) ;
#21802 = EDGE_LOOP ( 'NONE', ( #15160, #24970, #6665 ) ) ;
#21803 = AXIS2_PLACEMENT_3D ( 'NONE', #29062, #11671, #6254 ) ;
#21804 =( GEOMETRIC_REPRESENTATION_CONTEXT ( 3 ) GLOBAL_UNCERTAINTY_ASSIGNED_CONTEXT ( ( #8498 ) ) GLOBAL_UNIT_ASSIGNED_CONTEXT ( ( #19687, #21979, #32010 ) ) REPRESENTATION_CONTEXT ( 'NONE', 'WORKASPACE' ) );
#21805 = ORIENTED_EDGE ( 'NONE', *, *, #20757, .T. ) ;
#21806 = CARTESIAN_POINT ( 'NONE',  ( -39.64148344771002286, 7.657122216028890982, 61.94930799450052206 ) ) ;
#21807 = EDGE_CURVE ( 'NONE', #15416, #31613, #8377, .T. ) ;
#21808 = CARTESIAN_POINT ( 'NONE',  ( 53.16981722132879185, -5.983766253076979069, -12.70392589783158499 ) ) ;
#21809 = DIRECTION ( 'NONE',  ( -1.000000000000000000, 0.000000000000000000, 0.000000000000000000 ) ) ;
#21810 = EDGE_CURVE ( 'NONE', #24691, #28989, #19123, .T. ) ;
#21811 = CIRCLE ( 'NONE', #6104, 12.27641737965284996 ) ;
#21812 = ORIENTED_EDGE ( 'NONE', *, *, #632, .T. ) ;
#21813 = DIRECTION ( 'NONE',  ( -0.2756373558169954441, 0.9612616959383198934, -1.479773560108263204E-16 ) ) ;
#21814 = CARTESIAN_POINT ( 'NONE',  ( 33.46699938050304013, 38.56284415653841791, 47.04930799450051637 ) ) ;
#21815 = CARTESIAN_POINT ( 'NONE',  ( 79.11899642186367032, -5.573920848077356105, 14.84471408225261690 ) ) ;
#21816 = ORIENTED_EDGE ( 'NONE', *, *, #13987, .T. ) ;
#21817 = VERTEX_POINT ( 'NONE', #25770 ) ;
#21818 = FILL_AREA_STYLE ('',( #9684 ) ) ;
#21819 = ORIENTED_EDGE ( 'NONE', *, *, #12318, .F. ) ;
#21820 = DIRECTION ( 'NONE',  ( 1.234978253042719660E-16, -1.000000000000000000, -1.109335647967047851E-31 ) ) ;
#21821 = DIRECTION ( 'NONE',  ( 0.2756373558170082672, -0.9612616959383162296, 3.469446951953592101E-14 ) ) ;
#21822 = EDGE_CURVE ( 'NONE', #13392, #5398, #24880, .T. ) ;
#21823 = CARTESIAN_POINT ( 'NONE',  ( -34.02276494433180432, 1.214306433183764966E-14, 35.71885702409839070 ) ) ;
#21824 = EDGE_LOOP ( 'NONE', ( #5744, #3427, #30177, #6885 ) ) ;
#21825 = ORIENTED_EDGE ( 'NONE', *, *, #19998, .T. ) ;
#21826 = CYLINDRICAL_SURFACE ( 'NONE', #25495, 12.62506659569710443 ) ;
#21827 = CIRCLE ( 'NONE', #15535, 0.1250000000000001110 ) ;
#21828 = DIRECTION ( 'NONE',  ( 0.4848096202463429427, 0.8746197071393925215, -2.352477780477436294E-16 ) ) ;
#21829 = DIRECTION ( 'NONE',  ( -0.000000000000000000, -1.000000000000000000, -0.000000000000000000 ) ) ;
#21830 = VERTEX_POINT ( 'NONE', #23788 ) ;
#21831 = FACE_OUTER_BOUND ( 'NONE', #23723, .T. ) ;
#21832 = DIRECTION ( 'NONE',  ( 1.000000000000000000, 0.000000000000000000, 0.000000000000000000 ) ) ;
#21833 = ORIENTED_EDGE ( 'NONE', *, *, #1621, .F. ) ;
#21834 = FACE_OUTER_BOUND ( 'NONE', #21169, .T. ) ;
#21835 = CARTESIAN_POINT ( 'NONE',  ( 44.09250526802607340, 25.95621246473837829, 46.89322480343881949 ) ) ;
#21836 = AXIS2_PLACEMENT_3D ( 'NONE', #10243, #20237, #15159 ) ;
#21837 = CARTESIAN_POINT ( 'NONE',  ( 21.09785597605720753, 13.86454579224779948, 47.04930799450052348 ) ) ;
#21838 = ADVANCED_FACE ( 'NONE', ( #20841 ), #13153, .F. ) ;
#21839 = ADVANCED_FACE ( 'NONE', ( #6235 ), #3606, .F. ) ;
#21840 = ORIENTED_EDGE ( 'NONE', *, *, #5946, .F. ) ;
#21841 = CARTESIAN_POINT ( 'NONE',  ( 55.09785597605721108, 13.86454579224779948, 47.04930799450051637 ) ) ;
#21842 = DIRECTION ( 'NONE',  ( 0.2756373558169974980, -0.9612616959383193382, -1.315048337272770589E-17 ) ) ;
#21843 = ADVANCED_FACE ( 'NONE', ( #30867 ), #13791, .T. ) ;
#21844 = CIRCLE ( 'NONE', #18697, 0.1249999999999983763 ) ;
#21845 = CARTESIAN_POINT ( 'NONE',  ( 21.09785597605721108, -17.03545420775220265, 125.4493079945005150 ) ) ;
#21846 = CARTESIAN_POINT ( 'NONE',  ( 44.70507715278255745, 29.84951373492758719, 46.92503878583764987 ) ) ;
#21847 = ADVANCED_FACE ( 'NONE', ( #18058, #28085 ), #5593, .T. ) ;
#21848 = ORIENTED_EDGE ( 'NONE', *, *, #19622, .F. ) ;
#21849 = ADVANCED_FACE ( 'NONE', ( #20683 ), #26415, .T. ) ;
#21850 = DIRECTION ( 'NONE',  ( -1.101824276508909887E-16, 1.000000000000000000, -0.000000000000000000 ) ) ;
#21851 = CARTESIAN_POINT ( 'NONE',  ( -40.66586793973302605, 8.138261812237590931, 54.59072935073782418 ) ) ;
#21852 = PLANE ( 'NONE',  #14729 ) ;
#21853 = CARTESIAN_POINT ( 'NONE',  ( -42.50976151518963064, 14.59907569580870224, 38.19144330556764544 ) ) ;
#21854 = CARTESIAN_POINT ( 'NONE',  ( 21.09992658989239089, 28.09164230456639544, 47.04930799450051637 ) ) ;
#21855 = DIRECTION ( 'NONE',  ( -1.000000000000000000, 0.000000000000000000, 0.000000000000000000 ) ) ;
#21856 = DIRECTION ( 'NONE',  ( -1.101824276508909887E-16, 1.000000000000000000, -0.000000000000000000 ) ) ;
#21857 = CARTESIAN_POINT ( 'NONE',  ( 52.20929784716416577, -5.935454207834595763, 107.5147914783766510 ) ) ;
#21858 = EDGE_CURVE ( 'NONE', #32154, #13543, #28060, .T. ) ;
#21859 = EDGE_LOOP ( 'NONE', ( #19736, #27559, #2510, #7063 ) ) ;
#21860 = CARTESIAN_POINT ( 'NONE',  ( -40.58856461370174884, 7.499380836222963254, 53.94930799450052206 ) ) ;
#21861 = CARTESIAN_POINT ( 'NONE',  ( 46.94177278499491734, 25.43121246473836550, 50.05465870253188854 ) ) ;
#21862 = DIRECTION ( 'NONE',  ( 0.000000000000000000, -1.000000000000000000, 0.000000000000000000 ) ) ;
#21863 = CARTESIAN_POINT ( 'NONE',  ( -9.902144023942794249, -5.098646251524523443, 47.04930799450052348 ) ) ;
#21864 = ORIENTED_EDGE ( 'NONE', *, *, #31430, .F. ) ;
#21865 = CARTESIAN_POINT ( 'NONE',  ( 8.698509210239585343, 32.09164230456639899, 47.04930799450051637 ) ) ;
#21866 = AXIS2_PLACEMENT_3D ( 'NONE', #3969, #24312, #28926 ) ;
#21867 = CARTESIAN_POINT ( 'NONE',  ( -45.02838518323464001, -5.632298750458708980, 41.12626815361094401 ) ) ;
#21868 = DIRECTION ( 'NONE',  ( 0.000000000000000000, 0.000000000000000000, -1.000000000000000000 ) ) ;
#21869 = ORIENTED_EDGE ( 'NONE', *, *, #14228, .T. ) ;
#21870 = ORIENTED_EDGE ( 'NONE', *, *, #4750, .F. ) ;
#21871 = CARTESIAN_POINT ( 'NONE',  ( -40.11669538345026353, 6.804256812083828265, 39.45088313409969771 ) ) ;
#21872 = CARTESIAN_POINT ( 'NONE',  ( -39.57405207560572791, -5.936352567920400780, 77.94940154167748858 ) ) ;
#21873 = TOROIDAL_SURFACE ( 'NONE', #25562, 12.40141737965281621, 0.1250000000000009159 ) ;
#21874 = CARTESIAN_POINT ( 'NONE',  ( -5.602943079677954685, 9.702389020015065313, -37.95069200549950494 ) ) ;
#21875 = CARTESIAN_POINT ( 'NONE',  ( 47.09785597605719687, 24.86454579224779948, 47.04930799450042400 ) ) ;
#21876 = ORIENTED_EDGE ( 'NONE', *, *, #7651, .F. ) ;
#21877 = CARTESIAN_POINT ( 'NONE',  ( 45.66249254611258124, 29.37705119628220274, 48.83685427499938214 ) ) ;
#21878 = CIRCLE ( 'NONE', #28173, 0.9031915329475519449 ) ;
#21879 = ORIENTED_EDGE ( 'NONE', *, *, #2737, .T. ) ;
#21880 = ADVANCED_FACE ( 'NONE', ( #31672, #19176 ), #16398, .T. ) ;
#21881 = EDGE_CURVE ( 'NONE', #22685, #7056, #4084, .T. ) ;
#21882 = ORIENTED_EDGE ( 'NONE', *, *, #9005, .T. ) ;
#21883 = CARTESIAN_POINT ( 'NONE',  ( -41.89334324224037687, 13.85403361400641487, 54.61507042654626787 ) ) ;
#21884 = EDGE_CURVE ( 'NONE', #19026, #13441, #8124, .T. ) ;
#21885 = ORIENTED_EDGE ( 'NONE', *, *, #21029, .T. ) ;
#21886 = DIRECTION ( 'NONE',  ( 0.000000000000000000, 0.000000000000000000, -1.000000000000000000 ) ) ;
#21887 = CARTESIAN_POINT ( 'NONE',  ( -40.50726676055796105, 7.559560307024983494, 53.64930799450051779 ) ) ;
#21888 = CARTESIAN_POINT ( 'NONE',  ( -40.11286833322908052, 2.887657226147511302, 57.04930799450051637 ) ) ;
#21889 = AXIS2_PLACEMENT_3D ( 'NONE', #11606, #11922, #29003 ) ;
#21890 = ORIENTED_EDGE ( 'NONE', *, *, #17286, .T. ) ;
#21891 = CARTESIAN_POINT ( 'NONE',  ( 33.50134396954528171, 23.59164230456639544, 47.04930799450051637 ) ) ;
#21892 = ORIENTED_EDGE ( 'NONE', *, *, #12015, .T. ) ;
#21893 = DIRECTION ( 'NONE',  ( 0.000000000000000000, -0.000000000000000000, -1.000000000000000000 ) ) ;
#21894 = VECTOR ( 'NONE', #17356, 1000.000000000000000 ) ;
#21895 = DIRECTION ( 'NONE',  ( 0.2756373558169959437, -0.9612616959383197823, 0.000000000000000000 ) ) ;
#21896 = CARTESIAN_POINT ( 'NONE',  ( -40.67786913486117584, 6.803913533337310859, 39.48656708792704961 ) ) ;
#21897 = EDGE_LOOP ( 'NONE', ( #9854, #1210, #9999, #24014 ) ) ;
#21898 = CARTESIAN_POINT ( 'NONE',  ( -25.57662701300441555, 14.36454579224780126, 47.04930799450052348 ) ) ;
#21899 = CARTESIAN_POINT ( 'NONE',  ( 33.72499318558949710, 27.59184655352419568, 47.04930799450051637 ) ) ;
#21900 = CARTESIAN_POINT ( 'NONE',  ( 21.09785597605719332, -19.93545420775220123, 132.0493079945005377 ) ) ;
#21901 = CYLINDRICAL_SURFACE ( 'NONE', #11135, 2.500000000000002220 ) ;
#21902 = DIRECTION ( 'NONE',  ( -1.224646799147353207E-16, -1.349345573449484691E-32, 1.000000000000000000 ) ) ;
#21903 = VECTOR ( 'NONE', #21041, 1000.000000000000114 ) ;
#21904 = CARTESIAN_POINT ( 'NONE',  ( -40.23847960488978970, 6.935107575318146367, 34.63465864742641998 ) ) ;
#21905 = DIRECTION ( 'NONE',  ( -1.000000000000000000, 0.000000000000000000, 0.000000000000000000 ) ) ;
#21906 = ORIENTED_EDGE ( 'NONE', *, *, #7680, .T. ) ;
#21907 = DIRECTION ( 'NONE',  ( -0.000000000000000000, -1.000000000000000000, 0.000000000000000000 ) ) ;
#21908 = FACE_OUTER_BOUND ( 'NONE', #23341, .T. ) ;
#21909 = ORIENTED_EDGE ( 'NONE', *, *, #13952, .T. ) ;
#21910 = DIRECTION ( 'NONE',  ( 0.4848096202462280901, 0.8746197071394562483, 0.000000000000000000 ) ) ;
#21911 = DIRECTION ( 'NONE',  ( -1.101824276508909887E-16, 1.000000000000000000, -0.000000000000000000 ) ) ;
#21912 = ORIENTED_EDGE ( 'NONE', *, *, #10892, .T. ) ;
#21913 = EDGE_LOOP ( 'NONE', ( #31818, #17480, #3728, #17502 ) ) ;
#21914 = AXIS2_PLACEMENT_3D ( 'NONE', #21345, #20880, #13670 ) ;
#21915 = UNCERTAINTY_MEASURE_WITH_UNIT (LENGTH_MEASURE( 1.000000000000000082E-05 ), #18546, 'distance_accuracy_value', 'NONE');
#21916 = CIRCLE ( 'NONE', #7784, 12.27641737965288726 ) ;
#21917 = VERTEX_POINT ( 'NONE', #24277 ) ;
#21918 = TOROIDAL_SURFACE ( 'NONE', #6188, 12.61792373059895311, 0.1249999999999983485 ) ;
#21919 = VECTOR ( 'NONE', #28027, 1000.000000000000114 ) ;
#21920 = ADVANCED_FACE ( 'NONE', ( #9343 ), #16884, .T. ) ;
#21921 = AXIS2_PLACEMENT_3D ( 'NONE', #4974, #17104, #2346 ) ;
#21922 = EDGE_CURVE ( 'NONE', #6650, #313, #5517, .T. ) ;
#21923 = CARTESIAN_POINT ( 'NONE',  ( 21.09992658989238734, 38.56284415653841791, 47.04930799450051637 ) ) ;
#21924 = VERTEX_POINT ( 'NONE', #1793 ) ;
#21925 = VERTEX_POINT ( 'NONE', #1947 ) ;
#21926 = DIRECTION ( 'NONE',  ( -1.000000000000000000, 0.000000000000000000, 0.000000000000000000 ) ) ;
#21927 = CARTESIAN_POINT ( 'NONE',  ( 21.09992658989239089, 26.59143805560860940, 47.04930799450051637 ) ) ;
#21928 = DIRECTION ( 'NONE',  ( 0.000000000000000000, -0.000000000000000000, 1.000000000000000000 ) ) ;
#21929 = LINE ( 'NONE', #7506, #22706 ) ;
#21930 = CARTESIAN_POINT ( 'NONE',  ( 48.37829923888483563, 26.79452976649965379, 45.07556196625585443 ) ) ;
#21931 = ORIENTED_EDGE ( 'NONE', *, *, #5359, .T. ) ;
#21932 = CARTESIAN_POINT ( 'NONE',  ( -7.213884129472804219, 8.185031362399401544, 97.59170711626282468 ) ) ;
#21933 = ORIENTED_EDGE ( 'NONE', *, *, #19658, .F. ) ;
#21934 = ORIENTED_EDGE ( 'NONE', *, *, #6183, .F. ) ;
#21935 = DIRECTION ( 'NONE',  ( -1.000000000000000000, 0.000000000000000000, 0.000000000000000000 ) ) ;
#21936 = CARTESIAN_POINT ( 'NONE',  ( -41.10400476907452116, 9.333823787025618657, 35.46646528202590787 ) ) ;
#21937 = AXIS2_PLACEMENT_3D ( 'NONE', #1942, #29038, #32433 ) ;
#21938 = CARTESIAN_POINT ( 'NONE',  ( -42.28293707589220674, 13.65198258188957148, 54.55385885333606666 ) ) ;
#21939 = CARTESIAN_POINT ( 'NONE',  ( 47.60933809039193676, 23.04411619146718238, 48.05197954673941751 ) ) ;
#21940 = CARTESIAN_POINT ( 'NONE',  ( 21.09992658989239089, 27.09143805560860940, 47.04930799450051637 ) ) ;
#21941 = TOROIDAL_SURFACE ( 'NONE', #24550, 1.899999999999999467, 0.1000000000000000056 ) ;
#21942 = CARTESIAN_POINT ( 'NONE',  ( 48.46535932150934656, 26.18954579807170902, 49.73005965046827015 ) ) ;
#21943 = CARTESIAN_POINT ( 'NONE',  ( 21.09785597605719332, 25.18020726757345429, 6.561886094526840907 ) ) ;
#21944 = DIRECTION ( 'NONE',  ( 1.313185983435984691E-29, -1.000000000000000000, -3.761114140369702165E-15 ) ) ;
#21945 = ORIENTED_EDGE ( 'NONE', *, *, #24016, .T. ) ;
#21946 = DIRECTION ( 'NONE',  ( 0.000000000000000000, 1.000000000000000000, 0.000000000000000000 ) ) ;
#21947 = CYLINDRICAL_SURFACE ( 'NONE', #26071, 1.042135311067126979 ) ;
#21948 = CIRCLE ( 'NONE', #12007, 2.000000000000001776 ) ;
#21949 = CARTESIAN_POINT ( 'NONE',  ( 21.09992658989238734, 38.56284415653841791, 47.04930799450051637 ) ) ;
#21950 = LINE ( 'NONE', #12290, #20392 ) ;
#21951 = ORIENTED_EDGE ( 'NONE', *, *, #8229, .F. ) ;
#21952 = EDGE_LOOP ( 'NONE', ( #14370, #10027 ) ) ;
#21953 = DIRECTION ( 'NONE',  ( -1.000000000000000000, 0.000000000000000000, 0.000000000000000000 ) ) ;
#21954 = ORIENTED_EDGE ( 'NONE', *, *, #31143, .F. ) ;
#21955 = CIRCLE ( 'NONE', #16730, 12.62506659569710266 ) ;
#21956 = AXIS2_PLACEMENT_3D ( 'NONE', #29604, #22035, #17446 ) ;
#21957 = ADVANCED_FACE ( 'NONE', ( #24597 ), #9019, .F. ) ;
#21958 = EDGE_CURVE ( 'NONE', #3511, #1048, #25848, .T. ) ;
#21959 = EDGE_CURVE ( 'NONE', #22635, #3066, #26995, .T. ) ;
#21960 = ORIENTED_EDGE ( 'NONE', *, *, #6999, .T. ) ;
#21961 = EDGE_CURVE ( 'NONE', #30111, #8095, #29627, .T. ) ;
#21962 = EDGE_CURVE ( 'NONE', #15585, #26708, #14426, .T. ) ;
#21963 = CARTESIAN_POINT ( 'NONE',  ( 21.09992658989239089, 29.59164230456639899, 47.04930799450051637 ) ) ;
#21964 = CARTESIAN_POINT ( 'NONE',  ( 8.482002859293439556, 28.21664230456639899, 47.04930799450051637 ) ) ;
#21965 = DIRECTION ( 'NONE',  ( -1.101824276508909887E-16, 1.000000000000000000, -0.000000000000000000 ) ) ;
#21966 = AXIS2_PLACEMENT_3D ( 'NONE', #13702, #572, #11081 ) ;
#21967 = VERTEX_POINT ( 'NONE', #1629 ) ;
#21968 = CYLINDRICAL_SURFACE ( 'NONE', #16709, 12.36707279061065279 ) ;
#21969 = DIRECTION ( 'NONE',  ( -1.000000000000000000, 0.000000000000000000, 0.000000000000000000 ) ) ;
#21970 = CARTESIAN_POINT ( 'NONE',  ( 73.78878393608395925, 3.260977705924042347, 15.40761682156110979 ) ) ;
#21971 = EDGE_LOOP ( 'NONE', ( #9612, #31617, #27019, #297 ) ) ;
#21972 = VERTEX_POINT ( 'NONE', #1459 ) ;
#21973 = EDGE_LOOP ( 'NONE', ( #3360, #7119, #26597, #31686 ) ) ;
#21974 = CARTESIAN_POINT ( 'NONE',  ( 21.09992658989239089, 28.96183152705961206, 47.04930799450051637 ) ) ;
#21975 = DIRECTION ( 'NONE',  ( 0.000000000000000000, 0.000000000000000000, 1.000000000000000000 ) ) ;
#21976 = DIRECTION ( 'NONE',  ( 1.000000000000000000, 0.000000000000000000, 0.000000000000000000 ) ) ;
#21977 = CARTESIAN_POINT ( 'NONE',  ( -40.71142685946214357, 9.415924026127871826, 39.52001867261917312 ) ) ;
#21978 = EDGE_CURVE ( 'NONE', #7331, #13945, #4456, .T. ) ;
#21979 =( NAMED_UNIT ( * ) PLANE_ANGLE_UNIT ( ) SI_UNIT ( $, .RADIAN. ) );
#21980 = ORIENTED_EDGE ( 'NONE', *, *, #17148, .T. ) ;
#21981 = ORIENTED_EDGE ( 'NONE', *, *, #19663, .F. ) ;
#21982 = CARTESIAN_POINT ( 'NONE',  ( 76.55093444394998414, -13.30632128221581212, 39.74351294429737180 ) ) ;
#21983 = CIRCLE ( 'NONE', #10485, 1.499999999999994449 ) ;
#21984 = CARTESIAN_POINT ( 'NONE',  ( 9.016997203727582288, 34.59164230456639899, 47.36565641480107303 ) ) ;
#21985 = CIRCLE ( 'NONE', #7858, 0.1250000000000001110 ) ;
#21986 = CARTESIAN_POINT ( 'NONE',  ( -40.68997348041997952, 6.796928795907699161, 60.54930799450051637 ) ) ;
#21987 = ORIENTED_EDGE ( 'NONE', *, *, #19877, .T. ) ;
#21988 = CARTESIAN_POINT ( 'NONE',  ( 21.09785597605719332, 30.56454579224779522, 47.04930799450051637 ) ) ;
#21989 = LINE ( 'NONE', #29725, #11529 ) ;
#21990 = ORIENTED_EDGE ( 'NONE', *, *, #14354, .T. ) ;
#21991 = FACE_OUTER_BOUND ( 'NONE', #26163, .T. ) ;
#21992 = CARTESIAN_POINT ( 'NONE',  ( 46.96268396749378127, 25.43121246473837971, 49.65201805493727960 ) ) ;
#21993 = EDGE_CURVE ( 'NONE', #163, #12910, #15479, .T. ) ;
#21994 = CIRCLE ( 'NONE', #8885, 55.85791022362053582 ) ;
#21995 = CIRCLE ( 'NONE', #16747, 12.36707279061065101 ) ;
#21996 = CARTESIAN_POINT ( 'NONE',  ( -41.07644103349282005, 9.237697617431789965, 39.44930799450052206 ) ) ;
#21997 = AXIS2_PLACEMENT_3D ( 'NONE', #16449, #25980, #31401 ) ;
#21998 = CIRCLE ( 'NONE', #26208, 65.75844861871138392 ) ;
#21999 = CIRCLE ( 'NONE', #20414, 0.2000000000000004274 ) ;
#22000 = ORIENTED_EDGE ( 'NONE', *, *, #20283, .T. ) ;
#22001 = DIRECTION ( 'NONE',  ( -1.101824276508909887E-16, 1.000000000000000000, -0.000000000000000000 ) ) ;
#22002 = EDGE_CURVE ( 'NONE', #593, #22606, #11813, .T. ) ;
#22003 = CARTESIAN_POINT ( 'NONE',  ( 21.09785597605719332, -15.93545420775219945, -25.45069200549945165 ) ) ;
#22004 = DIRECTION ( 'NONE',  ( -1.000000000000000000, 0.000000000000000000, 0.000000000000000000 ) ) ;
#22005 = CARTESIAN_POINT ( 'NONE',  ( 48.16694854572211426, 25.16119643316632093, 49.14507740233662503 ) ) ;
#22006 = ORIENTED_EDGE ( 'NONE', *, *, #3889, .T. ) ;
#22007 = CARTESIAN_POINT ( 'NONE',  ( 21.09785597605719332, -19.93545420775220123, 47.04930799450051637 ) ) ;
#22008 = CARTESIAN_POINT ( 'NONE',  ( 33.72499318558949710, 26.34143805560860940, 47.04930799450051637 ) ) ;
#22009 = CARTESIAN_POINT ( 'NONE',  ( 52.84805770882741882, -5.769399297529544057, -10.43150399477652179 ) ) ;
#22010 = VECTOR ( 'NONE', #8043, 1000.000000000000114 ) ;
#22011 = VECTOR ( 'NONE', #2514, 1000.000000000000000 ) ;
#22012 = DIRECTION ( 'NONE',  ( 0.7141240004913222972, -0.3958453973320028019, -0.5773502691896303940 ) ) ;
#22013 = CARTESIAN_POINT ( 'NONE',  ( -40.68422973805265030, 6.807290781432339344, 39.44930799450052206 ) ) ;
#22014 = DIRECTION ( 'NONE',  ( -1.000000000000000000, 0.000000000000000000, 0.000000000000000000 ) ) ;
#22015 = CARTESIAN_POINT ( 'NONE',  ( -36.75072804420383221, -13.74047052604243646, 54.67070450616914457 ) ) ;
#22016 = FACE_OUTER_BOUND ( 'NONE', #11574, .T. ) ;
#22017 = AXIS2_PLACEMENT_3D ( 'NONE', #14127, #1644, #21821 ) ;
#22018 = EDGE_CURVE ( 'NONE', #2789, #9190, #9182, .T. ) ;
#22019 = CARTESIAN_POINT ( 'NONE',  ( -40.15225626691278649, 6.735663658092487793, 53.64930799450051779 ) ) ;
#22020 = AXIS2_PLACEMENT_3D ( 'NONE', #14537, #2054, #21744 ) ;
#22021 = ORIENTED_EDGE ( 'NONE', *, *, #3618, .F. ) ;
#22022 = AXIS2_PLACEMENT_3D ( 'NONE', #25642, #23182, #7608 ) ;
#22023 = CARTESIAN_POINT ( 'NONE',  ( 45.97377588299919893, 23.04411619146718238, 46.99092872297675427 ) ) ;
#22024 = CARTESIAN_POINT ( 'NONE',  ( -40.39719969963199020, 8.565602912590085438, 34.57497286466457354 ) ) ;
#22025 = EDGE_CURVE ( 'NONE', #29567, #20511, #2364, .T. ) ;
#22026 = CARTESIAN_POINT ( 'NONE',  ( -40.14921103274695469, 6.917687794149811609, 34.55286917618232678 ) ) ;
#22027 = CARTESIAN_POINT ( 'NONE',  ( 54.83597552911822959, -2.474457146986655864, 101.2460582471064328 ) ) ;
#22028 = EDGE_LOOP ( 'NONE', ( #9412, #8456, #2189, #29809 ) ) ;
#22029 = CARTESIAN_POINT ( 'NONE',  ( 21.09992658989239089, 27.59184655352419568, 47.04930799450051637 ) ) ;
#22030 = CARTESIAN_POINT ( 'NONE',  ( -40.13663441551143762, 7.212672898651377729, 38.96029010263398362 ) ) ;
#22031 = DIRECTION ( 'NONE',  ( 0.000000000000000000, 0.000000000000000000, -1.000000000000000000 ) ) ;
#22032 = VERTEX_POINT ( 'NONE', #32325 ) ;
#22033 = ORIENTED_EDGE ( 'NONE', *, *, #12172, .F. ) ;
#22034 = DIRECTION ( 'NONE',  ( -1.000000000000000000, 0.000000000000000000, 0.000000000000000000 ) ) ;
#22035 = DIRECTION ( 'NONE',  ( -0.9612616959383205595, -0.2756373558169932236, 1.660411357259282445E-16 ) ) ;
#22036 = EDGE_CURVE ( 'NONE', #22618, #23145, #27715, .T. ) ;
#22037 = AXIS2_PLACEMENT_3D ( 'NONE', #28421, #27769, #15298 ) ;
#22038 = EDGE_CURVE ( 'NONE', #3892, #24509, #6038, .T. ) ;
#22039 = CARTESIAN_POINT ( 'NONE',  ( -7.324817582041172948, 8.310461108307681144, -12.62465409255485582 ) ) ;
#22040 = LINE ( 'NONE', #31903, #17461 ) ;
#22041 = ORIENTED_EDGE ( 'NONE', *, *, #15559, .F. ) ;
#22042 = DIRECTION ( 'NONE',  ( -0.8746197071393790878, 0.4848096202463673676, 1.277302113040196197E-17 ) ) ;
#22043 = ORIENTED_EDGE ( 'NONE', *, *, #18031, .T. ) ;
#22044 = CIRCLE ( 'NONE', #17326, 0.09999999999998898659 ) ;
#22045 = EDGE_LOOP ( 'NONE', ( #7631, #13574, #13688, #17410 ) ) ;
#22046 = AXIS2_PLACEMENT_3D ( 'NONE', #14415, #23928, #11458 ) ;
#22047 = AXIS2_PLACEMENT_3D ( 'NONE', #17091, #11857, #14812 ) ;
#22048 = CIRCLE ( 'NONE', #16285, 12.62506659569710266 ) ;
#22049 = ADVANCED_FACE ( 'NONE', ( #20160 ), #25430, .T. ) ;
#22050 = CARTESIAN_POINT ( 'NONE',  ( -40.16174044770769314, 7.468546898574136783, 59.44930799450051495 ) ) ;
#22051 = CIRCLE ( 'NONE', #14225, 0.6621856154243876968 ) ;
#22052 = ORIENTED_EDGE ( 'NONE', *, *, #23858, .F. ) ;
#22053 = CARTESIAN_POINT ( 'NONE',  ( -40.02540636251514172, 2.839176264122877047, 57.04930799450051637 ) ) ;
#22054 = CARTESIAN_POINT ( 'NONE',  ( -29.52701465676184611, 10.77837282674672004, 72.12388452301328812 ) ) ;
#22055 = AXIS2_PLACEMENT_3D ( 'NONE', #26652, #19589, #32244 ) ;
#22056 = ORIENTED_EDGE ( 'NONE', *, *, #26083, .F. ) ;
#22057 = FACE_OUTER_BOUND ( 'NONE', #25510, .T. ) ;
#22058 = ORIENTED_EDGE ( 'NONE', *, *, #28830, .F. ) ;
#22059 = DIRECTION ( 'NONE',  ( -1.224646799147353207E-16, -1.349345573449484691E-32, 1.000000000000000000 ) ) ;
#22060 = EDGE_CURVE ( 'NONE', #16834, #11047, #9171, .T. ) ;
#22061 = DIRECTION ( 'NONE',  ( -1.000000000000000000, 0.000000000000000000, 0.000000000000000000 ) ) ;
#22062 = CARTESIAN_POINT ( 'NONE',  ( -40.68455241913549258, 6.798696092114603573, 39.47735115308336162 ) ) ;
#22063 = VERTEX_POINT ( 'NONE', #30345 ) ;
#22064 = CARTESIAN_POINT ( 'NONE',  ( 21.09785597605720042, -17.03545420775220265, 47.04930799450051637 ) ) ;
#22065 = CARTESIAN_POINT ( 'NONE',  ( -40.73091736380679606, 9.483895492497154578, 34.64930799450051779 ) ) ;
#22066 = CARTESIAN_POINT ( 'NONE',  ( -10.00935122521091003, -5.935651417315361833, -13.46746157186161064 ) ) ;
#22067 = EDGE_CURVE ( 'NONE', #25827, #20229, #27396, .T. ) ;
#22068 = CARTESIAN_POINT ( 'NONE',  ( 21.09785597605719332, 17.36451738380053555, 47.04930799450051637 ) ) ;
#22069 = CARTESIAN_POINT ( 'NONE',  ( -40.23847960489091236, 6.935107575317837281, 34.54930799450052348 ) ) ;
#22070 = CARTESIAN_POINT ( 'NONE',  ( 48.23388202445966755, 26.25087065737812253, 49.27628909396054979 ) ) ;
#22071 = EDGE_LOOP ( 'NONE', ( #29226, #14680, #32426, #12945 ) ) ;
#22072 = CIRCLE ( 'NONE', #11103, 12.50967055512594150 ) ;
#22073 = CARTESIAN_POINT ( 'NONE',  ( -40.02661603751052155, 7.039661056838986575, 34.81911587904692595 ) ) ;
#22074 = CARTESIAN_POINT ( 'NONE',  ( -30.89191212020314481, 11.92558985988972964, 26.62456132884095794 ) ) ;
#22075 = ORIENTED_EDGE ( 'NONE', *, *, #29768, .T. ) ;
#22076 = AXIS2_PLACEMENT_3D ( 'NONE', #18111, #556, #22879 ) ;
#22077 = DIRECTION ( 'NONE',  ( 0.9999997877697283100, 0.0006515063303658816165, 0.000000000000000000 ) ) ;
#22078 = VECTOR ( 'NONE', #9277, 1000.000000000000000 ) ;
#22079 = VECTOR ( 'NONE', #6498, 1000.000000000000000 ) ;
#22080 = EDGE_CURVE ( 'NONE', #20020, #8655, #19830, .T. ) ;
#22081 = CARTESIAN_POINT ( 'NONE',  ( 21.09992658989239089, 30.09164230456639544, 47.04930799450051637 ) ) ;
#22082 = ADVANCED_FACE ( 'NONE', ( #22622 ), #22681, .T. ) ;
#22083 = ORIENTED_EDGE ( 'NONE', *, *, #14228, .F. ) ;
#22084 = CIRCLE ( 'NONE', #12138, 0.1249999999999983763 ) ;
#22085 = ORIENTED_EDGE ( 'NONE', *, *, #6487, .F. ) ;
#22086 = AXIS2_PLACEMENT_3D ( 'NONE', #9727, #11532, #21855 ) ;
#22087 = EDGE_LOOP ( 'NONE', ( #3899, #2740, #2423, #20977 ) ) ;
#22088 = AXIS2_PLACEMENT_3D ( 'NONE', #14504, #22695, #9743 ) ;
#22089 = DIRECTION ( 'NONE',  ( 0.9275012328650849014, -0.3738200944756011057, -1.135861416033450161E-16 ) ) ;
#22090 = ORIENTED_EDGE ( 'NONE', *, *, #10244, .T. ) ;
#22091 = VERTEX_POINT ( 'NONE', #20315 ) ;
#22092 = CARTESIAN_POINT ( 'NONE',  ( 78.62428479167849105, -5.811083640285387375, 15.33388578550628090 ) ) ;
#22093 = CARTESIAN_POINT ( 'NONE',  ( 45.84097905237065618, 22.80400562401890241, 48.98672734302541443 ) ) ;
#22094 = LINE ( 'NONE', #29661, #5489 ) ;
#22095 = DIRECTION ( 'NONE',  ( -1.000000000000000000, 0.000000000000000000, 0.000000000000000000 ) ) ;
#22096 = EDGE_CURVE ( 'NONE', #23532, #8765, #23320, .T. ) ;
#22097 = CARTESIAN_POINT ( 'NONE',  ( 21.09785597605720042, -13.56320000832927875, 102.6777340130621639 ) ) ;
#22098 = VERTEX_POINT ( 'NONE', #20807 ) ;
#22099 = DIRECTION ( 'NONE',  ( 1.000000000000000000, 0.000000000000000000, 0.000000000000000000 ) ) ;
#22100 = EDGE_LOOP ( 'NONE', ( #22021, #10899, #5778, #24384 ) ) ;
#22101 = DIRECTION ( 'NONE',  ( 0.000000000000000000, 0.000000000000000000, -1.000000000000000000 ) ) ;
#22102 = CARTESIAN_POINT ( 'NONE',  ( -7.208542748348993001, 8.190330151142697801, -3.492701709236647911 ) ) ;
#22103 = CIRCLE ( 'NONE', #9547, 0.1250000000000001110 ) ;
#22104 = ORIENTED_EDGE ( 'NONE', *, *, #7859, .F. ) ;
#22105 = CARTESIAN_POINT ( 'NONE',  ( -42.37913764077812573, 15.23192269303853053, 35.54930799450051637 ) ) ;
#22106 = DIRECTION ( 'NONE',  ( -1.000000000000000000, 0.000000000000000000, 0.000000000000000000 ) ) ;
#22107 = CARTESIAN_POINT ( 'NONE',  ( -42.24141723705587737, 13.63285518870473290, 54.54930799450051637 ) ) ;
#22108 = LINE ( 'NONE', #25069, #10574 ) ;
#22109 = DIRECTION ( 'NONE',  ( -1.000000000000000000, -1.101824276508909887E-16, 0.000000000000000000 ) ) ;
#22110 = CARTESIAN_POINT ( 'NONE',  ( 48.73570333863616355, 25.02287913140504827, 44.52463952959527660 ) ) ;
#22111 = CARTESIAN_POINT ( 'NONE',  ( 46.79153437246152691, 23.10527845304106265, 47.52148899368456370 ) ) ;
#22112 = CARTESIAN_POINT ( 'NONE',  ( 75.19785597605721250, 14.36454579224779948, 47.04930799450051637 ) ) ;
#22113 = ORIENTED_EDGE ( 'NONE', *, *, #29460, .F. ) ;
#22114 = DIRECTION ( 'NONE',  ( 0.000000000000000000, 0.000000000000000000, -1.000000000000000000 ) ) ;
#22115 = LINE ( 'NONE', #14581, #18753 ) ;
#22116 = CARTESIAN_POINT ( 'NONE',  ( 21.09992658989239089, 26.09164230456639899, 47.04930799450051637 ) ) ;
#22117 = EDGE_CURVE ( 'NONE', #26412, #29942, #24363, .T. ) ;
#22118 = TOROIDAL_SURFACE ( 'NONE', #31637, 12.40141737965283930, 0.1250000000000007216 ) ;
#22119 = CARTESIAN_POINT ( 'NONE',  ( -40.65120636623950645, 8.087130829066872195, 57.04930799450051637 ) ) ;
#22120 = DIRECTION ( 'NONE',  ( -0.9612616959383194493, -0.2756373558169972759, -8.795445018804905742E-19 ) ) ;
#22121 = ORIENTED_EDGE ( 'NONE', *, *, #30755, .F. ) ;
#22122 = AXIS2_PLACEMENT_3D ( 'NONE', #24837, #20227, #17107 ) ;
#22123 = ORIENTED_EDGE ( 'NONE', *, *, #10805, .T. ) ;
#22124 = DIRECTION ( 'NONE',  ( -1.000000000000000000, 0.000000000000000000, 0.000000000000000000 ) ) ;
#22125 = EDGE_LOOP ( 'NONE', ( #20121, #20726, #28971, #9768 ) ) ;
#22126 = B_SPLINE_CURVE_WITH_KNOTS ( 'NONE', 3,
 ( #27920, #14965, #17246, #27261, #5437, #12674, #20037, #9872 ),
 .UNSPECIFIED., .F., .F.,
 ( 4, 2, 2, 4 ),
 ( 1.743375517060540341E-17, 0.0003981837892567215891, 0.0007963675785134257225, 0.001592735157026818702 ),
 .UNSPECIFIED. ) ;
#22127 = CIRCLE ( 'NONE', #21604, 12.36707279061065101 ) ;
#22128 = VERTEX_POINT ( 'NONE', #28043 ) ;
#22129 = CIRCLE ( 'NONE', #17428, 12.98419020052701889 ) ;
#22130 = DIRECTION ( 'NONE',  ( -0.9612616959383221138, -0.2756373558169876170, 0.000000000000000000 ) ) ;
#22131 = CARTESIAN_POINT ( 'NONE',  ( 21.09785597605719332, -9.935454207752199451, 47.04930799450051637 ) ) ;
#22132 = AXIS2_PLACEMENT_3D ( 'NONE', #24739, #19968, #17173 ) ;
#22133 = VERTEX_POINT ( 'NONE', #20486 ) ;
#22134 = DIRECTION ( 'NONE',  ( 0.000000000000000000, 1.000000000000000000, 0.000000000000000000 ) ) ;
#22135 = AXIS2_PLACEMENT_3D ( 'NONE', #4811, #14833, #2352 ) ;
#22136 = CARTESIAN_POINT ( 'NONE',  ( 21.09992658989238734, 31.46183152705961561, 47.04930799450051637 ) ) ;
#22137 = CARTESIAN_POINT ( 'NONE',  ( 21.09992658989239089, 27.46183152705960850, 47.04930799450051637 ) ) ;
#22138 = CARTESIAN_POINT ( 'NONE',  ( 48.18662509608405031, 25.79624452788248945, 49.18364984542562013 ) ) ;
#22139 = VERTEX_POINT ( 'NONE', #30830 ) ;
#22140 = EDGE_LOOP ( 'NONE', ( #28404, #18491, #12147, #30224 ) ) ;
#22141 = CARTESIAN_POINT ( 'NONE',  ( 106.0978559760575735, 1.925589859889728972, 26.63511333407112502 ) ) ;
#22142 = ORIENTED_EDGE ( 'NONE', *, *, #28673, .F. ) ;
#22143 = DIRECTION ( 'NONE',  ( -3.761114140369701376E-15, -1.000000000000000000, -0.000000000000000000 ) ) ;
#22144 = DIRECTION ( 'NONE',  ( -1.000000000000000000, 0.000000000000000000, 0.000000000000000000 ) ) ;
#22145 = DIRECTION ( 'NONE',  ( 0.000000000000000000, 0.000000000000000000, 1.000000000000000000 ) ) ;
#22146 = CARTESIAN_POINT ( 'NONE',  ( 21.09785597605719332, -15.43545420775221366, 119.0493079945005093 ) ) ;
#22147 = CARTESIAN_POINT ( 'NONE',  ( 46.00908685603033632, 28.94624452788248092, 44.91496614357595263 ) ) ;
#22148 = CARTESIAN_POINT ( 'NONE',  ( -14.77419368316019366, 6.938893903907228378E-15, 22.47910467279100288 ) ) ;
#22149 = VERTEX_POINT ( 'NONE', #23433 ) ;
#22150 = ORIENTED_EDGE ( 'NONE', *, *, #17236, .F. ) ;
#22151 = CARTESIAN_POINT ( 'NONE',  ( -42.50976151518963064, 14.59907569580870224, 35.90717268343339441 ) ) ;
#22152 = LINE ( 'NONE', #16906, #14602 ) ;
#22153 = ADVANCED_FACE ( 'NONE', ( #23279 ), #27515, .T. ) ;
#22154 = ADVANCED_FACE ( 'NONE', ( #3564 ), #5665, .F. ) ;
#22155 = CARTESIAN_POINT ( 'NONE',  ( -40.69343167531472005, 8.234387981831414294, 59.54930799450052348 ) ) ;
#22156 = ADVANCED_FACE ( 'NONE', ( #28678 ), #16195, .T. ) ;
#22157 = CIRCLE ( 'NONE', #9590, 12.62506659569710266 ) ;
#22158 = ADVANCED_FACE ( 'NONE', ( #18338 ), #28201, .T. ) ;
#22159 = ORIENTED_EDGE ( 'NONE', *, *, #22863, .F. ) ;
#22160 = CARTESIAN_POINT ( 'NONE',  ( 45.24946171279598417, 27.10784706826093071, 47.99220971130007740 ) ) ;
#22161 = CARTESIAN_POINT ( 'NONE',  ( 48.86248627303584158, 22.86454579224779948, 46.10725065118596433 ) ) ;
#22162 = EDGE_CURVE ( 'NONE', #16662, #27962, #13377, .T. ) ;
#22163 = CIRCLE ( 'NONE', #8011, 15.23374605753642186 ) ;
#22164 = ORIENTED_EDGE ( 'NONE', *, *, #407, .T. ) ;
#22165 = DIRECTION ( 'NONE',  ( -0.000000000000000000, -1.000000000000000000, 0.000000000000000000 ) ) ;
#22166 = DIRECTION ( 'NONE',  ( 0.000000000000000000, 1.000000000000000000, 0.000000000000000000 ) ) ;
#22167 = FACE_OUTER_BOUND ( 'NONE', #28562, .T. ) ;
#22168 = AXIS2_PLACEMENT_3D ( 'NONE', #27203, #4727, #128 ) ;
#22169 = VERTEX_POINT ( 'NONE', #788 ) ;
#22170 = ORIENTED_EDGE ( 'NONE', *, *, #8021, .T. ) ;
#22171 = CARTESIAN_POINT ( 'NONE',  ( -40.06561427811386267, 7.496110634155836117, 60.54930799450051637 ) ) ;
#22172 = FACE_OUTER_BOUND ( 'NONE', #25556, .T. ) ;
#22173 = CARTESIAN_POINT ( 'NONE',  ( 45.35708200440645044, 26.99118040159426357, 45.92000246470679770 ) ) ;
#22174 = ORIENTED_EDGE ( 'NONE', *, *, #11980, .T. ) ;
#22175 = CIRCLE ( 'NONE', #24812, 12.62506659569710443 ) ;
#22176 = DIRECTION ( 'NONE',  ( -1.224646799147353207E-16, -1.349345573449484691E-32, 1.000000000000000000 ) ) ;
#22177 = CARTESIAN_POINT ( 'NONE',  ( 45.52675994804781112, 27.41155426599985034, 49.47108226228597516 ) ) ;
#22178 = ADVANCED_FACE ( 'NONE', ( #8663 ), #24890, .T. ) ;
#22179 = CARTESIAN_POINT ( 'NONE',  ( 50.24971918728039100, 7.161243906346019372, -3.668688982869140691 ) ) ;
#22180 = DIRECTION ( 'NONE',  ( 0.000000000000000000, -1.000000000000000000, 0.000000000000000000 ) ) ;
#22181 = DIRECTION ( 'NONE',  ( -0.4848096202463430537, -0.8746197071393926326, -9.920727850371701658E-18 ) ) ;
#22182 = DIRECTION ( 'NONE',  ( -1.000000000000000000, 0.000000000000000000, 0.000000000000000000 ) ) ;
#22183 = CARTESIAN_POINT ( 'NONE',  ( 21.09785597605719332, -16.63545420775219696, -34.66074251183835031 ) ) ;
#22184 = DIRECTION ( 'NONE',  ( -0.9761574614375592152, 0.2110602665713099957, -0.05069688703093822024 ) ) ;
#22185 = CIRCLE ( 'NONE', #24801, 12.62506659569710443 ) ;
#22186 = AXIS2_PLACEMENT_3D ( 'NONE', #8009, #18007, #5544 ) ;
#22187 = CYLINDRICAL_SURFACE ( 'NONE', #14443, 12.36707279061065101 ) ;
#22188 = LINE ( 'NONE', #10060, #22620 ) ;
#22189 = ORIENTED_EDGE ( 'NONE', *, *, #30031, .T. ) ;
#22190 = VERTEX_POINT ( 'NONE', #22940 ) ;
#22191 = DIRECTION ( 'NONE',  ( -1.000000000000000000, 0.000000000000000000, 0.000000000000000000 ) ) ;
#22192 = DIRECTION ( 'NONE',  ( 0.000000000000000000, 0.000000000000000000, 1.000000000000000000 ) ) ;
#22193 = CARTESIAN_POINT ( 'NONE',  ( -30.47008420211899349, 11.87742387770962615, 25.50481123865409216 ) ) ;
#22194 = EDGE_CURVE ( 'NONE', #9438, #11793, #10755, .T. ) ;
#22195 = CARTESIAN_POINT ( 'NONE',  ( 46.55854765242722948, 27.26960992152947938, 44.51792966461572121 ) ) ;
#22196 = EDGE_CURVE ( 'NONE', #20369, #25423, #785, .T. ) ;
#22197 = EDGE_CURVE ( 'NONE', #21385, #7469, #31707, .T. ) ;
#22198 = ORIENTED_EDGE ( 'NONE', *, *, #28029, .T. ) ;
#22199 = DIRECTION ( 'NONE',  ( -1.101824276508909887E-16, 1.000000000000000000, -0.000000000000000000 ) ) ;
#22200 = CYLINDRICAL_SURFACE ( 'NONE', #22122, 12.08499999999999730 ) ;
#22201 = DIRECTION ( 'NONE',  ( -1.000000000000000000, -1.101824276508909887E-16, 0.000000000000000000 ) ) ;
#22202 = ORIENTED_EDGE ( 'NONE', *, *, #32119, .F. ) ;
#22203 = EDGE_LOOP ( 'NONE', ( #12918, #29036, #4714, #5226 ) ) ;
#22204 = FACE_OUTER_BOUND ( 'NONE', #24966, .T. ) ;
#22205 = EDGE_CURVE ( 'NONE', #4851, #19129, #11799, .T. ) ;
#22206 = DIRECTION ( 'NONE',  ( -1.224646799147353207E-16, -1.349345573449484691E-32, 1.000000000000000000 ) ) ;
#22207 = LINE ( 'NONE', #19738, #27252 ) ;
#22208 = CARTESIAN_POINT ( 'NONE',  ( 21.09785597605720753, 15.19538130838178169, 47.04930799450052348 ) ) ;
#22209 = CARTESIAN_POINT ( 'NONE',  ( 8.482002859293421793, 26.46664230456639899, 47.04930799450051637 ) ) ;
#22210 = ORIENTED_EDGE ( 'NONE', *, *, #3712, .F. ) ;
#22211 = ORIENTED_EDGE ( 'NONE', *, *, #6844, .F. ) ;
#22212 = AXIS2_PLACEMENT_3D ( 'NONE', #28991, #27165, #1409 ) ;
#22213 = CARTESIAN_POINT ( 'NONE',  ( -38.22549819199227272, 15.91524478274158483, 59.54930799450050927 ) ) ;
#22214 = VERTEX_POINT ( 'NONE', #5717 ) ;
#22215 = PLANE ( 'NONE',  #19179 ) ;
#22216 = CYLINDRICAL_SURFACE ( 'NONE', #26082, 12.36707279061065101 ) ;
#22217 = EDGE_CURVE ( 'NONE', #9700, #30206, #15723, .T. ) ;
#22218 = EDGE_CURVE ( 'NONE', #31343, #17323, #29033, .T. ) ;
#22219 = ORIENTED_EDGE ( 'NONE', *, *, #21702, .T. ) ;
#22220 = CARTESIAN_POINT ( 'NONE',  ( -40.81568357405034675, 8.445604592586153814, 34.57497286466457354 ) ) ;
#22221 = ORIENTED_EDGE ( 'NONE', *, *, #15453, .F. ) ;
#22222 = CARTESIAN_POINT ( 'NONE',  ( -41.88090303775678080, 13.82677487427665497, 59.44930799450051495 ) ) ;
#22223 = AXIS2_PLACEMENT_3D ( 'NONE', #16760, #19217, #31393 ) ;
#22224 = FACE_OUTER_BOUND ( 'NONE', #12623, .T. ) ;
#22225 = CARTESIAN_POINT ( 'NONE',  ( 21.09785597605719332, 12.39166260509097484, 47.04930799450051637 ) ) ;
#22226 = ORIENTED_EDGE ( 'NONE', *, *, #2118, .F. ) ;
#22227 = DIRECTION ( 'NONE',  ( -0.8746197071393790878, 0.4848096202463673676, 1.277302113040196197E-17 ) ) ;
#22228 = FACE_OUTER_BOUND ( 'NONE', #9257, .T. ) ;
#22229 = CARTESIAN_POINT ( 'NONE',  ( 21.09992658989238734, 38.56284415653841791, 47.04930799450051637 ) ) ;
#22230 = DIRECTION ( 'NONE',  ( -1.000000000000000000, 0.000000000000000000, 0.000000000000000000 ) ) ;
#22231 = CARTESIAN_POINT ( 'NONE',  ( 33.50134396954521065, 29.84164230456639899, 47.04930799450051637 ) ) ;
#22232 = TOROIDAL_SURFACE ( 'NONE', #8102, 26.49999999999999645, 0.9999999999999956701 ) ;
#22233 = CARTESIAN_POINT ( 'NONE',  ( 72.46310410352278097, 9.702389020015065313, 73.75010705023584023 ) ) ;
#22234 = ORIENTED_EDGE ( 'NONE', *, *, #17407, .T. ) ;
#22235 = CARTESIAN_POINT ( 'NONE',  ( 33.50134396954522487, 29.09164230456639899, 47.04930799450051637 ) ) ;
#22236 = CARTESIAN_POINT ( 'NONE',  ( -36.76418579970419387, 10.14130568307076352, 57.04930799450051637 ) ) ;
#22237 = VERTEX_POINT ( 'NONE', #21601 ) ;
#22238 = EDGE_CURVE ( 'NONE', #28492, #8138, #27146, .T. ) ;
#22239 = CARTESIAN_POINT ( 'NONE',  ( -40.18454328187963398, 7.548069831825862330, 60.44930799450051495 ) ) ;
#22240 = CARTESIAN_POINT ( 'NONE',  ( 8.698509210239576461, 31.34164230456639544, 47.04930799450051637 ) ) ;
#22241 = ORIENTED_EDGE ( 'NONE', *, *, #29805, .F. ) ;
#22242 = EDGE_LOOP ( 'NONE', ( #17057, #31262, #23228, #7400 ) ) ;
#22243 = ORIENTED_EDGE ( 'NONE', *, *, #28793, .F. ) ;
#22244 = AXIS2_PLACEMENT_3D ( 'NONE', #27597, #2488, #17088 ) ;
#22245=STYLED_ITEM('',(#32529),#1196);
#22246 = ADVANCED_FACE ( 'NONE', ( #26373 ), #1906, .F. ) ;
#22247 = CIRCLE ( 'NONE', #8115, 12.98419020052702599 ) ;
#22248 = AXIS2_PLACEMENT_3D ( 'NONE', #11616, #9804, #14404 ) ;
#22249 = CIRCLE ( 'NONE', #7614, 58.84990142703892246 ) ;
#22250 = EDGE_CURVE ( 'NONE', #14305, #18233, #20873, .T. ) ;
#22251 = CARTESIAN_POINT ( 'NONE',  ( 45.00053793792376666, 25.83655426599985816, 45.68869892245983522 ) ) ;
#22252 = EDGE_CURVE ( 'NONE', #14096, #30366, #29494, .T. ) ;
#22253 = ADVANCED_FACE ( 'NONE', ( #29319 ), #4216, .T. ) ;
#22254 = VERTEX_POINT ( 'NONE', #16355 ) ;
#22255 = ORIENTED_EDGE ( 'NONE', *, *, #1932, .F. ) ;
#22256 = CARTESIAN_POINT ( 'NONE',  ( 75.66689018375404885, -3.025068871688612937, 13.33232285377167337 ) ) ;
#22257 = ADVANCED_FACE ( 'NONE', ( #3730 ), #6842, .F. ) ;
#22258 = DIRECTION ( 'NONE',  ( -1.000000000000000000, 0.000000000000000000, 0.000000000000000000 ) ) ;
#22259 = CARTESIAN_POINT ( 'NONE',  ( 33.46699938050304013, 29.21183152705961206, 47.04930799450051637 ) ) ;
#22260 = CARTESIAN_POINT ( 'NONE',  ( -42.54104507194909957, 14.67778162788815344, 59.54930799450050927 ) ) ;
#22261 = DIRECTION ( 'NONE',  ( 1.000000000000000000, 0.000000000000000000, 0.000000000000000000 ) ) ;
#22262 = EDGE_LOOP ( 'NONE', ( #12134, #6551, #5159, #8990 ) ) ;
#22263 = CARTESIAN_POINT ( 'NONE',  ( -38.44000803836371460, -5.928063154200345686, 78.12747986390417054 ) ) ;
#22264 = ORIENTED_EDGE ( 'NONE', *, *, #32441, .T. ) ;
#22265 = CARTESIAN_POINT ( 'NONE',  ( -30.89758657727378832, 5.676337878349658972, 16.86309542392945104 ) ) ;
#22266 = CARTESIAN_POINT ( 'NONE',  ( -41.10316901461906980, 9.481183992871798694, 35.54930799450051637 ) ) ;
#22267 = VERTEX_POINT ( 'NONE', #24393 ) ;
#22268 = FACE_OUTER_BOUND ( 'NONE', #29064, .T. ) ;
#22269 = CARTESIAN_POINT ( 'NONE',  ( 21.09992658989239089, 23.59164230456639544, 47.04930799450051637 ) ) ;
#22270 = FACE_OUTER_BOUND ( 'NONE', #10162, .T. ) ;
#22271 = DIRECTION ( 'NONE',  ( -0.000000000000000000, -1.000000000000000000, 0.000000000000000000 ) ) ;
#22272 = DIRECTION ( 'NONE',  ( 0.000000000000000000, 0.000000000000000000, 1.000000000000000000 ) ) ;
#22273 = CARTESIAN_POINT ( 'NONE',  ( 46.00908685603034343, 26.84624452788248661, 44.91496614357595263 ) ) ;
#22274 = AXIS2_PLACEMENT_3D ( 'NONE', #14447, #17378, #6892 ) ;
#22275 = CARTESIAN_POINT ( 'NONE',  ( 21.09785597605720753, 14.61319044934410627, 47.04930799450052348 ) ) ;
#22276 = DIRECTION ( 'NONE',  ( -0.2756373558169973870, 0.9612616959383193382, 1.315048337272770280E-17 ) ) ;
#22277 = VECTOR ( 'NONE', #8392, 1000.000000000000000 ) ;
#22278 = EDGE_LOOP ( 'NONE', ( #30524, #2731, #27478, #26180 ) ) ;
#22279 = ADVANCED_FACE ( 'NONE', ( #23910 ), #29162, .F. ) ;
#22280 = CARTESIAN_POINT ( 'NONE',  ( 47.12873084020358760, 29.59659471728345181, 44.98158648324610454 ) ) ;
#22281 = DIRECTION ( 'NONE',  ( -1.000000000000000000, -1.101824276508909887E-16, 0.000000000000000000 ) ) ;
#22282 = AXIS2_PLACEMENT_3D ( 'NONE', #13255, #6014, #10788 ) ;
#22283 = ORIENTED_EDGE ( 'NONE', *, *, #6346, .T. ) ;
#22284 = VECTOR ( 'NONE', #6493, 1000.000000000000114 ) ;
#22285 = CIRCLE ( 'NONE', #11302, 0.1250000000000001110 ) ;
#22286 = DIRECTION ( 'NONE',  ( -0.000000000000000000, -1.000000000000000000, 0.000000000000000000 ) ) ;
#22287 = CARTESIAN_POINT ( 'NONE',  ( -39.85048242108726413, 2.742214340073605872, 47.04930799450051637 ) ) ;
#22288 = VERTEX_POINT ( 'NONE', #14237 ) ;
#22289 = ORIENTED_EDGE ( 'NONE', *, *, #5190, .T. ) ;
#22290 = DIRECTION ( 'NONE',  ( -1.000000000000000000, -1.101824276508909764E-16, 0.000000000000000000 ) ) ;
#22291 = EDGE_LOOP ( 'NONE', ( #15407, #25093, #10868, #24022 ) ) ;
#22292 = ADVANCED_FACE ( 'NONE', ( #7001 ), #16997, .T. ) ;
#22293 = EDGE_CURVE ( 'NONE', #27591, #21064, #1583, .T. ) ;
#22294 = CIRCLE ( 'NONE', #13349, 12.52247886585643677 ) ;
#22295 =( BOUNDED_SURFACE ( )  B_SPLINE_SURFACE ( 1, 2, ( 
 ( #11708, #7103, #26633, #4145, #29257, #4638, #14175, #14659, #21699, #24665, #27289, #1850, #19727 ),
 ( #2343, #21861, #19404, #6940, #24832, #16938, #4479, #31731, #14497, #12199, #24491, #7271, #17266 ) ),
 .UNSPECIFIED., .F., .F., .F. ) 
 B_SPLINE_SURFACE_WITH_KNOTS ( ( 2, 2 ),
 ( 3, 2, 2, 2, 2, 2, 3 ),
 ( 0.000000000000000000, 1.000000000000000000 ),
 ( 0.000000000000000000, 0.1666666666666666574, 0.3333333333333333148, 0.5000000000000000000, 0.6666666666666666297, 0.8333333333333333703, 1.000000000000000000 ),
 .UNSPECIFIED. ) 
 GEOMETRIC_REPRESENTATION_ITEM ( )  RATIONAL_B_SPLINE_SURFACE ( (
 ( 1.000000000000000000, 0.8660254037844387076, 1.000000000000000000, 0.8660254037844387076, 1.000000000000000000, 0.8660254037844387076, 1.000000000000000000, 0.8660254037844387076, 1.000000000000000000, 0.8660254037844387076, 1.000000000000000000, 0.8660254037844387076, 1.000000000000000000),
 ( 1.000000000000000000, 0.8660254037844387076, 1.000000000000000000, 0.8660254037844387076, 1.000000000000000000, 0.8660254037844387076, 1.000000000000000000, 0.8660254037844387076, 1.000000000000000000, 0.8660254037844387076, 1.000000000000000000, 0.8660254037844387076, 1.000000000000000000) ) ) 
 REPRESENTATION_ITEM ( '' )  SURFACE ( )  );
#22296 = VERTEX_POINT ( 'NONE', #13750 ) ;
#22297 = DIRECTION ( 'NONE',  ( 0.2756373558169976645, -0.9612616959383194493, 1.479773560108259753E-16 ) ) ;
#22298 = CARTESIAN_POINT ( 'NONE',  ( -40.50720532202722524, 7.584939507552746818, 54.01510846932454513 ) ) ;
#22299 = AXIS2_PLACEMENT_3D ( 'NONE', #17756, #17265, #4804 ) ;
#22300 = EDGE_CURVE ( 'NONE', #7753, #30447, #8295, .T. ) ;
#22301 = AXIS2_PLACEMENT_3D ( 'NONE', #3489, #21046, #30759 ) ;
#22302 = ORIENTED_EDGE ( 'NONE', *, *, #21152, .F. ) ;
#22303 = ADVANCED_FACE ( 'NONE', ( #26536 ), #9138, .F. ) ;
#22304 = FACE_OUTER_BOUND ( 'NONE', #28825, .T. ) ;
#22305 = DIRECTION ( 'NONE',  ( -0.000000000000000000, -1.000000000000000000, -0.000000000000000000 ) ) ;
#22306 = CARTESIAN_POINT ( 'NONE',  ( 49.40414881150629611, 22.80400562401889530, 47.16908566558144855 ) ) ;
#22307 = CARTESIAN_POINT ( 'NONE',  ( 47.20547626766766314, 27.48791119454915233, 44.97710074790751378 ) ) ;
#22308 = ORIENTED_EDGE ( 'NONE', *, *, #1166, .F. ) ;
#22309 = ORIENTED_EDGE ( 'NONE', *, *, #18692, .F. ) ;
#22310 = CARTESIAN_POINT ( 'NONE',  ( 52.09785597605720397, -5.098646251524523443, 47.04930799450051637 ) ) ;
#22311 = ORIENTED_EDGE ( 'NONE', *, *, #18192, .F. ) ;
#22312 = CIRCLE ( 'NONE', #6596, 1.000000000000000666 ) ;
#22313 = CARTESIAN_POINT ( 'NONE',  ( 21.09992658989238734, 32.59164230456639899, 47.04930799450051637 ) ) ;
#22314 = DIRECTION ( 'NONE',  ( -1.000000000000000000, -1.101824276508909764E-16, 0.000000000000000000 ) ) ;
#22315 = CARTESIAN_POINT ( 'NONE',  ( 21.09992658989238734, 38.56284415653841791, 47.04930799450051637 ) ) ;
#22316 = CARTESIAN_POINT ( 'NONE',  ( 33.46699938050304013, 26.97145308207318948, 47.04930799450050927 ) ) ;
#22317 = CARTESIAN_POINT ( 'NONE',  ( 47.20547626766765603, 28.88791119454915091, 44.97710074790751378 ) ) ;
#22318 = ORIENTED_EDGE ( 'NONE', *, *, #28617, .T. ) ;
#22319 = ORIENTED_EDGE ( 'NONE', *, *, #30298, .T. ) ;
#22320 = LINE ( 'NONE', #2627, #29668 ) ;
#22321 = FACE_OUTER_BOUND ( 'NONE', #15835, .T. ) ;
#22322 = FACE_BOUND ( 'NONE', #23519, .T. ) ;
#22323 = ORIENTED_EDGE ( 'NONE', *, *, #7781, .F. ) ;
#22324 = CARTESIAN_POINT ( 'NONE',  ( 44.70507715278255034, 29.14951373492759146, 46.92503878583765697 ) ) ;
#22325 = CARTESIAN_POINT ( 'NONE',  ( 21.09785597605720753, -13.87844638871996850, 106.4909947499981513 ) ) ;
#22326 = ORIENTED_EDGE ( 'NONE', *, *, #21150, .T. ) ;
#22327 = CARTESIAN_POINT ( 'NONE',  ( 21.09785597605720753, 14.86454579224779948, 47.04930799450052348 ) ) ;
#22328 = DIRECTION ( 'NONE',  ( -1.101824276508909887E-16, 1.000000000000000000, -0.000000000000000000 ) ) ;
#22329 = CIRCLE ( 'NONE', #12387, 54.10000000000000142 ) ;
#22330 =( GEOMETRIC_REPRESENTATION_CONTEXT ( 3 ) GLOBAL_UNCERTAINTY_ASSIGNED_CONTEXT ( ( #23270 ) ) GLOBAL_UNIT_ASSIGNED_CONTEXT ( ( #13173, #11026, #1156 ) ) REPRESENTATION_CONTEXT ( 'NONE', 'WORKASPACE' ) );
#22331 = FACE_OUTER_BOUND ( 'NONE', #7389, .T. ) ;
#22332 = AXIS2_PLACEMENT_3D ( 'NONE', #27805, #24853, #27634 ) ;
#22333 = ORIENTED_EDGE ( 'NONE', *, *, #6772, .F. ) ;
#22334 = ORIENTED_EDGE ( 'NONE', *, *, #6185, .F. ) ;
#22335 = DIRECTION ( 'NONE',  ( 0.000000000000000000, 1.000000000000000000, 0.000000000000000000 ) ) ;
#22336 = DIRECTION ( 'NONE',  ( -0.000000000000000000, -1.000000000000000000, 0.000000000000000000 ) ) ;
#22337 = EDGE_CURVE ( 'NONE', #18639, #7358, #1298, .T. ) ;
#22338 = VERTEX_POINT ( 'NONE', #6516 ) ;
#22339 = CYLINDRICAL_SURFACE ( 'NONE', #22244, 1.500000000000001332 ) ;
#22340 = DIRECTION ( 'NONE',  ( 0.000000000000000000, 0.000000000000000000, -1.000000000000000000 ) ) ;
#22341 = AXIS2_PLACEMENT_3D ( 'NONE', #19323, #14419, #11461 ) ;
#22342 = CARTESIAN_POINT ( 'NONE',  ( 53.40509610059028489, 2.044662169668915563, -5.087510015872766189 ) ) ;
#22343 = CARTESIAN_POINT ( 'NONE',  ( 21.09992658989238734, 31.71183152705962272, 47.04930799450051637 ) ) ;
#22344 = DIRECTION ( 'NONE',  ( 1.000000000000000000, 0.000000000000000000, 0.000000000000000000 ) ) ;
#22345 = CARTESIAN_POINT ( 'NONE',  ( -40.50146157965988891, 7.595301493077381672, 34.64930799450051779 ) ) ;
#22346 = CARTESIAN_POINT ( 'NONE',  ( 21.09785597605720753, -5.098646251524523443, 47.04930799450052348 ) ) ;
#22347 = CARTESIAN_POINT ( 'NONE',  ( -41.57366591477001805, 14.83385496645368384, 37.04930799450052348 ) ) ;
#22348 = CARTESIAN_POINT ( 'NONE',  ( 8.732853799281734553, 38.56284415653841791, 47.04930799450051637 ) ) ;
#22349 = DIRECTION ( 'NONE',  ( -1.101824276508909887E-16, 1.000000000000000000, -0.000000000000000000 ) ) ;
#22350 =( NAMED_UNIT ( * ) SI_UNIT ( $, .STERADIAN. ) SOLID_ANGLE_UNIT ( ) );
#22351 = ORIENTED_EDGE ( 'NONE', *, *, #22379, .F. ) ;
#22352 = ORIENTED_EDGE ( 'NONE', *, *, #10445, .F. ) ;
#22353 = CARTESIAN_POINT ( 'NONE',  ( -40.02540636251514172, 2.839176264122877047, 57.04930799450051637 ) ) ;
#22354 = PLANE ( 'NONE',  #23506 ) ;
#22355 = DIRECTION ( 'NONE',  ( 0.000000000000000000, 0.000000000000000000, -1.000000000000000000 ) ) ;
#22356 = CIRCLE ( 'NONE', #32327, 84.50000000000002842 ) ;
#22357 = CARTESIAN_POINT ( 'NONE',  ( 53.43087011377310347, -5.485531640240836282, 104.0244910283431494 ) ) ;
#22358 = ORIENTED_EDGE ( 'NONE', *, *, #30484, .F. ) ;
#22359 = DIRECTION ( 'NONE',  ( -1.000000000000000000, 0.000000000000000000, 0.000000000000000000 ) ) ;
#22360 = CARTESIAN_POINT ( 'NONE',  ( -40.18454328187963398, 7.548069831825863218, 60.54930799450051637 ) ) ;
#22361 = CARTESIAN_POINT ( 'NONE',  ( -40.99980536824363497, 9.333232819382775602, 39.52001867261917312 ) ) ;
#22362 = VERTEX_POINT ( 'NONE', #26693 ) ;
#22363 = EDGE_LOOP ( 'NONE', ( #10323, #4005, #20115, #31217 ) ) ;
#22364 = DIRECTION ( 'NONE',  ( 0.9612616959383205595, 0.2756373558169932236, -1.660411357259282445E-16 ) ) ;
#22365 = CARTESIAN_POINT ( 'NONE',  ( 48.40186567930498285, 28.91618040159426073, 45.03923535223908203 ) ) ;
#22366 = DIRECTION ( 'NONE',  ( -1.000000000000000000, 0.000000000000000000, 0.000000000000000000 ) ) ;
#22367 = CYLINDRICAL_SURFACE ( 'NONE', #27964, 12.62506659569710443 ) ;
#22368 = DIRECTION ( 'NONE',  ( -1.000000000000000000, 0.000000000000000000, 0.000000000000000000 ) ) ;
#22369 = ORIENTED_EDGE ( 'NONE', *, *, #22374, .T. ) ;
#22370 = ORIENTED_EDGE ( 'NONE', *, *, #27314, .F. ) ;
#22371 = DIRECTION ( 'NONE',  ( -1.000000000000000000, -1.101824276508909764E-16, 0.000000000000000000 ) ) ;
#22372 = EDGE_LOOP ( 'NONE', ( #30286, #20957, #29085, #3692 ) ) ;
#22373 = EDGE_CURVE ( 'NONE', #26808, #6349, #3558, .T. ) ;
#22374 = EDGE_CURVE ( 'NONE', #4784, #13945, #21762, .T. ) ;
#22375 = EDGE_CURVE ( 'NONE', #18804, #28622, #12097, .T. ) ;
#22376 = EDGE_CURVE ( 'NONE', #20809, #11333, #25079, .T. ) ;
#22377 = CARTESIAN_POINT ( 'NONE',  ( -41.23380787120766655, 11.23768311167744294, 37.04930799450052348 ) ) ;
#22378 = CARTESIAN_POINT ( 'NONE',  ( 21.09992658989238734, 30.84164230456639544, 47.04930799450051637 ) ) ;
#22379 = EDGE_CURVE ( 'NONE', #29498, #13639, #10903, .T. ) ;
#22380 = ORIENTED_EDGE ( 'NONE', *, *, #4783, .F. ) ;
#22381 = DIRECTION ( 'NONE',  ( -1.000000000000000000, 0.000000000000000000, 0.000000000000000000 ) ) ;
#22382 = VERTEX_POINT ( 'NONE', #27024 ) ;
#22383 = LINE ( 'NONE', #14694, #29885 ) ;
#22384 = DIRECTION ( 'NONE',  ( -1.188208965918165239E-16, -1.880121038077813132E-16, -1.000000000000000000 ) ) ;
#22385 = CARTESIAN_POINT ( 'NONE',  ( -4.902144023942810236, 25.56454579224779167, 47.04930799450042400 ) ) ;
#22386 = VERTEX_POINT ( 'NONE', #27352 ) ;
#22387 = CARTESIAN_POINT ( 'NONE',  ( 78.30297900732490746, -5.614579432636275236, 79.11844573034039740 ) ) ;
#22389 = CARTESIAN_POINT ( 'NONE',  ( -10.01358589504979513, -5.935454207834595763, -13.41617548937563598 ) ) ;
#22388 = CIRCLE ( 'NONE', #10359, 0.1250000000000001110 ) ;
#22390 = CARTESIAN_POINT ( 'NONE',  ( 21.09992658989239089, 29.59143805560861296, 47.04930799450051637 ) ) ;
#22391 = DIRECTION ( 'NONE',  ( 0.000000000000000000, 0.000000000000000000, -1.000000000000000000 ) ) ;
#22392 = CARTESIAN_POINT ( 'NONE',  ( 72.54334031540011551, 8.279996179725053196, 75.27408324235797465 ) ) ;
#22393 = VERTEX_POINT ( 'NONE', #10122 ) ;
#22394 = DIRECTION ( 'NONE',  ( 1.000000000000000000, 0.000000000000000000, 0.000000000000000000 ) ) ;
#22395 = DIRECTION ( 'NONE',  ( -1.101824276508909887E-16, 1.000000000000000000, -0.000000000000000000 ) ) ;
#22396 = AXIS2_PLACEMENT_3D ( 'NONE', #5341, #25987, #8441 ) ;
#22397 = ORIENTED_EDGE ( 'NONE', *, *, #3404, .T. ) ;
#22398 = DIRECTION ( 'NONE',  ( 0.4848096202463430537, 0.8746197071393926326, 1.323854077651070671E-16 ) ) ;
#22399 = DIRECTION ( 'NONE',  ( -0.4848096202463429427, -0.8746197071393925215, 2.352477780477436294E-16 ) ) ;
#22400 = VERTEX_POINT ( 'NONE', #2406 ) ;
#22401 = DIRECTION ( 'NONE',  ( -0.8746197071393926326, 0.4848096202463430537, 8.676864087101709653E-18 ) ) ;
#22402 = ORIENTED_EDGE ( 'NONE', *, *, #32178, .F. ) ;
#22403 = EDGE_CURVE ( 'NONE', #5569, #10175, #7244, .T. ) ;
#22404 = ADVANCED_FACE ( 'NONE', ( #2561 ), #15094, .T. ) ;
#22405 = ORIENTED_EDGE ( 'NONE', *, *, #31832, .T. ) ;
#22406 = AXIS2_PLACEMENT_3D ( 'NONE', #5851, #18140, #21084 ) ;
#22407 = CIRCLE ( 'NONE', #8854, 0.1250000000000001110 ) ;
#22408 = CIRCLE ( 'NONE', #6706, 2.500000000000002220 ) ;
#22409 = DIRECTION ( 'NONE',  ( -1.000000000000000000, 0.000000000000000000, 0.000000000000000000 ) ) ;
#22410 = ADVANCED_FACE ( 'NONE', ( #4699 ), #12503, .T. ) ;
#22411 = ORIENTED_EDGE ( 'NONE', *, *, #31267, .F. ) ;
#22412 = VECTOR ( 'NONE', #228, 1000.000000000000000 ) ;
#22413 = ORIENTED_EDGE ( 'NONE', *, *, #15719, .T. ) ;
#22414 = CARTESIAN_POINT ( 'NONE',  ( 75.29460622866322694, -2.474457146986669187, 13.31118844143965951 ) ) ;
#22415 = CARTESIAN_POINT ( 'NONE',  ( -43.68704682399115313, -4.539174506989449576, 52.13854715134223738 ) ) ;
#22416 = CARTESIAN_POINT ( 'NONE',  ( -40.15225626691278649, 6.735663658092487793, 60.44930799450051495 ) ) ;
#22417 = DIRECTION ( 'NONE',  ( -6.722685822323786766E-17, 1.000000000000000000, -0.000000000000000000 ) ) ;
#22418 = VERTEX_POINT ( 'NONE', #14883 ) ;
#22419 = CARTESIAN_POINT ( 'NONE',  ( -12.50781927836251128, -3.653843372214141461, 102.0960061880259815 ) ) ;
#22420 = VERTEX_POINT ( 'NONE', #20276 ) ;
#22421 = DIRECTION ( 'NONE',  ( -1.101824276508909887E-16, 1.000000000000000000, -0.000000000000000000 ) ) ;
#22422 = DIRECTION ( 'NONE',  ( 0.7141240004913198547, -0.3958453973320100738, -0.5773502691896283956 ) ) ;
#22423 = ORIENTED_EDGE ( 'NONE', *, *, #2641, .T. ) ;
#22424 = DIRECTION ( 'NONE',  ( -1.000000000000000000, 0.000000000000000000, 0.000000000000000000 ) ) ;
#22425 = DIRECTION ( 'NONE',  ( -1.101824276508909887E-16, 1.000000000000000000, -0.000000000000000000 ) ) ;
#22426 = CARTESIAN_POINT ( 'NONE',  ( 52.20929784716416577, -5.935454207834595763, 107.5147914783766510 ) ) ;
#22427 = CARTESIAN_POINT ( 'NONE',  ( -41.08785830660042393, 9.277514380576532105, 39.40788663826320715 ) ) ;
#22428 = CARTESIAN_POINT ( 'NONE',  ( 46.00908685603034343, 26.14624452788249087, 44.91496614357595263 ) ) ;
#22429 = FACE_OUTER_BOUND ( 'NONE', #2572, .T. ) ;
#22430 = DIRECTION ( 'NONE',  ( 0.000000000000000000, -1.000000000000000000, 0.000000000000000000 ) ) ;
#22431 = EDGE_CURVE ( 'NONE', #21772, #10919, #22580, .T. ) ;
#22432 = ORIENTED_EDGE ( 'NONE', *, *, #9028, .F. ) ;
#22433 = DIRECTION ( 'NONE',  ( 0.9577728606650218746, 0.2746369484007246675, 0.08512164205816423468 ) ) ;
#22434 = DIRECTION ( 'NONE',  ( 1.000000000000000000, 0.000000000000000000, 0.000000000000000000 ) ) ;
#22435 = AXIS2_PLACEMENT_3D ( 'NONE', #22708, #27477, #223 ) ;
#22436 = ORIENTED_EDGE ( 'NONE', *, *, #1711, .F. ) ;
#22437 = CIRCLE ( 'NONE', #20347, 2.000000000000001776 ) ;
#22438 = EDGE_CURVE ( 'NONE', #257, #28333, #16130, .T. ) ;
#22439 = CARTESIAN_POINT ( 'NONE',  ( 45.00053793792376666, 28.05920399681022559, 45.68869892245983522 ) ) ;
#22440 = AXIS2_PLACEMENT_3D ( 'NONE', #26314, #11221, #28944 ) ;
#22441 = ORIENTED_EDGE ( 'NONE', *, *, #6366, .T. ) ;
#22442 = VERTEX_POINT ( 'NONE', #27177 ) ;
#22443 = FACE_OUTER_BOUND ( 'NONE', #27526, .T. ) ;
#22444 = EDGE_CURVE ( 'NONE', #31580, #28492, #14066, .T. ) ;
#22445 = EDGE_CURVE ( 'NONE', #25766, #28443, #23474, .T. ) ;
#22446 = CIRCLE ( 'NONE', #10931, 0.1000000000000006301 ) ;
#22447 = ORIENTED_EDGE ( 'NONE', *, *, #7036, .F. ) ;
#22448 = ORIENTED_EDGE ( 'NONE', *, *, #21112, .T. ) ;
#22449 = CARTESIAN_POINT ( 'NONE',  ( 45.41164638504195494, 22.93807716476589675, 46.96173444154113241 ) ) ;
#22450 = EDGE_CURVE ( 'NONE', #460, #7622, #1984, .T. ) ;
#22451 = CARTESIAN_POINT ( 'NONE',  ( -40.30085376570235667, 8.316488220933674569, 54.52001867261917312 ) ) ;
#22452 = AXIS2_PLACEMENT_3D ( 'NONE', #21727, #14202, #6644 ) ;
#22453 = ORIENTED_EDGE ( 'NONE', *, *, #31028, .T. ) ;
#22454 = VECTOR ( 'NONE', #8875, 1000.000000000000227 ) ;
#22455 =( NAMED_UNIT ( * ) PLANE_ANGLE_UNIT ( ) SI_UNIT ( $, .RADIAN. ) );
#22456 = CIRCLE ( 'NONE', #8331, 69.59901951359279337 ) ;
#22457 = DIRECTION ( 'NONE',  ( 0.000000000000000000, 0.000000000000000000, -1.000000000000000000 ) ) ;
#22458 = CARTESIAN_POINT ( 'NONE',  ( 21.09992658989239089, 28.34184655352419213, 47.04930799450051637 ) ) ;
#22459 = CARTESIAN_POINT ( 'NONE',  ( 45.81741271322955100, 29.20122849631042072, 49.02305402274571122 ) ) ;
#22460 = ORIENTED_EDGE ( 'NONE', *, *, #21358, .F. ) ;
#22461 = ORIENTED_EDGE ( 'NONE', *, *, #13434, .F. ) ;
#22462 = DIRECTION ( 'NONE',  ( 0.8746197071393925215, -0.4848096202463429982, -8.676864087101708112E-18 ) ) ;
#22463 = ORIENTED_EDGE ( 'NONE', *, *, #25897, .F. ) ;
#22464 = VECTOR ( 'NONE', #15616, 1000.000000000000000 ) ;
#22465 = CARTESIAN_POINT ( 'NONE',  ( -41.00315188238673159, 10.79608561255925991, 36.12712545380572493 ) ) ;
#22466 = DIRECTION ( 'NONE',  ( 0.000000000000000000, 1.446921688628131436E-16, -1.000000000000000000 ) ) ;
#22467 = DIRECTION ( 'NONE',  ( -0.000000000000000000, -1.000000000000000000, 0.000000000000000000 ) ) ;
#22468 = CARTESIAN_POINT ( 'NONE',  ( 21.09785597605720753, 14.86454579224779948, 47.04930799450052348 ) ) ;
#22469 = FACE_OUTER_BOUND ( 'NONE', #7658, .T. ) ;
#22470 = ADVANCED_FACE ( 'NONE', ( #265 ), #18240, .T. ) ;
#22471 = APPLICATION_PROTOCOL_DEFINITION ( 'draft international standard', 'automotive_design', 1998, #705 ) ;
#22472 = ORIENTED_EDGE ( 'NONE', *, *, #6752, .F. ) ;
#22473 = EDGE_LOOP ( 'NONE', ( #19840, #25035, #362, #18968 ) ) ;
#22474 = DIRECTION ( 'NONE',  ( -1.000000000000000000, 0.000000000000000000, 0.000000000000000000 ) ) ;
#22475 = CARTESIAN_POINT ( 'NONE',  ( 8.474859994195286461, 25.59143805560860940, 47.04930799450051637 ) ) ;
#22476 = EDGE_CURVE ( 'NONE', #19469, #9081, #7771, .T. ) ;
#22477 = CARTESIAN_POINT ( 'NONE',  ( -40.16503835899720087, 7.510440877657823755, 38.80028690913362510 ) ) ;
#22478 = ORIENTED_EDGE ( 'NONE', *, *, #14598, .T. ) ;
#22479 = DIRECTION ( 'NONE',  ( -1.000000000000000000, 0.000000000000000000, -1.224646799147353207E-16 ) ) ;
#22480 = ORIENTED_EDGE ( 'NONE', *, *, #13470, .F. ) ;
#22481 = DIRECTION ( 'NONE',  ( 0.000000000000000000, -1.000000000000000000, 0.000000000000000000 ) ) ;
#22482 = DIRECTION ( 'NONE',  ( -1.000000000000000000, 0.000000000000000000, 0.000000000000000000 ) ) ;
#22483 = AXIS2_PLACEMENT_3D ( 'NONE', #792, #16199, #15560 ) ;
#22484 = EDGE_CURVE ( 'NONE', #19450, #28686, #22949, .T. ) ;
#22485 = PLANE ( 'NONE',  #2361 ) ;
#22486 = EDGE_CURVE ( 'NONE', #24034, #28026, #31514, .T. ) ;
#22487 =( BOUNDED_CURVE ( )  B_SPLINE_CURVE ( 3, ( #10738, #31236, #13836, #6277 ),
 .UNSPECIFIED., .F., .F. ) 
 B_SPLINE_CURVE_WITH_KNOTS ( ( 4, 4 ),
 ( 3.141592653589791784, 4.712388980384687898 ),
 .UNSPECIFIED. ) 
 CURVE ( )  GEOMETRIC_REPRESENTATION_ITEM ( )  RATIONAL_B_SPLINE_CURVE ( ( 1.000000000000000000, 0.8047378541243650485, 0.8047378541243650485, 1.000000000000000000 ) ) 
 REPRESENTATION_ITEM ( '' )  );
#22488 = TOROIDAL_SURFACE ( 'NONE', #32474, 26.49999999999999645, 1.499999999999997780 ) ;
#22489 = ORIENTED_EDGE ( 'NONE', *, *, #8083, .F. ) ;
#22490 = AXIS2_PLACEMENT_3D ( 'NONE', #15582, #5099, #25599 ) ;
#22491 = EDGE_LOOP ( 'NONE', ( #15283, #30243, #9133, #25655 ) ) ;
#22492 = CARTESIAN_POINT ( 'NONE',  ( 21.09785597605720042, 14.86454579224779948, 101.2593585008393404 ) ) ;
#22493 = CARTESIAN_POINT ( 'NONE',  ( 72.51463730528963936, 10.40182650318959112, 72.80069388813021192 ) ) ;
#22494 = CARTESIAN_POINT ( 'NONE',  ( 48.94625023931840957, 25.35784706826093426, 46.10640627770150246 ) ) ;
#22495 = ORIENTED_EDGE ( 'NONE', *, *, #3021, .T. ) ;
#22496 = CARTESIAN_POINT ( 'NONE',  ( -29.27613032885505007, 8.768497436727981764, 75.00977582921336762 ) ) ;
#22497 = FACE_OUTER_BOUND ( 'NONE', #21663, .T. ) ;
#22498 = CARTESIAN_POINT ( 'NONE',  ( 46.27991722120741258, 29.86454579224779948, 45.44588160288975587 ) ) ;
#22499 = APPLICATION_CONTEXT ( 'automotive_design' ) ;
#22500 = CARTESIAN_POINT ( 'NONE',  ( 21.09992658989239089, 26.72145308207318948, 47.04930799450051637 ) ) ;
#22501 = CIRCLE ( 'NONE', #4164, 1.000000000000000888 ) ;
#22502 = AXIS2_PLACEMENT_3D ( 'NONE', #6467, #28474, #23702 ) ;
#22503 = CARTESIAN_POINT ( 'NONE',  ( 21.09785597605719332, 45.06299627138002251, 24.54752547464790524 ) ) ;
#22504 = CARTESIAN_POINT ( 'NONE',  ( 21.09785597605720397, -19.93545420775220123, -37.95069200549950494 ) ) ;
#22505 = DIRECTION ( 'NONE',  ( 0.2756373558169932236, -0.9612616959383205595, 1.479773560108267395E-16 ) ) ;
#22506 = DIRECTION ( 'NONE',  ( 0.000000000000000000, 3.756723415560144304E-15, -1.000000000000000000 ) ) ;
#22507 = DIRECTION ( 'NONE',  ( -0.6298853748009114462, 0.7071067811865472397, 0.3213166889719795694 ) ) ;
#22508 = FACE_OUTER_BOUND ( 'NONE', #20113, .T. ) ;
#22509 = EDGE_CURVE ( 'NONE', #14586, #10311, #2371, .T. ) ;
#22510 =( LENGTH_UNIT ( ) NAMED_UNIT ( * ) SI_UNIT ( .MILLI., .METRE. ) );
#22511 = ORIENTED_EDGE ( 'NONE', *, *, #14170, .T. ) ;
#22512 = ORIENTED_EDGE ( 'NONE', *, *, #10439, .F. ) ;
#22513 = DIRECTION ( 'NONE',  ( -1.101824276508909887E-16, 1.000000000000000000, -0.000000000000000000 ) ) ;
#22514 = CARTESIAN_POINT ( 'NONE',  ( -40.70335362822509495, 9.387769322903325886, 39.54930799450052348 ) ) ;
#22515 = LINE ( 'NONE', #25478, #8806 ) ;
#22516 = CIRCLE ( 'NONE', #1032, 12.62506659569710443 ) ;
#22517 = VECTOR ( 'NONE', #14186, 1000.000000000000000 ) ;
#22518 = FACE_OUTER_BOUND ( 'NONE', #4761, .T. ) ;
#22519 = ORIENTED_EDGE ( 'NONE', *, *, #17705, .T. ) ;
#22520 = CARTESIAN_POINT ( 'NONE',  ( 40.09785597605721108, 13.86454579224779948, 47.04930799450052348 ) ) ;
#22521 = AXIS2_PLACEMENT_3D ( 'NONE', #22775, #9992, #25251 ) ;
#22522 = CARTESIAN_POINT ( 'NONE',  ( 21.09785597605719332, 17.56454579224779877, 47.04930799450051637 ) ) ;
#22523 = CARTESIAN_POINT ( 'NONE',  ( 21.09785597605720042, 12.74140866975414887, 102.9204696617962185 ) ) ;
#22524 = ORIENTED_EDGE ( 'NONE', *, *, #14891, .F. ) ;
#22525 = ORIENTED_EDGE ( 'NONE', *, *, #8803, .T. ) ;
#22526 = DIRECTION ( 'NONE',  ( 0.000000000000000000, -1.000000000000000000, 0.000000000000000000 ) ) ;
#22527 = CARTESIAN_POINT ( 'NONE',  ( 46.00908685603034343, 28.33284706826092503, 44.91496614357594552 ) ) ;
#22528 = CIRCLE ( 'NONE', #19906, 0.1250000000000001110 ) ;
#22529 = B_SPLINE_CURVE_WITH_KNOTS ( 'NONE', 3,
 ( #24542, #26849, #27504, #27167, #9618, #6828, #4687, #16983 ),
 .UNSPECIFIED., .F., .F.,
 ( 4, 2, 2, 4 ),
 ( 0.0002082711175172216199, 0.0005080769251113473285, 0.0008078827327054731184, 0.001407494347893724481 ),
 .UNSPECIFIED. ) ;
#22530 = FACE_OUTER_BOUND ( 'NONE', #17869, .T. ) ;
#22531 = EDGE_CURVE ( 'NONE', #21089, #8039, #29201, .T. ) ;
#22532 = CARTESIAN_POINT ( 'NONE',  ( 21.09992658989238734, 38.56284415653841791, 47.04930799450051637 ) ) ;
#22533 = SPHERICAL_SURFACE ( 'NONE', #28763, 0.1000000000000000056 ) ;
#22534 = CIRCLE ( 'NONE', #11518, 0.5000000000000004441 ) ;
#22535 = TOROIDAL_SURFACE ( 'NONE', #19912, 12.40141737965288726, 0.1250000000000003331 ) ;
#22536 = VERTEX_POINT ( 'NONE', #903 ) ;
#22537 = CARTESIAN_POINT ( 'NONE',  ( 33.50134396954518934, 31.84164230456639544, 47.04930799450051637 ) ) ;
#22538 = AXIS2_PLACEMENT_3D ( 'NONE', #12712, #32238, #4652 ) ;
#22539 = ORIENTED_EDGE ( 'NONE', *, *, #11433, .T. ) ;
#22540 = CARTESIAN_POINT ( 'NONE',  ( 21.09992658989238734, 32.09184655352418503, 47.04930799450051637 ) ) ;
#22541 = CARTESIAN_POINT ( 'NONE',  ( 21.09785597605720397, -15.93545420775219945, 119.5493079945004808 ) ) ;
#22542 = AXIS2_PLACEMENT_3D ( 'NONE', #4544, #2736, #25058 ) ;
#22543 = AXIS2_PLACEMENT_3D ( 'NONE', #30101, #22526, #10390 ) ;
#22544 = ORIENTED_EDGE ( 'NONE', *, *, #21553, .T. ) ;
#22545 = DIRECTION ( 'NONE',  ( 1.000000000000000000, 0.000000000000000000, 0.000000000000000000 ) ) ;
#22546 = EDGE_LOOP ( 'NONE', ( #7648, #24806, #2340, #22511 ) ) ;
#22547 = DIRECTION ( 'NONE',  ( -1.101824276508909887E-16, 1.000000000000000000, -0.000000000000000000 ) ) ;
#22548 = DIRECTION ( 'NONE',  ( 0.8746197071393926326, -0.4848096202463430537, -8.676864087101709653E-18 ) ) ;
#22549 = CARTESIAN_POINT ( 'NONE',  ( 33.88204617658421824, 17.36451738380053555, 47.04930799450051637 ) ) ;
#22550 = ORIENTED_EDGE ( 'NONE', *, *, #31113, .T. ) ;
#22551 = CARTESIAN_POINT ( 'NONE',  ( 71.55936645880184699, 9.702389020015065313, 73.75010705023584023 ) ) ;
#22552 = CARTESIAN_POINT ( 'NONE',  ( -10.01358928193996434, -5.935454061169746609, -13.44187069025445602 ) ) ;
#22553 = VECTOR ( 'NONE', #8394, 1000.000000000000000 ) ;
#22554 = DIRECTION ( 'NONE',  ( -1.000000000000000000, 0.000000000000000000, 0.000000000000000000 ) ) ;
#22555 = DIRECTION ( 'NONE',  ( 0.000000000000000000, 0.000000000000000000, 1.000000000000000000 ) ) ;
#22556 = CARTESIAN_POINT ( 'NONE',  ( 73.79844651144168211, 3.230235421722119860, 78.70801319132137053 ) ) ;
#22557 = ORIENTED_EDGE ( 'NONE', *, *, #26533, .T. ) ;
#22558 = DIRECTION ( 'NONE',  ( -1.000000000000000000, 0.000000000000000000, 0.000000000000000000 ) ) ;
#22559 = CARTESIAN_POINT ( 'NONE',  ( 8.482002859293432451, 27.46664230456639899, 47.04930799450051637 ) ) ;
#22560 = ORIENTED_EDGE ( 'NONE', *, *, #27106, .T. ) ;
#22561 = CARTESIAN_POINT ( 'NONE',  ( 21.09992658989239089, 27.71183152705960850, 47.04930799450051637 ) ) ;
#22562 = ADVANCED_FACE ( 'NONE', ( #15366 ), #20325, .T. ) ;
#22563 = TOROIDAL_SURFACE ( 'NONE', #6332, 83.95485889133257729, 94.44530576803552435 ) ;
#22564 = DIRECTION ( 'NONE',  ( 0.8746197071393926326, -0.4848096202463430537, -8.676864087101709653E-18 ) ) ;
#22565 = EDGE_CURVE ( 'NONE', #16711, #15162, #8299, .T. ) ;
#22566 = ADVANCED_FACE ( 'NONE', ( #23396 ), #25375, .T. ) ;
#22567 = VERTEX_POINT ( 'NONE', #12917 ) ;
#22568 = EDGE_CURVE ( 'NONE', #29739, #163, #4088, .T. ) ;
#22569 = VECTOR ( 'NONE', #14940, 1000.000000000000000 ) ;
#22570 = ORIENTED_EDGE ( 'NONE', *, *, #28461, .T. ) ;
#22571 = EDGE_CURVE ( 'NONE', #1960, #11279, #751, .T. ) ;
#22572 = EDGE_CURVE ( 'NONE', #21015, #414, #10394, .T. ) ;
#22573 = CIRCLE ( 'NONE', #25209, 30.00000000000000711 ) ;
#22574 = AXIS2_PLACEMENT_3D ( 'NONE', #18049, #22813, #27910 ) ;
#22575 = AXIS2_PLACEMENT_3D ( 'NONE', #19114, #16821, #9283 ) ;
#22576 = VERTEX_POINT ( 'NONE', #5365 ) ;
#22577 = AXIS2_PLACEMENT_3D ( 'NONE', #12278, #17516, #12606 ) ;
#22578 = EDGE_CURVE ( 'NONE', #23798, #24691, #22906, .T. ) ;
#22579 = DIRECTION ( 'NONE',  ( 0.8746197071393926326, -0.4848096202463430537, -8.676864087101709653E-18 ) ) ;
#22580 = LINE ( 'NONE', #19625, #11429 ) ;
#22581 = ORIENTED_EDGE ( 'NONE', *, *, #27468, .T. ) ;
#22582 = ORIENTED_EDGE ( 'NONE', *, *, #30472, .F. ) ;
#22583 = DIRECTION ( 'NONE',  ( -1.101824276508909887E-16, 1.000000000000000000, -0.000000000000000000 ) ) ;
#22584 = DIRECTION ( 'NONE',  ( -1.101824276508909887E-16, 1.000000000000000000, -0.000000000000000000 ) ) ;
#22585 = VECTOR ( 'NONE', #964, 999.9999999999998863 ) ;
#22586 = DIRECTION ( 'NONE',  ( -1.224646799147353207E-16, -1.349345573449484691E-32, 1.000000000000000000 ) ) ;
#22587 = DIRECTION ( 'NONE',  ( -1.000000000000000000, 0.000000000000000000, 0.000000000000000000 ) ) ;
#22588 = DIRECTION ( 'NONE',  ( -1.101824276508909887E-16, 1.000000000000000000, -0.000000000000000000 ) ) ;
#22589 = VECTOR ( 'NONE', #5168, 1000.000000000000000 ) ;
#22590 = ADVANCED_FACE ( 'NONE', ( #30635 ), #23226, .F. ) ;
#22591 = VERTEX_POINT ( 'NONE', #23069 ) ;
#22592 = CARTESIAN_POINT ( 'NONE',  ( 21.09785597605719332, 45.06299627138002251, 47.04930799450051637 ) ) ;
#22593 = ORIENTED_EDGE ( 'NONE', *, *, #24603, .F. ) ;
#22594 = CARTESIAN_POINT ( 'NONE',  ( -35.76350089666777876, -4.599861557816947055, 13.89978500458213873 ) ) ;
#22595 = CARTESIAN_POINT ( 'NONE',  ( 79.88559988584306382, -5.819500620027728388, 15.36413957712890088 ) ) ;
#22596 = CIRCLE ( 'NONE', #16287, 2.000000000000000000 ) ;
#22597 = ORIENTED_EDGE ( 'NONE', *, *, #13837, .T. ) ;
#22598 = CARTESIAN_POINT ( 'NONE',  ( 21.09992658989238734, 38.56284415653841791, 47.04930799450051637 ) ) ;
#22599 = CARTESIAN_POINT ( 'NONE',  ( -41.04685960816998147, 9.497330455345890599, 38.54930799450052348 ) ) ;
#22600 = CARTESIAN_POINT ( 'NONE',  ( 48.69396222501143967, 22.86454579224779948, 45.77688862270734660 ) ) ;
#22601 = CARTESIAN_POINT ( 'NONE',  ( 47.09785597605719687, 23.12036939723557083, 47.04930799450080059 ) ) ;
#22602 = CARTESIAN_POINT ( 'NONE',  ( 21.09992658989238734, 31.84184655352418503, 47.04930799450051637 ) ) ;
#22603 = CARTESIAN_POINT ( 'NONE',  ( 45.79384627280941089, 27.07957786121582444, 49.05938063676249072 ) ) ;
#22604 = FACE_OUTER_BOUND ( 'NONE', #3183, .T. ) ;
#22605 = CARTESIAN_POINT ( 'NONE',  ( -40.14651252454546437, 6.746025643617124423, 34.64930799450052490 ) ) ;
#22606 = VERTEX_POINT ( 'NONE', #8148 ) ;
#22607 = CARTESIAN_POINT ( 'NONE',  ( 21.09992658989239089, 25.84164230456639899, 47.04930799450051637 ) ) ;
#22608 = CARTESIAN_POINT ( 'NONE',  ( 48.37020528065356473, 25.16454579224780019, 49.54352675938351069 ) ) ;
#22609 = ORIENTED_EDGE ( 'NONE', *, *, #589, .T. ) ;
#22610 = TOROIDAL_SURFACE ( 'NONE', #22055, 12.61792373059891048, 0.1250000000000026368 ) ;
#22611 = DIRECTION ( 'NONE',  ( 0.2756373558169954441, -0.9612616959383198934, 1.479773560108263451E-16 ) ) ;
#22612 = ORIENTED_EDGE ( 'NONE', *, *, #15012, .F. ) ;
#22613 = ADVANCED_FACE ( 'NONE', ( #588 ), #10619, .F. ) ;
#22614 = ORIENTED_EDGE ( 'NONE', *, *, #671, .T. ) ;
#22615 = CARTESIAN_POINT ( 'NONE',  ( 21.09785597605720753, 13.86454579224779948, 47.04930799450052348 ) ) ;
#22616 = EDGE_CURVE ( 'NONE', #8103, #29193, #15682, .T. ) ;
#22617 = CIRCLE ( 'NONE', #2197, 71.99999999999998579 ) ;
#22618 = VERTEX_POINT ( 'NONE', #23237 ) ;
#22619 = AXIS2_PLACEMENT_3D ( 'NONE', #9613, #9937, #15029 ) ;
#22620 = VECTOR ( 'NONE', #4472, 1000.000000000000000 ) ;
#22621 = ORIENTED_EDGE ( 'NONE', *, *, #1114, .F. ) ;
#22622 = FACE_OUTER_BOUND ( 'NONE', #17127, .T. ) ;
#22623 = AXIS2_PLACEMENT_3D ( 'NONE', #22598, #24908, #2424 ) ;
#22624 = EDGE_CURVE ( 'NONE', #31962, #18298, #31351, .T. ) ;
#22625 = ORIENTED_EDGE ( 'NONE', *, *, #10423, .F. ) ;
#22626 = SURFACE_SIDE_STYLE ('',( #32329 ) ) ;
#22627 = CARTESIAN_POINT ( 'NONE',  ( -39.64148344771002286, 7.657122216028891870, 32.14930799450051779 ) ) ;
#22628 = DIRECTION ( 'NONE',  ( -0.000000000000000000, -0.000000000000000000, -1.000000000000000000 ) ) ;
#22629 = CARTESIAN_POINT ( 'NONE',  ( 48.18662509608405031, 25.09624452788248661, 49.18364984542562013 ) ) ;
#22630 = EDGE_CURVE ( 'NONE', #18307, #22267, #22437, .T. ) ;
#22631 = ORIENTED_EDGE ( 'NONE', *, *, #11130, .T. ) ;
#22632 = EDGE_LOOP ( 'NONE', ( #21255, #31936, #9460, #10220 ) ) ;
#22633 = DIRECTION ( 'NONE',  ( -1.101824276508909887E-16, 1.000000000000000000, -0.000000000000000000 ) ) ;
#22634 = EDGE_CURVE ( 'NONE', #9470, #26626, #9104, .T. ) ;
#22635 = VERTEX_POINT ( 'NONE', #16805 ) ;
#22636 = CARTESIAN_POINT ( 'NONE',  ( -40.62017490690357846, 6.854514378931023444, 34.77675100468818670 ) ) ;
#22637 = CIRCLE ( 'NONE', #11635, 55.85791022362053582 ) ;
#22638 = CARTESIAN_POINT ( 'NONE',  ( 8.474859994195281132, 30.84143805560860585, 47.04930799450051637 ) ) ;
#22639 = AXIS2_PLACEMENT_3D ( 'NONE', #31473, #8981, #24235 ) ;
#22640 = AXIS2_PLACEMENT_3D ( 'NONE', #23698, #24011, #29110 ) ;
#22641 = CARTESIAN_POINT ( 'NONE',  ( -5.602943079677954685, 9.702389020015065313, -4.315940132965163656 ) ) ;
#22642 = DIRECTION ( 'NONE',  ( 0.000000000000000000, 1.000000000000000000, 0.000000000000000000 ) ) ;
#22643 = ITEM_DEFINED_TRANSFORMATION ( 'NONE', 'NONE', #16551,  #8172 ) ;
#22644 = EDGE_LOOP ( 'NONE', ( #5140, #23559, #8849, #7778 ) ) ;
#22645 = ORIENTED_EDGE ( 'NONE', *, *, #22896, .F. ) ;
#22646 = CARTESIAN_POINT ( 'NONE',  ( 21.09992658989239089, 27.22145308207318593, 47.04930799450051637 ) ) ;
#22647 = CARTESIAN_POINT ( 'NONE',  ( 8.474859994195282908, 38.56284415653841791, 47.04930799450051637 ) ) ;
#22648 = DIRECTION ( 'NONE',  ( -1.101824276508909887E-16, 1.000000000000000000, -0.000000000000000000 ) ) ;
#22649 = ORIENTED_EDGE ( 'NONE', *, *, #3070, .T. ) ;
#22650 = CARTESIAN_POINT ( 'NONE',  ( 45.35708200440645044, 28.39118040159425860, 45.92000246470680480 ) ) ;
#22651 = ORIENTED_EDGE ( 'NONE', *, *, #12398, .F. ) ;
#22652 = CYLINDRICAL_SURFACE ( 'NONE', #6781, 43.50000000000000000 ) ;
#22653 = DIRECTION ( 'NONE',  ( 1.177206059073964094E-16, -0.2756373558165849391, 0.9612616959384376880 ) ) ;
#22654 = EDGE_CURVE ( 'NONE', #20495, #9745, #8622, .T. ) ;
#22655 = AXIS2_PLACEMENT_3D ( 'NONE', #29143, #16649, #3703 ) ;
#22656 = CARTESIAN_POINT ( 'NONE',  ( -41.09081837022679906, 10.70862666502100069, 57.17865484131924347 ) ) ;
#22657 = CIRCLE ( 'NONE', #8507, 19.18998195308981636 ) ;
#22658 = PRESENTATION_LAYER_ASSIGNMENT (  '', '', ( #29488 ) ) ;
#22659 = VERTEX_POINT ( 'NONE', #8770 ) ;
#22660 = CIRCLE ( 'NONE', #12177, 0.1000000000000018235 ) ;
#22661 = EDGE_LOOP ( 'NONE', ( #10633, #10908, #29961, #8636 ) ) ;
#22662 = EDGE_CURVE ( 'NONE', #7469, #4474, #10958, .T. ) ;
#22663 = AXIS2_PLACEMENT_3D ( 'NONE', #17135, #12071, #17306 ) ;
#22664 = DIRECTION ( 'NONE',  ( -1.000000000000000000, 0.000000000000000000, 0.000000000000000000 ) ) ;
#22665 = DIRECTION ( 'NONE',  ( -0.000000000000000000, -1.000000000000000000, 0.000000000000000000 ) ) ;
#22666 = CARTESIAN_POINT ( 'NONE',  ( 45.35708200440645044, 25.59118040159426855, 45.92000246470679770 ) ) ;
#22667 = EDGE_CURVE ( 'NONE', #21162, #23266, #9932, .T. ) ;
#22668 = VERTEX_POINT ( 'NONE', #18935 ) ;
#22669 = DIRECTION ( 'NONE',  ( -0.9577728606650218746, -0.2746369484007246675, 0.08512164205816423468 ) ) ;
#22670 = DIRECTION ( 'NONE',  ( -1.000000000000000000, -1.101824276508909887E-16, 0.000000000000000000 ) ) ;
#22671 = EDGE_CURVE ( 'NONE', #19672, #6679, #6746, .T. ) ;
#22672 = LINE ( 'NONE', #30560, #28886 ) ;
#22673 = ADVANCED_FACE ( 'NONE', ( #26657 ), #25095, .T. ) ;
#22674 = CARTESIAN_POINT ( 'NONE',  ( -40.99173213700658636, 9.305078116158229662, 39.54930799450052348 ) ) ;
#22675 = EDGE_CURVE ( 'NONE', #12556, #16034, #16484, .T. ) ;
#22676 = CARTESIAN_POINT ( 'NONE',  ( 21.09785597605719332, -9.935454207752199451, 47.04930799450051637 ) ) ;
#22677 = CARTESIAN_POINT ( 'NONE',  ( -40.41647043964083252, 8.356895951721261540, 59.64930799450051779 ) ) ;
#22678 = CARTESIAN_POINT ( 'NONE',  ( 45.37804019580246973, 22.89977464660286444, 47.76827453631080544 ) ) ;
#22679 = CARTESIAN_POINT ( 'NONE',  ( -36.59542768321662720, 12.56771722797891400, 38.09144330556765112 ) ) ;
#22680 = AXIS2_PLACEMENT_3D ( 'NONE', #18702, #18070, #28100 ) ;
#22681 = B_SPLINE_SURFACE_WITH_KNOTS ( 'NONE', 3, 3, ( 
 ( #7698, #12467, #5235, #5072, #9834, #22449 ),
 ( #29862, #19667, #2769, #29697, #7377, #32484 ),
 ( #30187, #17369, #145, #10001, #19997, #17694 ),
 ( #7204, #7861, #17199, #7544, #5400, #27218 ),
 ( #10163, #4745, #15246, #30025, #27556, #304 ),
 ( #17538, #25257, #15083, #12797, #22781, #10324 ) ),
 .UNSPECIFIED., .F., .F., .F.,
 ( 4, 2, 4 ),
 ( 4, 2, 4 ),
 ( 0.000000000000000000, 0.5000000000000000000, 1.000000000000000000 ),
 ( 0.000000000000000000, 0.5000000000000000000, 1.000000000000000000 ),
 .UNSPECIFIED. ) ;
#22682 = CARTESIAN_POINT ( 'NONE',  ( -41.02113223168485234, 7.230835263863472306, 39.44930799450052206 ) ) ;
#22683 = TOROIDAL_SURFACE ( 'NONE', #14820, 55.72393233686778302, 0.09999999999999760469 ) ;
#22684 = DIRECTION ( 'NONE',  ( 8.659560562354932858E-17, 0.7071067811865474617, -0.7071067811865474617 ) ) ;
#22685 = VERTEX_POINT ( 'NONE', #4174 ) ;
#22686 = EDGE_LOOP ( 'NONE', ( #15770, #28836, #25978, #17930 ) ) ;
#22687 = CARTESIAN_POINT ( 'NONE',  ( 47.17209261226641104, 29.58954579224849368, 44.97563639035409011 ) ) ;
#22688 = DIRECTION ( 'NONE',  ( -1.000000000000000000, -1.101824276508909764E-16, 0.000000000000000000 ) ) ;
#22689 = DIRECTION ( 'NONE',  ( -1.000000000000000000, 0.000000000000000000, 0.000000000000000000 ) ) ;
#22690 = CARTESIAN_POINT ( 'NONE',  ( 71.48501281440437083, -5.983766253076979069, 79.12126923977230319 ) ) ;
#22691 = ORIENTED_EDGE ( 'NONE', *, *, #28945, .T. ) ;
#22692 = AXIS2_PLACEMENT_3D ( 'NONE', #19285, #26850, #16831 ) ;
#22693 =( BOUNDED_CURVE ( )  B_SPLINE_CURVE ( 2, ( #27598, #2489, #20045, #12516, #20360, #22177, #5114, #20209, #4791 ),
 .UNSPECIFIED., .F., .F. ) 
 B_SPLINE_CURVE_WITH_KNOTS ( ( 3, 2, 2, 2, 3 ),
 ( 0.3928571416958702711, 0.4047619047619047672, 0.4285714285714286031, 0.4523809523809523281, 0.4642857131244416125 ),
 .UNSPECIFIED. ) 
 CURVE ( )  GEOMETRIC_REPRESENTATION_ITEM ( )  RATIONAL_B_SPLINE_CURVE ( ( 0.9330127018922200755, 0.9330126953578163906, 1.000000000000000000, 0.8660254037844387076, 1.000000000000000000, 0.8660254037844387076, 1.000000000000000000, 0.9330127084266226500, 0.9330127018922199644 ) ) 
 REPRESENTATION_ITEM ( '' )  );
#22694 = DIRECTION ( 'NONE',  ( 1.431146867680865853E-17, 2.558717127065790464E-17, 1.000000000000000000 ) ) ;
#22695 = DIRECTION ( 'NONE',  ( 0.1949050434465250392, -0.6797146636928682595, -0.7071067811865470176 ) ) ;
#22696 = CARTESIAN_POINT ( 'NONE',  ( -42.03703168893574116, 3.954238390689462257, 45.74930799450051211 ) ) ;
#22697 = ORIENTED_EDGE ( 'NONE', *, *, #12275, .F. ) ;
#22698 = ORIENTED_EDGE ( 'NONE', *, *, #27759, .F. ) ;
#22699 = DIRECTION ( 'NONE',  ( -2.779292025043186357E-18, 1.288349127009862057E-17, -1.000000000000000000 ) ) ;
#22700 = CARTESIAN_POINT ( 'NONE',  ( 45.35708200440645044, 25.59118040159426855, 45.92000246470679770 ) ) ;
#22701 = LINE ( 'NONE', #17279, #12029 ) ;
#22702 = CYLINDRICAL_SURFACE ( 'NONE', #16956, 12.36707279061065279 ) ;
#22703 = CARTESIAN_POINT ( 'NONE',  ( 21.09992658989239089, 24.34164230456639544, 47.04930799450051637 ) ) ;
#22704 = ORIENTED_EDGE ( 'NONE', *, *, #15227, .T. ) ;
#22705 = CIRCLE ( 'NONE', #26899, 2.500000000000002220 ) ;
#22706 = VECTOR ( 'NONE', #7009, 1000.000000000000000 ) ;
#22707 = ADVANCED_FACE ( 'NONE', ( #31755 ), #5702, .T. ) ;
#22708 = CARTESIAN_POINT ( 'NONE',  ( 21.09992658989238734, 38.56284415653841791, 47.04930799450051637 ) ) ;
#22709 = EDGE_CURVE ( 'NONE', #16387, #24759, #24547, .T. ) ;
#22710 = VERTEX_POINT ( 'NONE', #3690 ) ;
#22711 = AXIS2_PLACEMENT_3D ( 'NONE', #9943, #25038, #2549 ) ;
#22712 = AXIS2_PLACEMENT_3D ( 'NONE', #12284, #12122, #24254 ) ;
#22713 = DIRECTION ( 'NONE',  ( -1.101824276508909887E-16, 1.000000000000000000, -0.000000000000000000 ) ) ;
#22714 = DIRECTION ( 'NONE',  ( -0.9612616959383221138, -0.2756373558169876170, 0.000000000000000000 ) ) ;
#22715 = EDGE_CURVE ( 'NONE', #22032, #29832, #28237, .T. ) ;
#22716 = EDGE_LOOP ( 'NONE', ( #6809, #11913 ) ) ;
#22717 = LINE ( 'NONE', #10258, #5006 ) ;
#22718 = ORIENTED_EDGE ( 'NONE', *, *, #11980, .F. ) ;
#22719 = CARTESIAN_POINT ( 'NONE',  ( 21.09785597605720753, 13.86454579224779948, 47.04930799450052348 ) ) ;
#22720 = DIRECTION ( 'NONE',  ( -1.000000000000000000, -1.101824276508909887E-16, 0.000000000000000000 ) ) ;
#22721 = CARTESIAN_POINT ( 'NONE',  ( -3.644339245467521859, 10.95889540305196341, 98.61699126615421562 ) ) ;
#22722 = CARTESIAN_POINT ( 'NONE',  ( 8.474859994195286461, 24.34184655352419213, 47.04930799450051637 ) ) ;
#22723 = ORIENTED_EDGE ( 'NONE', *, *, #29500, .F. ) ;
#22724 = CARTESIAN_POINT ( 'NONE',  ( 79.18332612743283505, -5.935454207752198563, 77.87546120947918382 ) ) ;
#22725 = DIRECTION ( 'NONE',  ( -1.101824276508909887E-16, 1.000000000000000000, -0.000000000000000000 ) ) ;
#22726 = CARTESIAN_POINT ( 'NONE',  ( 21.09992658989239089, 28.59164230456639544, 47.04930799450051637 ) ) ;
#22727 = CARTESIAN_POINT ( 'NONE',  ( -35.64882101543633297, 9.925589859889722533, 42.04930799450051637 ) ) ;
#22728 = AXIS2_PLACEMENT_3D ( 'NONE', #6173, #8957, #31610 ) ;
#22729 = CARTESIAN_POINT ( 'NONE',  ( 72.64112472104469020, 7.651854857428991075, 75.81648953516938150 ) ) ;
#22730 = ORIENTED_EDGE ( 'NONE', *, *, #26901, .F. ) ;
#22731 = CARTESIAN_POINT ( 'NONE',  ( 21.09992658989239089, 24.34184655352419213, 47.04930799450051637 ) ) ;
#22732 = DIRECTION ( 'NONE',  ( -0.9097384655268496711, -0.4151817967359032746, -2.088192543647023221E-17 ) ) ;
#22733 = EDGE_LOOP ( 'NONE', ( #14622, #12449, #8057, #16572 ) ) ;
#22734 = CARTESIAN_POINT ( 'NONE',  ( -10.37754766804345508, -5.881344816830196720, -12.09508678449311070 ) ) ;
#22735 = CYLINDRICAL_SURFACE ( 'NONE', #11500, 4.200000000000000178 ) ;
#22736 = DIRECTION ( 'NONE',  ( 0.000000000000000000, 0.000000000000000000, -1.000000000000000000 ) ) ;
#22737 = VECTOR ( 'NONE', #18596, 1000.000000000000114 ) ;
#22738 = ORIENTED_EDGE ( 'NONE', *, *, #11824, .T. ) ;
#22739 = AXIS2_PLACEMENT_3D ( 'NONE', #14674, #17612, #15158 ) ;
#22740 = LINE ( 'NONE', #10281, #16710 ) ;
#22741 = ORIENTED_EDGE ( 'NONE', *, *, #18967, .F. ) ;
#22742 = ORIENTED_EDGE ( 'NONE', *, *, #26524, .F. ) ;
#22743 = CIRCLE ( 'NONE', #5546, 0.1249999999999966416 ) ;
#22744 = DIRECTION ( 'NONE',  ( -1.000000000000000000, 0.000000000000000000, 0.000000000000000000 ) ) ;
#22745 = DIRECTION ( 'NONE',  ( 0.000000000000000000, 1.000000000000000000, 0.000000000000000000 ) ) ;
#22746 = EDGE_CURVE ( 'NONE', #12393, #17230, #956, .T. ) ;
#22747 = ORIENTED_EDGE ( 'NONE', *, *, #25718, .F. ) ;
#22748 = ORIENTED_EDGE ( 'NONE', *, *, #23430, .T. ) ;
#22749 = EDGE_CURVE ( 'NONE', #9808, #27983, #19290, .T. ) ;
#22750 = LINE ( 'NONE', #7167, #6794 ) ;
#22751 = EDGE_CURVE ( 'NONE', #13336, #8460, #25604, .T. ) ;
#22752 = DIRECTION ( 'NONE',  ( -0.000000000000000000, -1.000000000000000000, -0.000000000000000000 ) ) ;
#22753 = CARTESIAN_POINT ( 'NONE',  ( -30.40347463700609865, 7.917901822120666289, 75.58887676006128231 ) ) ;
#22754 = CARTESIAN_POINT ( 'NONE',  ( -5.402144023942789808, 13.86454579224779948, 47.04930799450052348 ) ) ;
#22755 = VERTEX_POINT ( 'NONE', #11397 ) ;
#22756 = CARTESIAN_POINT ( 'NONE',  ( -40.90015969217747482, 8.955334253785164123, 56.14611646155296398 ) ) ;
#22757 = VERTEX_POINT ( 'NONE', #24517 ) ;
#22758 = CARTESIAN_POINT ( 'NONE',  ( -30.33894848875469918, 10.49891163461608379, 21.45876492183288420 ) ) ;
#22759 = CARTESIAN_POINT ( 'NONE',  ( -43.69495677161796010, 1.169528900831203311, 60.44930799450051495 ) ) ;
#22760 = ORIENTED_EDGE ( 'NONE', *, *, #12061, .F. ) ;
#22761 = FACE_OUTER_BOUND ( 'NONE', #6553, .T. ) ;
#22762 = CYLINDRICAL_SURFACE ( 'NONE', #1585, 19.50000000000000000 ) ;
#22763 = DIRECTION ( 'NONE',  ( 0.000000000000000000, 1.000000000000000000, 0.000000000000000000 ) ) ;
#22764 = DIRECTION ( 'NONE',  ( -0.4848096202463424986, -0.8746197071393928546, 2.220446049250312834E-16 ) ) ;
#22765 = CARTESIAN_POINT ( 'NONE',  ( 44.70507715278255745, 27.66291119454915304, 46.92503878583764987 ) ) ;
#22766 = CARTESIAN_POINT ( 'NONE',  ( -40.09616233467386337, 6.848043556934458209, 34.82480928884837112 ) ) ;
#22767 = CARTESIAN_POINT ( 'NONE',  ( 21.09992658989238734, 38.56284415653841791, 47.04930799450051637 ) ) ;
#22768 = ORIENTED_EDGE ( 'NONE', *, *, #20266, .T. ) ;
#22769 = FACE_OUTER_BOUND ( 'NONE', #17497, .T. ) ;
#22770 = ORIENTED_EDGE ( 'NONE', *, *, #16734, .F. ) ;
#22771 = FACE_OUTER_BOUND ( 'NONE', #25130, .T. ) ;
#22772 = ORIENTED_EDGE ( 'NONE', *, *, #26861, .T. ) ;
#22773 = CIRCLE ( 'NONE', #19597, 2.499999999999998668 ) ;
#22774 = EDGE_LOOP ( 'NONE', ( #18396, #23791, #26166, #19144 ) ) ;
#22775 = CARTESIAN_POINT ( 'NONE',  ( -39.64148344771002286, 7.657122216028890982, 32.14930799450051779 ) ) ;
#22776 = AXIS2_PLACEMENT_3D ( 'NONE', #16289, #13840, #9393 ) ;
#22777 = AXIS2_PLACEMENT_3D ( 'NONE', #5102, #24963, #17079 ) ;
#22778 = AXIS2_PLACEMENT_3D ( 'NONE', #19050, #26941, #26456 ) ;
#22779 = ORIENTED_EDGE ( 'NONE', *, *, #16604, .F. ) ;
#22780 = EDGE_LOOP ( 'NONE', ( #2807, #4212, #13152, #13763 ) ) ;
#22781 = CARTESIAN_POINT ( 'NONE',  ( 45.50623141997586174, 22.89977464660286444, 48.01957109218837871 ) ) ;
#22782 = VERTEX_POINT ( 'NONE', #12995 ) ;
#22783 = ADVANCED_FACE ( 'NONE', ( #5283 ), #30022, .F. ) ;
#22784 = ADVANCED_FACE ( 'NONE', ( #22828 ), #25619, .T. ) ;
#22785 = AXIS2_PLACEMENT_3D ( 'NONE', #30072, #4790, #22670 ) ;
#22786 = DIRECTION ( 'NONE',  ( 0.000000000000000000, 0.000000000000000000, 1.000000000000000000 ) ) ;
#22787 = EDGE_CURVE ( 'NONE', #16102, #21972, #16683, .T. ) ;
#22788 = CARTESIAN_POINT ( 'NONE',  ( -17.40214402394279247, 13.86454579224779948, 47.04930799450052348 ) ) ;
#22789 = CARTESIAN_POINT ( 'NONE',  ( 47.22751897799751220, 26.54253733014356342, 44.55267275764142454 ) ) ;
#22790 = CIRCLE ( 'NONE', #12864, 56.65825807113184709 ) ;
#22791 = EDGE_CURVE ( 'NONE', #13157, #1894, #16153, .T. ) ;
#22792 = CARTESIAN_POINT ( 'NONE',  ( 44.70507715278255745, 25.56291119454915517, 46.92503878583764987 ) ) ;
#22793 = ORIENTED_EDGE ( 'NONE', *, *, #25570, .T. ) ;
#22794 = ADVANCED_FACE ( 'NONE', ( #16964 ), #31378, .F. ) ;
#22795 = VERTEX_POINT ( 'NONE', #26989 ) ;
#22797 = CARTESIAN_POINT ( 'NONE',  ( -43.95628906790246759, -0.1269931775117038586, 32.14930799450051779 ) ) ;
#22796 = CIRCLE ( 'NONE', #260, 58.67217910650386870 ) ;
#22798 = CIRCLE ( 'NONE', #8658, 56.65825807113184709 ) ;
#22799 = EDGE_LOOP ( 'NONE', ( #12725, #31072, #7422, #15391 ) ) ;
#22800 = CARTESIAN_POINT ( 'NONE',  ( 21.09785597605720753, 13.86454579224779948, 47.04930799450052348 ) ) ;
#22801 = AXIS2_PLACEMENT_3D ( 'NONE', #21478, #19506, #14593 ) ;
#22802 = CARTESIAN_POINT ( 'NONE',  ( 49.86372208582861276, 7.652955895019247556, 98.59261258995066157 ) ) ;
#22803 = DIRECTION ( 'NONE',  ( -1.000000000000000000, 0.000000000000000000, 0.000000000000000000 ) ) ;
#22804 = CARTESIAN_POINT ( 'NONE',  ( 47.33512057650604277, 22.89977464660286444, 45.20042056806582309 ) ) ;
#22805 = DIRECTION ( 'NONE',  ( 0.8746197071393926326, -0.4848096202463430537, -8.676864087101709653E-18 ) ) ;
#22806 = ORIENTED_EDGE ( 'NONE', *, *, #26533, .F. ) ;
#22807 = EDGE_LOOP ( 'NONE', ( #20071, #27217, #17174, #10499 ) ) ;
#22808 = CARTESIAN_POINT ( 'NONE',  ( -42.38351229602917414, 14.72295342448899191, 58.95959122802360497 ) ) ;
#22809 = CARTESIAN_POINT ( 'NONE',  ( 45.52675994804781112, 28.93420399681022559, 49.47108226228596806 ) ) ;
#22810 = CARTESIAN_POINT ( 'NONE',  ( -9.728297238921260970, -5.935454207752201228, 107.6337305256964640 ) ) ;
#22811 = CARTESIAN_POINT ( 'NONE',  ( 48.83862994770794330, 29.44118040159425931, 48.17861352429476796 ) ) ;
#22812 = ORIENTED_EDGE ( 'NONE', *, *, #21553, .F. ) ;
#22813 = DIRECTION ( 'NONE',  ( -1.101824276508909887E-16, 1.000000000000000000, -0.000000000000000000 ) ) ;
#22814 = CARTESIAN_POINT ( 'NONE',  ( -40.51045226066063520, 7.589116544599141534, 53.87859731638185679 ) ) ;
#22815 = LINE ( 'NONE', #10521, #9170 ) ;
#22816 = AXIS2_PLACEMENT_3D ( 'NONE', #2927, #12959, #10494 ) ;
#22817 = AXIS2_PLACEMENT_3D ( 'NONE', #4061, #9154, #13770 ) ;
#22818 = EDGE_CURVE ( 'NONE', #18076, #22755, #10924, .T. ) ;
#22819 = ADVANCED_FACE ( 'NONE', ( #20043 ), #30071, .T. ) ;
#22820 = AXIS2_PLACEMENT_3D ( 'NONE', #8260, #1023, #5633 ) ;
#22821 = ORIENTED_EDGE ( 'NONE', *, *, #24154, .T. ) ;
#22822 = ORIENTED_EDGE ( 'NONE', *, *, #16222, .T. ) ;
#22823 = DIRECTION ( 'NONE',  ( 0.8746197071393926326, -0.4848096202463430537, -8.676864087101709653E-18 ) ) ;
#22824 = DIRECTION ( 'NONE',  ( -0.000000000000000000, -1.000000000000000000, 0.000000000000000000 ) ) ;
#22825 = CYLINDRICAL_SURFACE ( 'NONE', #21473, 2.500000000000002220 ) ;
#22826 = AXIS2_PLACEMENT_3D ( 'NONE', #3607, #13631, #21480 ) ;
#22827 = ORIENTED_EDGE ( 'NONE', *, *, #26223, .T. ) ;
#22828 = FACE_OUTER_BOUND ( 'NONE', #27360, .T. ) ;
#22829 = CARTESIAN_POINT ( 'NONE',  ( -40.67837904183829068, 9.488261090400163411, 39.44504779057211863 ) ) ;
#22830 = CARTESIAN_POINT ( 'NONE',  ( -0.4021440239427888086, 13.86454579224779948, 47.04930799450052348 ) ) ;
#22831 = EDGE_CURVE ( 'NONE', #15549, #24463, #7909, .T. ) ;
#22832 = LINE ( 'NONE', #30233, #1953 ) ;
#22833 = PLANE ( 'NONE',  #10203 ) ;
#22834 = CARTESIAN_POINT ( 'NONE',  ( 21.09785597605719332, 11.92558985988973497, -9.608950076631337822 ) ) ;
#22835 = CARTESIAN_POINT ( 'NONE',  ( -40.51045226066063520, 7.589116544599135317, 60.22001867261916175 ) ) ;
#22836 = CARTESIAN_POINT ( 'NONE',  ( -43.37834615508418068, 1.121909970995876638, 34.64930799450052490 ) ) ;
#22837 = DIRECTION ( 'NONE',  ( -1.000000000000000000, 0.000000000000000000, 0.000000000000000000 ) ) ;
#22838 = FACE_OUTER_BOUND ( 'NONE', #2350, .T. ) ;
#22839 = CARTESIAN_POINT ( 'NONE',  ( 48.46535932150934656, 28.98954579807170617, 49.73005965046827015 ) ) ;
#22840 = ORIENTED_EDGE ( 'NONE', *, *, #30110, .T. ) ;
#22841 = ORIENTED_EDGE ( 'NONE', *, *, #19376, .T. ) ;
#22842 = DIRECTION ( 'NONE',  ( -1.101824276508909887E-16, 1.000000000000000000, -0.000000000000000000 ) ) ;
#22843 = AXIS2_PLACEMENT_3D ( 'NONE', #30090, #27775, #32379 ) ;
#22844 = AXIS2_PLACEMENT_3D ( 'NONE', #22549, #2857, #12893 ) ;
#22845 = FACE_OUTER_BOUND ( 'NONE', #6957, .T. ) ;
#22846 = CARTESIAN_POINT ( 'NONE',  ( -32.38499150730411458, -1.224855502300924437, 13.47596506989118836 ) ) ;
#22847 = CARTESIAN_POINT ( 'NONE',  ( 21.09992658989239089, 25.09164230456639899, 47.04930799450051637 ) ) ;
#22848 = VERTEX_POINT ( 'NONE', #25461 ) ;
#22849 = LINE ( 'NONE', #5305, #17688 ) ;
#22850 = DIRECTION ( 'NONE',  ( 0.000000000000000000, 1.000000000000000000, -0.000000000000000000 ) ) ;
#22851 = DIRECTION ( 'NONE',  ( 0.000000000000000000, 1.000000000000000000, -0.000000000000000000 ) ) ;
#22852 = ADVANCED_FACE ( 'NONE', ( #17581 ), #18256, .T. ) ;
#22853 = ORIENTED_EDGE ( 'NONE', *, *, #3070, .F. ) ;
#22854 = ORIENTED_EDGE ( 'NONE', *, *, #531, .F. ) ;
#22855 = CARTESIAN_POINT ( 'NONE',  ( 21.09992658989239089, 25.09164230456639899, 47.04930799450051637 ) ) ;
#22856 = CARTESIAN_POINT ( 'NONE',  ( 48.40186567930498285, 28.21618040159426499, 45.03923535223908203 ) ) ;
#22857 = CARTESIAN_POINT ( 'NONE',  ( 44.70507715278255745, 29.06291119454914451, 46.92503878583764987 ) ) ;
#22858 = ADVANCED_FACE ( 'NONE', ( #20358 ), #13545, .T. ) ;
#22859 = CONICAL_SURFACE ( 'NONE', #22332, 67.38776620500242132, 0.5061454830783623793 ) ;
#22860 = FACE_OUTER_BOUND ( 'NONE', #14437, .T. ) ;
#22861 = DIRECTION ( 'NONE',  ( -1.000000000000000000, 0.000000000000000000, 0.000000000000000000 ) ) ;
#22862 = EDGE_CURVE ( 'NONE', #21437, #19261, #30229, .T. ) ;
#22863 = EDGE_CURVE ( 'NONE', #24037, #24849, #30861, .T. ) ;
#22864 = ORIENTED_EDGE ( 'NONE', *, *, #22818, .T. ) ;
#22865 = EDGE_CURVE ( 'NONE', #19678, #6679, #8823, .T. ) ;
#22866 = CARTESIAN_POINT ( 'NONE',  ( -42.47434154250544225, 4.196643200812637531, 58.34930799450052064 ) ) ;
#22867 = CIRCLE ( 'NONE', #26003, 0.1250000000000001110 ) ;
#22868 = VERTEX_POINT ( 'NONE', #6083 ) ;
#22869 = CARTESIAN_POINT ( 'NONE',  ( -36.76418579970419387, 10.14130568307076352, 57.95249952744806166 ) ) ;
#22870 = DIRECTION ( 'NONE',  ( 0.000000000000000000, 0.000000000000000000, -1.000000000000000000 ) ) ;
#22871 = EDGE_CURVE ( 'NONE', #1121, #5504, #30334, .T. ) ;
#22872 = AXIS2_PLACEMENT_3D ( 'NONE', #4502, #9432, #16962 ) ;
#22873 = VERTEX_POINT ( 'NONE', #25776 ) ;
#22874 = CARTESIAN_POINT ( 'NONE',  ( 45.39969523643555505, 22.86454579224779948, 45.99212200068701861 ) ) ;
#22875 = ORIENTED_EDGE ( 'NONE', *, *, #29160, .F. ) ;
#22876 = CARTESIAN_POINT ( 'NONE',  ( 80.64537389521012756, -5.931148802125833619, 78.13246447790419325 ) ) ;
#22877 = CARTESIAN_POINT ( 'NONE',  ( -40.60333149162104860, 7.557375771971046596, 54.64930799450051779 ) ) ;
#22878 =( BOUNDED_CURVE ( )  B_SPLINE_CURVE ( 3, ( #11771, #11288, #4540, #18810 ),
 .UNSPECIFIED., .F., .F. ) 
 B_SPLINE_CURVE_WITH_KNOTS ( ( 4, 4 ),
 ( 2.008243333561409827, 2.704294664099573975 ),
 .UNSPECIFIED. ) 
 CURVE ( )  GEOMETRIC_REPRESENTATION_ITEM ( )  RATIONAL_B_SPLINE_CURVE ( ( 1.000000000000000000, 0.9600319177481757560, 0.9600319177481757560, 1.000000000000000000 ) ) 
 REPRESENTATION_ITEM ( '' )  );
#22879 = DIRECTION ( 'NONE',  ( -1.000000000000000000, -1.101824276508909764E-16, 0.000000000000000000 ) ) ;
#22880 = CARTESIAN_POINT ( 'NONE',  ( 21.09785597605719332, -13.49020584019834601, 47.04930799450051637 ) ) ;
#22881 = ORIENTED_EDGE ( 'NONE', *, *, #12647, .F. ) ;
#22882 = CARTESIAN_POINT ( 'NONE',  ( 47.09785597605719687, 30.56454579224779522, 47.04930799450078638 ) ) ;
#22883 = CARTESIAN_POINT ( 'NONE',  ( 21.09785597605720753, 14.16454579224779842, 47.04930799450052348 ) ) ;
#22884 = CARTESIAN_POINT ( 'NONE',  ( -41.02113223168485234, 7.230835263863471418, 34.54930799450052348 ) ) ;
#22885 = DIRECTION ( 'NONE',  ( -0.000000000000000000, -1.000000000000000000, 0.000000000000000000 ) ) ;
#22886 = CARTESIAN_POINT ( 'NONE',  ( 49.98072202819531640, 26.24488759933319670, 47.19902993264913960 ) ) ;
#22887 = ORIENTED_EDGE ( 'NONE', *, *, #25090, .T. ) ;
#22888 = DIRECTION ( 'NONE',  ( -0.000000000000000000, 1.000000000000000000, -0.000000000000000000 ) ) ;
#22889 = CARTESIAN_POINT ( 'NONE',  ( 33.71785032049134401, 27.96664230456639899, 47.04930799450051637 ) ) ;
#22890 = EDGE_CURVE ( 'NONE', #24509, #490, #10408, .T. ) ;
#22891 = ORIENTED_EDGE ( 'NONE', *, *, #6257, .F. ) ;
#22892 = CARTESIAN_POINT ( 'NONE',  ( -42.24141723705587737, 13.63285518870473290, 59.54930799450050927 ) ) ;
#22893 = CARTESIAN_POINT ( 'NONE',  ( -40.52669582637187773, 7.652910973922034010, 60.15421819779514578 ) ) ;
#22894 = VECTOR ( 'NONE', #3752, 1000.000000000000000 ) ;
#22895 = CARTESIAN_POINT ( 'NONE',  ( -38.57628410747783221, -0.7885452029232787874, 13.38511290719907798 ) ) ;
#22896 = EDGE_CURVE ( 'NONE', #6923, #7408, #26369, .T. ) ;
#22897 = CARTESIAN_POINT ( 'NONE',  ( -45.06166779280743384, -5.721341737285086992, 53.14897153969102561 ) ) ;
#22898 = EDGE_LOOP ( 'NONE', ( #1250, #28924, #1249, #14854 ) ) ;
#22899 = FACE_OUTER_BOUND ( 'NONE', #28225, .T. ) ;
#22900 = ORIENTED_EDGE ( 'NONE', *, *, #21822, .T. ) ;
#22901 = EDGE_CURVE ( 'NONE', #10687, #30925, #8326, .T. ) ;
#22902 = AXIS2_PLACEMENT_3D ( 'NONE', #22703, #32337, #4923 ) ;
#22903 = EDGE_LOOP ( 'NONE', ( #16192, #28520, #28425, #6771 ) ) ;
#22904 = ADVANCED_FACE ( 'NONE', ( #28248 ), #5764, .F. ) ;
#22905 = CARTESIAN_POINT ( 'NONE',  ( 8.732853799281734553, 38.56284415653841791, 47.04930799450051637 ) ) ;
#22906 = LINE ( 'NONE', #423, #13024 ) ;
#22907 = CIRCLE ( 'NONE', #19742, 31.00000000000000000 ) ;
#22908 = ORIENTED_EDGE ( 'NONE', *, *, #19559, .T. ) ;
#22909 = EDGE_LOOP ( 'NONE', ( #17313, #27508, #24544 ) ) ;
#22910 = CARTESIAN_POINT ( 'NONE',  ( -44.11922148153472278, -5.395861642922686663, 52.67658529385213484 ) ) ;
#22911 = FACE_OUTER_BOUND ( 'NONE', #27208, .T. ) ;
#22912 = DIRECTION ( 'NONE',  ( -1.000000000000000000, 0.000000000000000000, 0.000000000000000000 ) ) ;
#22913 = ORIENTED_EDGE ( 'NONE', *, *, #9794, .T. ) ;
#22914 = CARTESIAN_POINT ( 'NONE',  ( 47.91579473090698116, 29.86454579224779948, 48.65273438611181689 ) ) ;
#22915 = DIRECTION ( 'NONE',  ( -1.000000000000000000, 0.000000000000000000, 0.000000000000000000 ) ) ;
#22916 = DIRECTION ( 'NONE',  ( -0.8746197071393926326, 0.4848096202463430537, 8.676864087101709653E-18 ) ) ;
#22917 = DIRECTION ( 'NONE',  ( -1.101824276508909887E-16, 1.000000000000000000, -0.000000000000000000 ) ) ;
#22918 = VERTEX_POINT ( 'NONE', #8382 ) ;
#22919 = CARTESIAN_POINT ( 'NONE',  ( 47.59771343202220351, 22.98879437201065912, 45.66843904406525922 ) ) ;
#22920 = LINE ( 'NONE', #8163, #4741 ) ;
#22921 = DIRECTION ( 'NONE',  ( 1.188208965918165239E-16, 1.880121038077813132E-16, 1.000000000000000000 ) ) ;
#22922 = DIRECTION ( 'NONE',  ( -1.101824276508909887E-16, 1.000000000000000000, -0.000000000000000000 ) ) ;
#22923 = CARTESIAN_POINT ( 'NONE',  ( 48.94625023931840246, 29.47124452788248306, 46.10640627770150246 ) ) ;
#22924 = CARTESIAN_POINT ( 'NONE',  ( 21.09992658989239089, 25.34164230456639899, 47.04930799450051637 ) ) ;
#22925 = DIRECTION ( 'NONE',  ( 0.000000000000000000, -0.000000000000000000, -1.000000000000000000 ) ) ;
#22926 = ORIENTED_EDGE ( 'NONE', *, *, #4000, .T. ) ;
#22927 = DIRECTION ( 'NONE',  ( 0.000000000000000000, 0.000000000000000000, -1.000000000000000000 ) ) ;
#22928 = VERTEX_POINT ( 'NONE', #18382 ) ;
#22929 = CARTESIAN_POINT ( 'NONE',  ( 21.09785597605720397, -16.93042895458276575, 131.5543332476699732 ) ) ;
#22930 = ORIENTED_EDGE ( 'NONE', *, *, #13278, .F. ) ;
#22931 = ORIENTED_EDGE ( 'NONE', *, *, #29533, .F. ) ;
#22932 = DIRECTION ( 'NONE',  ( -1.101824276508909887E-16, 1.000000000000000000, -0.000000000000000000 ) ) ;
#22933 = CIRCLE ( 'NONE', #16621, 2.000000000000001776 ) ;
#22934 = EDGE_CURVE ( 'NONE', #30065, #3912, #21916, .T. ) ;
#22935 = ORIENTED_EDGE ( 'NONE', *, *, #24008, .T. ) ;
#22936 = ADVANCED_FACE ( 'NONE', ( #29373 ), #16716, .T. ) ;
#22937 = AXIS2_PLACEMENT_3D ( 'NONE', #9079, #14010, #31408 ) ;
#22938 = CIRCLE ( 'NONE', #31852, 12.27641737965281798 ) ;
#22939 = VERTEX_POINT ( 'NONE', #6568 ) ;
#22940 = CARTESIAN_POINT ( 'NONE',  ( 55.09785597605721108, 14.86454579224779948, 47.04930799450051637 ) ) ;
#22941 = ORIENTED_EDGE ( 'NONE', *, *, #32441, .F. ) ;
#22942 = DIRECTION ( 'NONE',  ( 0.8746197071393926326, -0.4848096202463430537, -8.676864087101709653E-18 ) ) ;
#22943 = CARTESIAN_POINT ( 'NONE',  ( -40.02540636251513462, 2.839176264122873050, 37.04930799450052348 ) ) ;
#22944 = FACE_OUTER_BOUND ( 'NONE', #25256, .T. ) ;
#22945 = CARTESIAN_POINT ( 'NONE',  ( 44.74832014356462651, 26.28456182964376353, 46.92728461490987257 ) ) ;
#22946 = VERTEX_POINT ( 'NONE', #19511 ) ;
#22947 = AXIS2_PLACEMENT_3D ( 'NONE', #26075, #15749, #13617 ) ;
#22948 = EDGE_LOOP ( 'NONE', ( #7186, #30174 ) ) ;
#22949 = CIRCLE ( 'NONE', #30301, 2.000000000000001776 ) ;
#22950 = ORIENTED_EDGE ( 'NONE', *, *, #21322, .F. ) ;
#22951 = CARTESIAN_POINT ( 'NONE',  ( 49.87408856414482727, 24.84440440346269341, 46.61556741858395725 ) ) ;
#22952 = CARTESIAN_POINT ( 'NONE',  ( 54.27971259635813084, 0.05876815387847823813, 100.8802911971805258 ) ) ;
#22953 = DIRECTION ( 'NONE',  ( -1.000000000000000000, -1.101824276508909764E-16, 0.000000000000000000 ) ) ;
#22954 = AXIS2_PLACEMENT_3D ( 'NONE', #27941, #5301, #25151 ) ;
#22955 = AXIS2_PLACEMENT_3D ( 'NONE', #26239, #11795, #31173 ) ;
#22956 = LINE ( 'NONE', #10338, #6311 ) ;
#22957 = CARTESIAN_POINT ( 'NONE',  ( 21.09992658989238734, 38.56284415653841791, 47.04930799450051637 ) ) ;
#22958 = PRODUCT_CONTEXT ( 'NONE', #93, 'mechanical' ) ;
#22959 = ORIENTED_EDGE ( 'NONE', *, *, #3807, .T. ) ;
#22960 = DIRECTION ( 'NONE',  ( 1.000000000000000000, 0.000000000000000000, 0.000000000000000000 ) ) ;
#22961 = CYLINDRICAL_SURFACE ( 'NONE', #28240, 12.36707279061065101 ) ;
#22962 = AXIS2_PLACEMENT_3D ( 'NONE', #5807, #5638, #8584 ) ;
#22963 = CARTESIAN_POINT ( 'NONE',  ( 21.09992658989239089, 29.71664230456640254, 47.04930799450051637 ) ) ;
#22964 = CARTESIAN_POINT ( 'NONE',  ( 48.18662509608405742, 26.58284706826093569, 49.18364984542562013 ) ) ;
#22965 = ORIENTED_EDGE ( 'NONE', *, *, #1214, .T. ) ;
#22966 = CARTESIAN_POINT ( 'NONE',  ( 33.46699938050303302, 38.56284415653841791, 47.04930799450051637 ) ) ;
#22967 = CARTESIAN_POINT ( 'NONE',  ( 47.09785597605719687, 20.36454579224780304, 47.04930799450078638 ) ) ;
#22968 = EDGE_CURVE ( 'NONE', #4406, #3003, #23951, .T. ) ;
#22969 = CARTESIAN_POINT ( 'NONE',  ( -31.54952026363617179, 11.92645593095197754, 26.10458935450218831 ) ) ;
#22970 = ORIENTED_EDGE ( 'NONE', *, *, #5793, .F. ) ;
#22971 = EDGE_CURVE ( 'NONE', #18805, #22848, #26120, .T. ) ;
#22972 = EDGE_CURVE ( 'NONE', #15854, #32455, #27065, .T. ) ;
#22973 = EDGE_CURVE ( 'NONE', #18982, #31760, #18765, .T. ) ;
#22974 = EDGE_CURVE ( 'NONE', #3661, #28974, #4091, .T. ) ;
#22975 = AXIS2_PLACEMENT_3D ( 'NONE', #10364, #14522, #30386 ) ;
#22976 = AXIS2_PLACEMENT_3D ( 'NONE', #25289, #27586, #13143 ) ;
#22977 = ORIENTED_EDGE ( 'NONE', *, *, #982, .T. ) ;
#22978 = AXIS2_PLACEMENT_3D ( 'NONE', #9205, #19691, #14134 ) ;
#22979 = AXIS2_PLACEMENT_3D ( 'NONE', #3390, #7847, #18009 ) ;
#22980 = ORIENTED_EDGE ( 'NONE', *, *, #22431, .F. ) ;
#22981 = B_SPLINE_CURVE_WITH_KNOTS ( 'NONE', 3,
 ( #30376, #22969, #7895, #489, #30544, #17897, #27913, #22758, #2253, #12602, #29997, #15215, #12273, #24738, #19636, #22265, #32295, #7512, #7673, #9643, #17666, #7832, #15379, #24904, #17512, #9806, #27686, #29667, #27527, #30162, #19800, #5048, #4715, #22594, #15056, #12769, #29833, #7341, #25063, #12437 ),
 .UNSPECIFIED., .F., .F.,
 ( 4, 2, 2, 2, 2, 2, 2, 2, 2, 2, 2, 2, 2, 2, 2, 2, 2, 2, 2, 4 ),
 ( 3.469446951953614189E-18, 0.001682718673271781573, 0.003365437346543559676, 0.005048156019815338430, 0.006730874693087115883, 0.008413593366358893336, 0.01009631203963067339, 0.01177903071290245171, 0.01346174938617423177, 0.01682718673271779708, 0.01850990540598957540, 0.02019262407926135719, 0.02103398341589724982, 0.02187534275253314245, 0.02271670208916903508, 0.02355806142580492771, 0.02439942076244081687, 0.02524078009907670950, 0.02608213943571260213, 0.02692349877234849476 ),
 .UNSPECIFIED. ) ;
#22982 = DIRECTION ( 'NONE',  ( -1.188208965918165239E-16, -1.880121038077812885E-16, -1.000000000000000000 ) ) ;
#22983 = LINE ( 'NONE', #498, #25529 ) ;
#22984 = LINE ( 'NONE', #15594, #18340 ) ;
#22985 = CIRCLE ( 'NONE', #13054, 2.000000000000001776 ) ;
#22986 = ORIENTED_EDGE ( 'NONE', *, *, #18561, .F. ) ;
#22987 = CARTESIAN_POINT ( 'NONE',  ( 21.09992658989238734, 31.59184655352418503, 47.04930799450051637 ) ) ;
#22988 = CARTESIAN_POINT ( 'NONE',  ( 21.09785597605719332, 48.06454579224779877, 47.04930799450051637 ) ) ;
#22989 = DIRECTION ( 'NONE',  ( -0.000000000000000000, -1.000000000000000000, -0.000000000000000000 ) ) ;
#22990 = EDGE_CURVE ( 'NONE', #29832, #22032, #1490, .T. ) ;
#22991 = CARTESIAN_POINT ( 'NONE',  ( 21.09992658989239089, 26.21183152705960140, 47.04930799450051637 ) ) ;
#22992 = CARTESIAN_POINT ( 'NONE',  ( -41.93344242462055149, 13.82826554927147988, 59.53596428539564300 ) ) ;
#22993 = DIRECTION ( 'NONE',  ( 0.000000000000000000, 1.000000000000000000, -0.000000000000000000 ) ) ;
#22994 = CARTESIAN_POINT ( 'NONE',  ( -40.57832940339290673, 7.446916344587777736, 60.29072935073781991 ) ) ;
#22995 = CARTESIAN_POINT ( 'NONE',  ( 21.09785597605719332, 34.11266481626051217, 47.04930799450051637 ) ) ;
#22996 = DIRECTION ( 'NONE',  ( -1.000000000000000000, -1.101824276508909887E-16, 0.000000000000000000 ) ) ;
#22997 = DIRECTION ( 'NONE',  ( -1.101824276508909887E-16, 1.000000000000000000, -0.000000000000000000 ) ) ;
#22998 = CARTESIAN_POINT ( 'NONE',  ( 47.23302798462060537, 28.58121246473837473, 44.44659793406428605 ) ) ;
#22999 = SURFACE_STYLE_FILL_AREA ( #42 ) ;
#23000 = ORIENTED_EDGE ( 'NONE', *, *, #26483, .T. ) ;
#23001 = ORIENTED_EDGE ( 'NONE', *, *, #18885, .F. ) ;
#23002 = ADVANCED_FACE ( 'NONE', ( #4577 ), #21968, .F. ) ;
#23003 = CYLINDRICAL_SURFACE ( 'NONE', #14486, 27.99999999999999645 ) ;
#23004 = CARTESIAN_POINT ( 'NONE',  ( 21.09785597605719332, -15.93545420775219945, -25.45069200549945165 ) ) ;
#23005 = AXIS2_PLACEMENT_3D ( 'NONE', #17810, #5666, #15671 ) ;
#23006 = CIRCLE ( 'NONE', #18213, 2.500000000000002220 ) ;
#23007 = DIRECTION ( 'NONE',  ( 0.000000000000000000, 0.000000000000000000, -1.000000000000000000 ) ) ;
#23008 = EDGE_LOOP ( 'NONE', ( #5757, #9480, #12148, #20173 ) ) ;
#23009 = CARTESIAN_POINT ( 'NONE',  ( -39.51006936586720286, -5.935674496966103497, 77.97486924391246532 ) ) ;
#23010 = CARTESIAN_POINT ( 'NONE',  ( 47.43556129377199682, 23.11533908250407165, 46.87703799288242124 ) ) ;
#23011 = CARTESIAN_POINT ( 'NONE',  ( -40.06118906035621308, 6.942907937678849173, 39.10569540309890613 ) ) ;
#23012 = ORIENTED_EDGE ( 'NONE', *, *, #20155, .F. ) ;
#23013 = ORIENTED_EDGE ( 'NONE', *, *, #14475, .F. ) ;
#23014 = DIRECTION ( 'NONE',  ( 0.4848096202463429427, 0.8746197071393925215, -2.352477780477436787E-16 ) ) ;
#23015 = CARTESIAN_POINT ( 'NONE',  ( 48.40186567930498285, 26.11618040159426357, 45.03923535223908203 ) ) ;
#23016 = CARTESIAN_POINT ( 'NONE',  ( 45.24946171279598417, 29.12124452788248163, 47.99220971130007030 ) ) ;
#23017 = CARTESIAN_POINT ( 'NONE',  ( -39.40510812339053359, -5.935838084272694992, 77.96604415839914282 ) ) ;
#23018 = EDGE_CURVE ( 'NONE', #30053, #14586, #26911, .T. ) ;
#23019 = ORIENTED_EDGE ( 'NONE', *, *, #30808, .F. ) ;
#23020 = FACE_OUTER_BOUND ( 'NONE', #1264, .T. ) ;
#23021 = CARTESIAN_POINT ( 'NONE',  ( 7.282982007932096380, 15.57592086119046826, 47.04930799450052348 ) ) ;
#23022 = AXIS2_PLACEMENT_3D ( 'NONE', #29167, #16521, #11772 ) ;
#23023 = AXIS2_PLACEMENT_3D ( 'NONE', #6628, #13701, #1205 ) ;
#23024 = ORIENTED_EDGE ( 'NONE', *, *, #14839, .F. ) ;
#23025 = CARTESIAN_POINT ( 'NONE',  ( 45.00053793792376666, 26.65920399681023056, 45.68869892245983522 ) ) ;
#23026 = DIRECTION ( 'NONE',  ( -1.224646799147353207E-16, -1.349345573449484691E-32, 1.000000000000000000 ) ) ;
#23027 = EDGE_CURVE ( 'NONE', #26705, #7293, #17757, .T. ) ;
#23028 = AXIS2_PLACEMENT_3D ( 'NONE', #2188, #4979, #22201 ) ;
#23029 = ORIENTED_EDGE ( 'NONE', *, *, #30440, .T. ) ;
#23030 = AXIS2_PLACEMENT_3D ( 'NONE', #17360, #15991, #20911 ) ;
#23031 = DIRECTION ( 'NONE',  ( 1.000000000000000000, 0.000000000000000000, 0.000000000000000000 ) ) ;
#23032 = CARTESIAN_POINT ( 'NONE',  ( 80.43047408610513571, -5.903366343041404285, 78.33353586572610538 ) ) ;
#23033 = CYLINDRICAL_SURFACE ( 'NONE', #7857, 12.62506659569710266 ) ;
#23034 = AXIS2_PLACEMENT_3D ( 'NONE', #22615, #10155, #20149 ) ;
#23035 = CARTESIAN_POINT ( 'NONE',  ( -1.513221900615301818, 11.69718155787697533, -4.169217829025758881 ) ) ;
#23036 = DIRECTION ( 'NONE',  ( 0.8746197071393926326, -0.4848096202463430537, -8.676864087101709653E-18 ) ) ;
#23037 = ORIENTED_EDGE ( 'NONE', *, *, #20380, .F. ) ;
#23038 = CIRCLE ( 'NONE', #1545, 12.27641737965287838 ) ;
#23039 = EDGE_CURVE ( 'NONE', #16313, #31740, #21418, .T. ) ;
#23040 = CARTESIAN_POINT ( 'NONE',  ( 77.29794470067753309, -4.853532562205578493, 80.02403050357165171 ) ) ;
#23041 = DIRECTION ( 'NONE',  ( -0.000000000000000000, -1.000000000000000000, 0.000000000000000000 ) ) ;
#23042 = EDGE_CURVE ( 'NONE', #22928, #30572, #17237, .T. ) ;
#23043 = DIRECTION ( 'NONE',  ( -1.000000000000000000, 0.000000000000000000, 0.000000000000000000 ) ) ;
#23044 = CARTESIAN_POINT ( 'NONE',  ( 21.09992658989239089, 25.71183152705960140, 47.04930799450051637 ) ) ;
#23045 = CARTESIAN_POINT ( 'NONE',  ( -42.38687957179150345, 4.148162238788003719, 57.04930799450051637 ) ) ;
#23046 = ORIENTED_EDGE ( 'NONE', *, *, #32315, .T. ) ;
#23047 = DIRECTION ( 'NONE',  ( 0.000000000000000000, 0.000000000000000000, -1.000000000000000000 ) ) ;
#23048 = DIRECTION ( 'NONE',  ( -1.000000000000000000, 0.000000000000000000, 0.000000000000000000 ) ) ;
#23049 = ORIENTED_EDGE ( 'NONE', *, *, #11386, .F. ) ;
#23050 = CARTESIAN_POINT ( 'NONE',  ( 8.698509210239501854, 23.59164230456639544, 47.04930799450051637 ) ) ;
#23051 = DIRECTION ( 'NONE',  ( -1.000000000000000000, 0.000000000000000000, 0.000000000000000000 ) ) ;
#23052 = VECTOR ( 'NONE', #15649, 1000.000000000000000 ) ;
#23053 = DIRECTION ( 'NONE',  ( -0.000000000000000000, -0.000000000000000000, 1.000000000000000000 ) ) ;
#23054 = CARTESIAN_POINT ( 'NONE',  ( 53.97939423941235049, -4.961365878511737826, -10.19931710281307247 ) ) ;
#23055 = ORIENTED_EDGE ( 'NONE', *, *, #22117, .F. ) ;
#23056 = CARTESIAN_POINT ( 'NONE',  ( 48.78406556707242459, 22.93807716476589675, 47.13688154746046166 ) ) ;
#23057 = ORIENTED_EDGE ( 'NONE', *, *, #13760, .T. ) ;
#23058 = ADVANCED_FACE ( 'NONE', ( #4423 ), #16185, .T. ) ;
#23059 = AXIS2_PLACEMENT_3D ( 'NONE', #15062, #5053, #11943 ) ;
#23060 = CIRCLE ( 'NONE', #25692, 0.7905694150421027633 ) ;
#23061 = ORIENTED_EDGE ( 'NONE', *, *, #6004, .F. ) ;
#23062 = AXIS2_PLACEMENT_3D ( 'NONE', #22682, #4964, #5455 ) ;
#23063 = VECTOR ( 'NONE', #11786, 1000.000000000000000 ) ;
#23064 = CIRCLE ( 'NONE', #7898, 67.32891250266496286 ) ;
#23065 =( BOUNDED_SURFACE ( )  B_SPLINE_SURFACE ( 3, 2, ( 
 ( #3903, #13929, #29179 ),
 ( #9315, #16533, #21129 ),
 ( #26231, #11452, #21450 ),
 ( #31486, #14088, #8679 ),
 ( #18669, #3578, #9153 ),
 ( #31652, #23608, #23924 ),
 ( #1435, #24084, #3743 ),
 ( #31323, #11147, #8827 ),
 ( #28690, #1602, #8994 ),
 ( #16211, #11623, #19152 ) ),
 .UNSPECIFIED., .F., .F., .T. ) 
 B_SPLINE_SURFACE_WITH_KNOTS ( ( 4, 2, 2, 2, 4 ),
 ( 3, 3 ),
 ( -1.680513367352531873E-18, 0.0003347409949942531512, 0.0006694819899885080371, 0.001004222984982762815, 0.001338963979977017809 ),
 ( 0.000000000000000000, 1.000000000000000000 ),
 .UNSPECIFIED. ) 
 GEOMETRIC_REPRESENTATION_ITEM ( )  RATIONAL_B_SPLINE_SURFACE ( (
 ( 1.000000000000000000, 0.7071067811865460184, 1.000000000000000000),
 ( 1.000000000000000000, 0.7102524952744432296, 1.000000000000000000),
 ( 1.000000000000000000, 0.7282169120239688764, 1.000000000000000000),
 ( 1.000000000000000000, 0.7754022835990964646, 1.000000000000000000),
 ( 1.000000000000000000, 0.8043059223103944388, 1.000000000000000000),
 ( 1.000000000000000000, 0.8571167854599045510, 1.000000000000000000),
 ( 1.000000000000000000, 0.8816198077921589826, 1.000000000000000000),
 ( 1.000000000000000000, 0.9175117844828227787, 1.000000000000000000),
 ( 1.000000000000000000, 0.9295466150067912547, 1.000000000000000000),
 ( 1.000000000000000000, 0.9308844615755744734, 1.000000000000000000) ) ) 
 REPRESENTATION_ITEM ( '' )  SURFACE ( )  );
#23066 = EDGE_CURVE ( 'NONE', #12208, #31745, #27716, .T. ) ;
#23067 = CARTESIAN_POINT ( 'NONE',  ( 33.46699938050304013, 29.72145308207318237, 47.04930799450050927 ) ) ;
#23068 = CARTESIAN_POINT ( 'NONE',  ( -9.813471072924700778, -5.936918610400975460, 107.7389212035124046 ) ) ;
#23069 = CARTESIAN_POINT ( 'NONE',  ( -38.36853489569023168, 7.065850718397949315, 32.14930799450051779 ) ) ;
#23070 = AXIS2_PLACEMENT_3D ( 'NONE', #11215, #31243, #8742 ) ;
#23071 = ADVANCED_FACE ( 'NONE', ( #1466 ), #24282, .F. ) ;
#23072 = VERTEX_POINT ( 'NONE', #16562 ) ;
#23073 = DIRECTION ( 'NONE',  ( -1.000000000000000000, 0.000000000000000000, 0.000000000000000000 ) ) ;
#23074 = EDGE_LOOP ( 'NONE', ( #16081, #22718, #23272, #15922 ) ) ;
#23075 = CARTESIAN_POINT ( 'NONE',  ( -40.23971823762673239, 6.784144620117123381, 60.54930799450051637 ) ) ;
#23076 = CARTESIAN_POINT ( 'NONE',  ( -41.94956971822180947, 3.905757428664828890, 47.04930799450051637 ) ) ;
#23077 = CARTESIAN_POINT ( 'NONE',  ( -34.85155852797733189, -3.604462483032124354, 80.65629953933577667 ) ) ;
#23078 = DIRECTION ( 'NONE',  ( 0.000000000000000000, 0.000000000000000000, 1.000000000000000000 ) ) ;
#23079 = ORIENTED_EDGE ( 'NONE', *, *, #22509, .F. ) ;
#23080 = DIRECTION ( 'NONE',  ( -1.101824276508909887E-16, 1.000000000000000000, -0.000000000000000000 ) ) ;
#23081 = VERTEX_POINT ( 'NONE', #21650 ) ;
#23082 = CARTESIAN_POINT ( 'NONE',  ( -41.52218637998914375, 11.15499190493234671, 36.00717268343339583 ) ) ;
#23083 = CARTESIAN_POINT ( 'NONE',  ( 5.092160267343103897, 14.99513937955032716, 47.04930799450052348 ) ) ;
#23084 = EDGE_CURVE ( 'NONE', #5136, #10913, #12326, .T. ) ;
#23085 = VERTEX_POINT ( 'NONE', #4752 ) ;
#23086 = FACE_OUTER_BOUND ( 'NONE', #6379, .T. ) ;
#23087 = AXIS2_PLACEMENT_3D ( 'NONE', #24574, #14410, #29513 ) ;
#23088 = AXIS2_PLACEMENT_3D ( 'NONE', #10618, #21965, #4420 ) ;
#23089 = DIRECTION ( 'NONE',  ( 0.000000000000000000, 0.000000000000000000, -1.000000000000000000 ) ) ;
#23090 = CARTESIAN_POINT ( 'NONE',  ( -40.51522948349269626, 7.610540244934344223, 53.90050787996893433 ) ) ;
#23091 = DIRECTION ( 'NONE',  ( 0.000000000000000000, 0.000000000000000000, 1.000000000000000000 ) ) ;
#23092 = EDGE_CURVE ( 'NONE', #414, #21015, #32457, .T. ) ;
#23093 = CARTESIAN_POINT ( 'NONE',  ( 48.23388202445966755, 15.77906836436399374, 49.27628909396055690 ) ) ;
#23094 = VECTOR ( 'NONE', #31530, 1000.000000000000000 ) ;
#23095 = CARTESIAN_POINT ( 'NONE',  ( 21.09785597605719332, 6.574714862014670480, 67.18583656269663607 ) ) ;
#23096 = CARTESIAN_POINT ( 'NONE',  ( -40.66259927863561785, 6.843847033173870109, 34.78317517103428003 ) ) ;
#23097 = ORIENTED_EDGE ( 'NONE', *, *, #7038, .T. ) ;
#23098 = DIRECTION ( 'NONE',  ( -1.000000000000000000, 0.000000000000000000, 0.000000000000000000 ) ) ;
#23099 = AXIS2_PLACEMENT_3D ( 'NONE', #2973, #20541, #18226 ) ;
#23100 = DIRECTION ( 'NONE',  ( -2.779292025043186357E-18, 1.288349127009862211E-17, -1.000000000000000000 ) ) ;
#23101 = ORIENTED_EDGE ( 'NONE', *, *, #13951, .F. ) ;
#23102 = ORIENTED_EDGE ( 'NONE', *, *, #19616, .T. ) ;
#23103 = CARTESIAN_POINT ( 'NONE',  ( -5.930220226013869222, 9.437824910247670118, 98.40971065117005878 ) ) ;
#23104 = AXIS2_PLACEMENT_3D ( 'NONE', #14568, #8993, #4390 ) ;
#23105 = ORIENTED_EDGE ( 'NONE', *, *, #8844, .F. ) ;
#23106 = CIRCLE ( 'NONE', #31508, 0.1250000000000001110 ) ;
#23107 = AXIS2_PLACEMENT_3D ( 'NONE', #22924, #442, #9980 ) ;
#23108 = EDGE_LOOP ( 'NONE', ( #12785, #27149, #25888, #24667 ) ) ;
#23109 = AXIS2_PLACEMENT_3D ( 'NONE', #20210, #7429, #10536 ) ;
#23110 = EDGE_CURVE ( 'NONE', #110, #19940, #7701, .T. ) ;
#23111 = AXIS2_PLACEMENT_3D ( 'NONE', #15530, #20618, #25542 ) ;
#23112 = DIRECTION ( 'NONE',  ( -0.2756373558169947779, 0.9612616959383200044, 0.000000000000000000 ) ) ;
#23113 = CIRCLE ( 'NONE', #5300, 13.50178401536290806 ) ;
#23114 = EDGE_CURVE ( 'NONE', #14267, #5457, #17376, .T. ) ;
#23115 = ORIENTED_EDGE ( 'NONE', *, *, #4854, .T. ) ;
#23116 = CARTESIAN_POINT ( 'NONE',  ( 21.09785597605719332, 30.56454579224779522, 64.04930799450050927 ) ) ;
#23117 = FACE_OUTER_BOUND ( 'NONE', #22780, .T. ) ;
#23118 = FACE_OUTER_BOUND ( 'NONE', #7500, .T. ) ;
#23119 = CARTESIAN_POINT ( 'NONE',  ( 45.38854177497844944, 26.22622849631042996, 45.94041160078741370 ) ) ;
#23120 = ORIENTED_EDGE ( 'NONE', *, *, #20777, .T. ) ;
#23121 = ORIENTED_EDGE ( 'NONE', *, *, #6636, .T. ) ;
#23122 = DIRECTION ( 'NONE',  ( -1.000000000000000000, 0.000000000000000000, 0.000000000000000000 ) ) ;
#23123 = CIRCLE ( 'NONE', #8972, 13.20000000000000284 ) ;
#23124 = ADVANCED_FACE ( 'NONE', ( #12302 ), #15673, .F. ) ;
#23125 = ORIENTED_EDGE ( 'NONE', *, *, #30698, .F. ) ;
#23126 = DIRECTION ( 'NONE',  ( -1.224646799147353207E-16, -1.349345573449484691E-32, 1.000000000000000000 ) ) ;
#23127 = CARTESIAN_POINT ( 'NONE',  ( 49.03637579218595732, 8.583949016299408541, 98.45931519117756636 ) ) ;
#23128 = CARTESIAN_POINT ( 'NONE',  ( 21.09785597605719332, 15.24673779880127178, 47.04930799450051637 ) ) ;
#23129 = MANIFOLD_SOLID_BREP ( 'Stock-MAT-060-1', #15277 ) ;
#23130 = ADVANCED_FACE ( 'NONE', ( #17870 ), #30030, .F. ) ;
#23131 = CARTESIAN_POINT ( 'NONE',  ( -2.057288477451015840, 11.55930814891847902, -4.886607555839500350 ) ) ;
#23132 = DIRECTION ( 'NONE',  ( 0.8746197071393926326, -0.4848096202463430537, -8.676864087101709653E-18 ) ) ;
#23133 = ORIENTED_EDGE ( 'NONE', *, *, #17571, .F. ) ;
#23134 = CARTESIAN_POINT ( 'NONE',  ( 33.50134396954527460, 24.34164230456639544, 47.04930799450051637 ) ) ;
#23135 = FACE_BOUND ( 'NONE', #11657, .T. ) ;
#23136 = DIRECTION ( 'NONE',  ( 0.8746197071393926326, -0.4848096202463430537, -8.676864087101709653E-18 ) ) ;
#23137 = CARTESIAN_POINT ( 'NONE',  ( 33.37634396954526039, 25.59164230456639899, 47.04930799450051637 ) ) ;
#23138 = CIRCLE ( 'NONE', #87, 5.499019513592787511 ) ;
#23139 = ORIENTED_EDGE ( 'NONE', *, *, #7160, .T. ) ;
#23140=STYLED_ITEM('',(#32522),#11688);
#23141 = DIRECTION ( 'NONE',  ( -1.101824276508909887E-16, 1.000000000000000000, -0.000000000000000000 ) ) ;
#23142 = CLOSED_SHELL ( 'NONE', ( #25022, #30108, #1888, #3809, #25391, #26007 ) ) ;
#23143 = AXIS2_PLACEMENT_3D ( 'NONE', #28982, #3707, #14217 ) ;
#23144 = DIRECTION ( 'NONE',  ( -1.101824276508909887E-16, 1.000000000000000000, -0.000000000000000000 ) ) ;
#23145 = VERTEX_POINT ( 'NONE', #25259 ) ;
#23146 = CIRCLE ( 'NONE', #24191, 0.09999999999999896472 ) ;
#23147 = ORIENTED_EDGE ( 'NONE', *, *, #29579, .F. ) ;
#23148 = ORIENTED_EDGE ( 'NONE', *, *, #3517, .F. ) ;
#23149 = DIRECTION ( 'NONE',  ( 0.000000000000000000, -0.2964022880492245271, -0.9550631830613013351 ) ) ;
#23150 = CARTESIAN_POINT ( 'NONE',  ( 21.09992658989239089, 25.84164230456639899, 47.04930799450051637 ) ) ;
#23151 = CARTESIAN_POINT ( 'NONE',  ( 8.823509210239588896, 32.59164230456639899, 47.04930799450051637 ) ) ;
#23152 = VERTEX_POINT ( 'NONE', #12958 ) ;
#23153 = AXIS2_PLACEMENT_3D ( 'NONE', #24043, #27002, #6654 ) ;
#23154 = CARTESIAN_POINT ( 'NONE',  ( 17.44491328785239048, -13.30632128221581034, 102.8621610177830519 ) ) ;
#23155 = CONICAL_SURFACE ( 'NONE', #6918, 31.29999999999997939, 0.7853981633974482790 ) ;
#23156 = CARTESIAN_POINT ( 'NONE',  ( 21.09785597605719332, 12.78350261226561280, 47.04930799450051637 ) ) ;
#23157 = CARTESIAN_POINT ( 'NONE',  ( -42.38687957179149635, 4.148162238787999279, 37.04930799450052348 ) ) ;
#23158 = CARTESIAN_POINT ( 'NONE',  ( 21.09785597605719332, -16.43042895458278352, 47.04930799450051637 ) ) ;
#23159 = EDGE_CURVE ( 'NONE', #9936, #19822, #30890, .T. ) ;
#23160 = DIRECTION ( 'NONE',  ( 0.000000000000000000, 0.000000000000000000, -1.000000000000000000 ) ) ;
#23161 = DIRECTION ( 'NONE',  ( 0.4848096202463429427, 0.8746197071393925215, -2.352477780477436294E-16 ) ) ;
#23162 = CARTESIAN_POINT ( 'NONE',  ( 75.19785597605721250, 14.86454579224779948, 47.04930799450051637 ) ) ;
#23163 = ADVANCED_FACE ( 'NONE', ( #27722 ), #1006, .T. ) ;
#23164 = CARTESIAN_POINT ( 'NONE',  ( 48.10030433005226769, 29.45850404830353142, 49.01443330185325920 ) ) ;
#23166 = ADVANCED_FACE ( 'NONE', ( #22304 ), #25098, .T. ) ;
#23165 = CARTESIAN_POINT ( 'NONE',  ( 21.09992658989239089, 26.47145308207318593, 47.04930799450051637 ) ) ;
#23167 = ADVANCED_FACE ( 'NONE', ( #10492 ), #10440, .F. ) ;
#23168 = DIRECTION ( 'NONE',  ( 1.000000000000000000, 0.000000000000000000, 0.000000000000000000 ) ) ;
#23169 = CARTESIAN_POINT ( 'NONE',  ( 47.79865503179234310, 9.702389020015065313, -4.315940132965163656 ) ) ;
#23170 = EDGE_LOOP ( 'NONE', ( #6307, #2607, #3074, #26915 ) ) ;
#23171 = ORIENTED_EDGE ( 'NONE', *, *, #3134, .F. ) ;
#23172 = CARTESIAN_POINT ( 'NONE',  ( -42.50084779003665147, 14.56798984196178637, 37.04930799450052348 ) ) ;
#23173 = AXIS2_PLACEMENT_3D ( 'NONE', #23729, #1084, #8787 ) ;
#23174 = CARTESIAN_POINT ( 'NONE',  ( 21.09785597605720753, 14.86454579224779948, 47.04930799450052348 ) ) ;
#23175 = FACE_BOUND ( 'NONE', #21952, .T. ) ;
#23176 = VECTOR ( 'NONE', #26950, 1000.000000000000000 ) ;
#23177 = VERTEX_POINT ( 'NONE', #32488 ) ;
#23178 = DIRECTION ( 'NONE',  ( 1.000000000000000000, 0.000000000000000000, 0.000000000000000000 ) ) ;
#23179 = CARTESIAN_POINT ( 'NONE',  ( -41.88090303775678080, 13.82677487427665497, 54.64930799450051779 ) ) ;
#23180 = ORIENTED_EDGE ( 'NONE', *, *, #4530, .F. ) ;
#23181 = ORIENTED_EDGE ( 'NONE', *, *, #22709, .F. ) ;
#23182 = DIRECTION ( 'NONE',  ( -0.000000000000000000, 1.000000000000000000, -0.000000000000000000 ) ) ;
#23183 = CARTESIAN_POINT ( 'NONE',  ( 48.40186567930498285, 27.51618040159426570, 45.03923535223908203 ) ) ;
#23184 = CARTESIAN_POINT ( 'NONE',  ( 45.24946171279598417, 28.42124452788248234, 47.99220971130007030 ) ) ;
#23185 = TOROIDAL_SURFACE ( 'NONE', #30527, 12.40141737965287128, 0.1249999999999993477 ) ;
#23186 = CARTESIAN_POINT ( 'NONE',  ( -34.71505847545616064, 11.47745911305554145, 52.78077050074096377 ) ) ;
#23187 = VECTOR ( 'NONE', #4073, 1000.000000000000000 ) ;
#23188 = ORIENTED_EDGE ( 'NONE', *, *, #26379, .T. ) ;
#23189 = DIRECTION ( 'NONE',  ( -1.101824276508909887E-16, 1.000000000000000000, -0.000000000000000000 ) ) ;
#23190 = ADVANCED_FACE ( 'NONE', ( #7546 ), #17541, .F. ) ;
#23191 = CARTESIAN_POINT ( 'NONE',  ( 33.50134396954526750, 25.09164230456639899, 47.04930799450051637 ) ) ;
#23192 = EDGE_LOOP ( 'NONE', ( #28651, #27285 ) ) ;
#23193 = AXIS2_PLACEMENT_3D ( 'NONE', #31528, #19028, #29057 ) ;
#23194 = CARTESIAN_POINT ( 'NONE',  ( 21.09785597605719332, 11.92558985988973497, 47.04930799450051637 ) ) ;
#23196 = DIRECTION ( 'NONE',  ( -0.2756373558170082672, 0.9612616959383162296, 0.000000000000000000 ) ) ;
#23195 = VECTOR ( 'NONE', #8228, 1000.000000000000114 ) ;
#23197 = DIRECTION ( 'NONE',  ( -1.101824276508909887E-16, 1.000000000000000000, -0.000000000000000000 ) ) ;
#23198 = AXIS2_PLACEMENT_3D ( 'NONE', #12929, #2421, #22422 ) ;
#23199 = EDGE_LOOP ( 'NONE', ( #6330, #3072, #2059, #28191, #14835 ) ) ;
#23200 = CARTESIAN_POINT ( 'NONE',  ( -41.10400476907452116, 9.333823787025618657, 38.63215070697513909 ) ) ;
#23201 = ADVANCED_FACE ( 'NONE', ( #3566 ), #2766, .T. ) ;
#23203 = EDGE_CURVE ( 'NONE', #10661, #14676, #29309, .T. ) ;
#23202 = DIRECTION ( 'NONE',  ( -2.779292025043186357E-18, 1.288349127009862211E-17, -1.000000000000000000 ) ) ;
#23204 = EDGE_CURVE ( 'NONE', #28894, #30447, #28046, .T. ) ;
#23205 = AXIS2_PLACEMENT_3D ( 'NONE', #26200, #28360, #3722 ) ;
#23206 = DIRECTION ( 'NONE',  ( -1.000000000000000000, 0.000000000000000000, 0.000000000000000000 ) ) ;
#23207 = EDGE_CURVE ( 'NONE', #28560, #10403, #5186, .T. ) ;
#23208 = LINE ( 'NONE', #30446, #21211 ) ;
#23209 = ORIENTED_EDGE ( 'NONE', *, *, #22972, .T. ) ;
#23210 = DIRECTION ( 'NONE',  ( 0.9612616959383200044, 0.2756373558169954996, -1.660411357259285896E-16 ) ) ;
#23211 = PLANE ( 'NONE',  #24725 ) ;
#23212 = DIRECTION ( 'NONE',  ( 2.779292025043186357E-18, -1.288349127009862211E-17, 1.000000000000000000 ) ) ;
#23213 = CARTESIAN_POINT ( 'NONE',  ( -40.23397449525940317, 6.794506605641763564, 34.54930799450052348 ) ) ;
#23214 = CARTESIAN_POINT ( 'NONE',  ( -40.47579404106497236, 7.230063580211346874, 38.88540821492420463 ) ) ;
#23215 = EDGE_LOOP ( 'NONE', ( #32052, #7654, #26426, #356 ) ) ;
#23216 = DIRECTION ( 'NONE',  ( -0.2756373558169947779, 0.9612616959383200044, 0.000000000000000000 ) ) ;
#23217 = CARTESIAN_POINT ( 'NONE',  ( 33.72499318558949710, 28.09143805560861296, 47.04930799450051637 ) ) ;
#23218 = CARTESIAN_POINT ( 'NONE',  ( -42.67312000749024747, 15.16877446138198238, 35.54930799450051637 ) ) ;
#23219 = EDGE_LOOP ( 'NONE', ( #7672, #23427, #16567, #21275 ) ) ;
#23220 = DIRECTION ( 'NONE',  ( -1.101824276508909887E-16, 1.000000000000000000, -0.000000000000000000 ) ) ;
#23221 = FACE_OUTER_BOUND ( 'NONE', #7793, .T. ) ;
#23222 = DIRECTION ( 'NONE',  ( -0.2756373558170082672, 0.9612616959383162296, 0.000000000000000000 ) ) ;
#23223 = CARTESIAN_POINT ( 'NONE',  ( 49.86503751672583462, 7.651854857429027490, -4.493960750487066669 ) ) ;
#23224 = CIRCLE ( 'NONE', #23733, 0.1000000000000018235 ) ;
#23225 = EDGE_LOOP ( 'NONE', ( #26012, #21407, #16127, #1548 ) ) ;
#23226 = B_SPLINE_SURFACE_WITH_KNOTS ( 'NONE', 3, 1, ( 
 ( #20770, #30786 ),
 ( #28004, #20442 ),
 ( #25700, #30475 ),
 ( #17983, #13077 ) ),
 .UNSPECIFIED., .F., .F., .F.,
 ( 4, 4 ),
 ( 2, 2 ),
 ( 0.9911194921636323762, 1.000000000000000000 ),
 ( 0.000000000000000000, 1.000000000000000000 ),
 .UNSPECIFIED. ) ;
#23227 = CARTESIAN_POINT ( 'NONE',  ( -40.60333149162104860, 7.557375771971038603, 60.08350751967649472 ) ) ;
#23228 = ORIENTED_EDGE ( 'NONE', *, *, #25318, .T. ) ;
#23229 = CIRCLE ( 'NONE', #26360, 1.300000000000002487 ) ;
#23230 = EDGE_LOOP ( 'NONE', ( #30094, #5183, #17065, #21931, #20915 ) ) ;
#23231 = AXIS2_PLACEMENT_3D ( 'NONE', #19908, #30259, #19739 ) ;
#23232 = CIRCLE ( 'NONE', #14328, 13.23540278830031447 ) ;
#23233 = EDGE_CURVE ( 'NONE', #8765, #14556, #19309, .T. ) ;
#23234 = EDGE_CURVE ( 'NONE', #30824, #29832, #15143, .T. ) ;
#23235 = DIRECTION ( 'NONE',  ( -1.000000000000000000, 0.000000000000000000, 0.000000000000000000 ) ) ;
#23236 = DIRECTION ( 'NONE',  ( 1.000000000000000000, 0.000000000000000000, 2.775557561562888984E-15 ) ) ;
#23237 = CARTESIAN_POINT ( 'NONE',  ( -4.902144023942810236, 25.56454579224779877, 44.54930799450078638 ) ) ;
#23238 = EDGE_LOOP ( 'NONE', ( #31510, #25812, #13923, #15484 ) ) ;
#23239 = CARTESIAN_POINT ( 'NONE',  ( -34.71177954129748855, 11.48555665516351354, 41.32782006312588408 ) ) ;
#23240 = ORIENTED_EDGE ( 'NONE', *, *, #14046, .T. ) ;
#23241 = TOROIDAL_SURFACE ( 'NONE', #30590, 55.78321279447762748, 0.1000000000000016986 ) ;
#23242 = LINE ( 'NONE', #13555, #11498 ) ;
#23243 = FACE_OUTER_BOUND ( 'NONE', #22903, .T. ) ;
#23244 = CARTESIAN_POINT ( 'NONE',  ( -33.46773820220050766, -1.490757911476732867, 80.67629718822401230 ) ) ;
#23245 = CIRCLE ( 'NONE', #5889, 2.000000000000001776 ) ;
#23246 = DIRECTION ( 'NONE',  ( 1.000000000000000000, 0.000000000000000000, 0.000000000000000000 ) ) ;
#23247 = EDGE_CURVE ( 'NONE', #22296, #4270, #25633, .T. ) ;
#23248 = ORIENTED_EDGE ( 'NONE', *, *, #2155, .F. ) ;
#23249 = DIRECTION ( 'NONE',  ( 1.000000000000000000, 0.000000000000000000, 0.000000000000000000 ) ) ;
#23250 = ORIENTED_EDGE ( 'NONE', *, *, #24310, .F. ) ;
#23251 = DIRECTION ( 'NONE',  ( 7.588956326749211550E-18, -4.206627182996912454E-18, 1.000000000000000000 ) ) ;
#23252 = DIRECTION ( 'NONE',  ( 0.000000000000000000, 0.000000000000000000, -1.000000000000000000 ) ) ;
#23253 = VERTEX_POINT ( 'NONE', #8189 ) ;
#23254 = CARTESIAN_POINT ( 'NONE',  ( 21.09785597605719332, 43.56454579224774193, 47.04930799450051637 ) ) ;
#23255 = DIRECTION ( 'NONE',  ( -1.000000000000000000, 0.000000000000000000, 0.000000000000000000 ) ) ;
#23256 = DIRECTION ( 'NONE',  ( 0.4848096202463429982, 0.8746197071393925215, -4.250072516143176149E-17 ) ) ;
#23257 = DIRECTION ( 'NONE',  ( 0.000000000000000000, 0.000000000000000000, -1.000000000000000000 ) ) ;
#23258 = CIRCLE ( 'NONE', #9099, 0.1250000000000001110 ) ;
#23259 = CIRCLE ( 'NONE', #9100, 0.1000000000000006301 ) ;
#23260 = CARTESIAN_POINT ( 'NONE',  ( 21.09785597605719332, 43.56454579224774193, 47.04930799450051637 ) ) ;
#23261 = CARTESIAN_POINT ( 'NONE',  ( -41.13768170161382898, 11.26524684725914227, 35.90717268343339441 ) ) ;
#23262 = ORIENTED_EDGE ( 'NONE', *, *, #20283, .F. ) ;
#23263 = CYLINDRICAL_SURFACE ( 'NONE', #22979, 2.499999999999997335 ) ;
#23264 = VERTEX_POINT ( 'NONE', #5890 ) ;
#23265 = DIRECTION ( 'NONE',  ( -1.000000000000000000, 0.000000000000000000, 0.000000000000000000 ) ) ;
#23266 = VERTEX_POINT ( 'NONE', #15894 ) ;
#23267 = ADVANCED_FACE ( 'NONE', ( #25900 ), #20965, .T. ) ;
#23268 = ORIENTED_EDGE ( 'NONE', *, *, #25320, .T. ) ;
#23269 = CARTESIAN_POINT ( 'NONE',  ( -6.842391073119661549, 8.582373042058234702, 98.45937169672181710 ) ) ;
#23270 = UNCERTAINTY_MEASURE_WITH_UNIT (LENGTH_MEASURE( 1.000000000000000082E-05 ), #13173, 'distance_accuracy_value', 'NONE');
#23271 = EDGE_CURVE ( 'NONE', #31078, #29942, #946, .T. ) ;
#23272 = ORIENTED_EDGE ( 'NONE', *, *, #17331, .T. ) ;
#23273 = B_SPLINE_CURVE_WITH_KNOTS ( 'NONE', 3,
 ( #31115, #13399, #3854, #23395, #20769, #902, #3689, #5848, #15851, #8464, #16005, #28487, #28804, #18615, #1220, #16318, #21238, #31271, #26987, #4503, #6479, #31754, #19430, #9268, #19257, #26656, #7132, #2207, #32082, #24516, #31916, #12058, #9103, #14689, #14521, #27144, #24196, #17126, #19093, #22054, #29130, #1716, #14030, #26825, #9596, #24030, #2039, #19593 ),
 .UNSPECIFIED., .F., .F.,
 ( 4, 2, 2, 2, 2, 2, 2, 2, 2, 2, 2, 2, 2, 2, 2, 2, 2, 2, 2, 2, 2, 2, 2, 4 ),
 ( 0.000000000000000000, 0.0008877576229114608882, 0.001331636434367201687, 0.001775515245822942376, 0.002663272868734409878, 0.003551030491645877380, 0.004438788114557345316, 0.005326545737468812818, 0.006214303360380279452, 0.007102060983291746954, 0.008877576229114671549, 0.009765333852026134714, 0.01065309147493759788, 0.01242860672076051554, 0.01420412196658343493, 0.01597963721240634738, 0.01775515245822926677, 0.01953066770405217922, 0.02130618294987509861, 0.02308169819569801107, 0.02396945581860946903, 0.02485721344152092699, 0.02663272868734380475, 0.02840824393316667903 ),
 .UNSPECIFIED. ) ;
#23274 = EDGE_CURVE ( 'NONE', #23145, #22133, #3076, .T. ) ;
#23275 = ADVANCED_FACE ( 'NONE', ( #18975 ), #8982, .T. ) ;
#23276 = EDGE_CURVE ( 'NONE', #11074, #11047, #13576, .T. ) ;
#23277 = AXIS2_PLACEMENT_3D ( 'NONE', #14705, #12903, #7315 ) ;
#23278 = ORIENTED_EDGE ( 'NONE', *, *, #23814, .F. ) ;
#23279 = FACE_OUTER_BOUND ( 'NONE', #1117, .T. ) ;
#23280 = ORIENTED_EDGE ( 'NONE', *, *, #9157, .F. ) ;
#23281 = DIRECTION ( 'NONE',  ( -1.000000000000000000, 0.000000000000000000, 0.000000000000000000 ) ) ;
#23282 = DIRECTION ( 'NONE',  ( 0.8746197071393926326, -0.4848096202463430537, -8.676864087101709653E-18 ) ) ;
#23283 = DIRECTION ( 'NONE',  ( 0.2756373558170082672, -0.9612616959383162296, 0.000000000000000000 ) ) ;
#23284 = CARTESIAN_POINT ( 'NONE',  ( 44.74832014356462651, 26.98456182964376637, 46.92728461490987257 ) ) ;
#23285 = EDGE_CURVE ( 'NONE', #16262, #6052, #11441, .T. ) ;
#23286 = EDGE_LOOP ( 'NONE', ( #203, #7448, #18774, #12994, #2667, #15360 ) ) ;
#23287 = VERTEX_POINT ( 'NONE', #24236 ) ;
#23288 = CYLINDRICAL_SURFACE ( 'NONE', #18458, 0.1000000000000014905 ) ;
#23289 = VERTEX_POINT ( 'NONE', #6848 ) ;
#23290 = CARTESIAN_POINT ( 'NONE',  ( 42.60875976922299202, 11.86909835304794569, 99.49998532334635115 ) ) ;
#23291 = CYLINDRICAL_SURFACE ( 'NONE', #13280, 7.999999999999999112 ) ;
#23292 = AXIS2_PLACEMENT_3D ( 'NONE', #20044, #12515, #9556 ) ;
#23293 = LINE ( 'NONE', #6060, #1623 ) ;
#23294 = DIRECTION ( 'NONE',  ( 0.2155021956183755527, 0.9702957262759969170, -0.1099318300320483582 ) ) ;
#23295 = AXIS2_PLACEMENT_3D ( 'NONE', #15528, #22586, #107 ) ;
#23296 = VERTEX_POINT ( 'NONE', #11929 ) ;
#23297 = CARTESIAN_POINT ( 'NONE',  ( 21.09992658989239089, 24.34143805560860940, 47.04930799450051637 ) ) ;
#23298 = AXIS2_PLACEMENT_3D ( 'NONE', #28454, #8739, #3655 ) ;
#23299 = DIRECTION ( 'NONE',  ( -1.000000000000000000, -1.101824276508910010E-16, 0.000000000000000000 ) ) ;
#23300 = VECTOR ( 'NONE', #23149, 999.9999999999998863 ) ;
#23301 = CARTESIAN_POINT ( 'NONE',  ( 8.732853799281738105, 23.96183152705959785, 47.04930799450051637 ) ) ;
#23302 = CARTESIAN_POINT ( 'NONE',  ( -40.59689739711614465, 7.533859135569301202, 60.29072935073781991 ) ) ;
#23303 = EDGE_CURVE ( 'NONE', #7375, #306, #4664, .T. ) ;
#23304 = EDGE_LOOP ( 'NONE', ( #27362, #13554, #25013, #13471 ) ) ;
#23305 = DIRECTION ( 'NONE',  ( -1.101824276508909887E-16, 1.000000000000000000, -0.000000000000000000 ) ) ;
#23306 = DIRECTION ( 'NONE',  ( 0.000000000000000000, -1.000000000000000000, 0.000000000000000000 ) ) ;
#23307 = EDGE_CURVE ( 'NONE', #10175, #3984, #19137, .T. ) ;
#23308 = ORIENTED_EDGE ( 'NONE', *, *, #27010, .F. ) ;
#23309 = EDGE_CURVE ( 'NONE', #20897, #32154, #13070, .T. ) ;
#23310 = ORIENTED_EDGE ( 'NONE', *, *, #29621, .F. ) ;
#23311 = EDGE_CURVE ( 'NONE', #20144, #15199, #15695, .T. ) ;
#23312 = TOROIDAL_SURFACE ( 'NONE', #10226, 15.27594751018003194, 0.2551199516247882326 ) ;
#23313 = ORIENTED_EDGE ( 'NONE', *, *, #24457, .T. ) ;
#23314 = AXIS2_PLACEMENT_3D ( 'NONE', #999, #21010, #25624 ) ;
#23315 = DIRECTION ( 'NONE',  ( 1.000000000000000000, 0.000000000000000000, 0.000000000000000000 ) ) ;
#23316 = DIRECTION ( 'NONE',  ( -0.000000000000000000, -1.000000000000000000, -0.000000000000000000 ) ) ;
#23318 = CARTESIAN_POINT ( 'NONE',  ( 67.84785597605720397, 13.61454579224779771, 47.04930799450051637 ) ) ;
#23317 = CIRCLE ( 'NONE', #23820, 1.142135311067127512 ) ;
#23319 = CIRCLE ( 'NONE', #18567, 12.62506659569710443 ) ;
#23320 = CIRCLE ( 'NONE', #26453, 0.8999999999999991340 ) ;
#23321 = ORIENTED_EDGE ( 'NONE', *, *, #16555, .T. ) ;
#23322 = DIRECTION ( 'NONE',  ( -0.000000000000000000, -1.000000000000000000, -0.000000000000000000 ) ) ;
#23323 = CARTESIAN_POINT ( 'NONE',  ( -39.64148344771002286, 7.657122216028890982, 47.04930799450051637 ) ) ;
#23324 = DIRECTION ( 'NONE',  ( -0.9612616959383221138, -0.2756373558169876170, 0.000000000000000000 ) ) ;
#23325 = CARTESIAN_POINT ( 'NONE',  ( 21.09785597605719332, 25.56454579224779877, 21.04930799450051282 ) ) ;
#23326 = CARTESIAN_POINT ( 'NONE',  ( -37.74053575120161952, -5.821578765910089714, 78.65578092815914601 ) ) ;
#23327 = CARTESIAN_POINT ( 'NONE',  ( 21.09785597605720042, -16.63545420775220407, 47.04930799450051637 ) ) ;
#23328 = CARTESIAN_POINT ( 'NONE',  ( 21.09992658989239089, 27.71664230456639899, 47.04930799450051637 ) ) ;
#23329 = PLANE ( 'NONE',  #26240 ) ;
#23330 = DIRECTION ( 'NONE',  ( 0.000000000000000000, 0.000000000000000000, -1.000000000000000000 ) ) ;
#23331 = DIRECTION ( 'NONE',  ( 0.000000000000000000, -1.000000000000000000, 0.000000000000000000 ) ) ;
#23332 =( NAMED_UNIT ( * ) PLANE_ANGLE_UNIT ( ) SI_UNIT ( $, .RADIAN. ) );
#23333 = EDGE_LOOP ( 'NONE', ( #2032, #4990, #4447, #13704 ) ) ;
#23334 = VERTEX_POINT ( 'NONE', #16360 ) ;
#23335 = CARTESIAN_POINT ( 'NONE',  ( 74.06012918148381630, -13.30632128221581567, 65.03308317646937553 ) ) ;
#23336 = DIRECTION ( 'NONE',  ( -2.779292025043186357E-18, 1.288349127009862211E-17, -1.000000000000000000 ) ) ;
#23337 = CIRCLE ( 'NONE', #11289, 2.500000000000002220 ) ;
#23338 = EDGE_LOOP ( 'NONE', ( #20574, #21194, #24378, #10930 ) ) ;
#23339 = DIRECTION ( 'NONE',  ( -1.101824276508909887E-16, 1.000000000000000000, -0.000000000000000000 ) ) ;
#23340 = CARTESIAN_POINT ( 'NONE',  ( -40.65487266620045403, 9.475231293617262907, 34.66144002885648945 ) ) ;
#23341 = EDGE_LOOP ( 'NONE', ( #23604, #16573, #1479, #30949 ) ) ;
#23343 = AXIS2_PLACEMENT_3D ( 'NONE', #10830, #20820, #30844 ) ;
#23342 = DIRECTION ( 'NONE',  ( 0.8746197071393925215, -0.4848096202463429982, -8.676864087101708112E-18 ) ) ;
#23344 = CARTESIAN_POINT ( 'NONE',  ( 45.73035263060504718, 28.63954579807170475, 44.36855633853329550 ) ) ;
#23345 = AXIS2_PLACEMENT_3D ( 'NONE', #17474, #17956, #27493 ) ;
#23346 = AXIS2_PLACEMENT_3D ( 'NONE', #23886, #7096, #7435 ) ;
#23347 = CARTESIAN_POINT ( 'NONE',  ( 48.83862994770794330, 29.35457786121581591, 48.17861352429476796 ) ) ;
#23348 = CARTESIAN_POINT ( 'NONE',  ( -39.46892853597984896, -5.935610090285465823, 77.88162228658642050 ) ) ;
#23349 = AXIS2_PLACEMENT_3D ( 'NONE', #27639, #20245, #7957 ) ;
#23350 = B_SPLINE_CURVE_WITH_KNOTS ( 'NONE', 3,
 ( #10466, #17999, #10793, #28020, #20136, #30652, #2747, #25550, #7838, #10635, #20626, #20786 ),
 .UNSPECIFIED., .F., .F.,
 ( 4, 2, 2, 2, 2, 4 ),
 ( 0.000000000000000000, 7.696047042371321643E-05, 0.0001154407056355867789, 0.0001539209408474603413, 0.0002308814112711852671, 0.0003078418816949101658 ),
 .UNSPECIFIED. ) ;
#23351 = EDGE_CURVE ( 'NONE', #893, #25766, #15190, .T. ) ;
#23352 = ORIENTED_EDGE ( 'NONE', *, *, #14028, .F. ) ;
#23353 = DIRECTION ( 'NONE',  ( 0.000000000000000000, 1.000000000000000000, 0.000000000000000000 ) ) ;
#23354 = DIRECTION ( 'NONE',  ( -1.224646799147353207E-16, -1.349345573449484691E-32, 1.000000000000000000 ) ) ;
#23355 = VERTEX_POINT ( 'NONE', #6362 ) ;
#23356 = AXIS2_PLACEMENT_3D ( 'NONE', #32450, #17506, #31793 ) ;
#23357 = DIRECTION ( 'NONE',  ( -1.000000000000000000, 0.000000000000000000, 0.000000000000000000 ) ) ;
#23358 = DIRECTION ( 'NONE',  ( 0.000000000000000000, -1.251509963831984395E-16, 1.000000000000000000 ) ) ;
#23359 = CONICAL_SURFACE ( 'NONE', #19669, 19.04889477833696176, 0.8552113334772211140 ) ;
#23360 = CARTESIAN_POINT ( 'NONE',  ( 8.698509210239537381, 27.09164230456639899, 47.04930799450051637 ) ) ;
#23361 = EDGE_LOOP ( 'NONE', ( #9820, #993, #289, #29012 ) ) ;
#23362 = FACE_OUTER_BOUND ( 'NONE', #10038, .T. ) ;
#23363 = AXIS2_PLACEMENT_3D ( 'NONE', #21525, #1350, #16766 ) ;
#23364 = DIRECTION ( 'NONE',  ( -0.000000000000000000, -1.000000000000000000, -0.000000000000000000 ) ) ;
#23365 = DIRECTION ( 'NONE',  ( 0.000000000000000000, 1.000000000000000000, -0.000000000000000000 ) ) ;
#23366 = CARTESIAN_POINT ( 'NONE',  ( -5.602943079677954685, 9.702389020015065313, -3.412202488244239884 ) ) ;
#23367 =( NAMED_UNIT ( * ) SI_UNIT ( $, .STERADIAN. ) SOLID_ANGLE_UNIT ( ) );
#23368 = ORIENTED_EDGE ( 'NONE', *, *, #2719, .T. ) ;
#23369 = CARTESIAN_POINT ( 'NONE',  ( 46.45294456288812057, 23.04411657098542676, 46.11470425768455783 ) ) ;
#23370 = CARTESIAN_POINT ( 'NONE',  ( -42.67844523361456766, 15.18734573188464765, 38.54111136810265492 ) ) ;
#23371 = CARTESIAN_POINT ( 'NONE',  ( -42.26497471389478733, 14.66834543456875117, 55.08207028713757580 ) ) ;
#23372 = CARTESIAN_POINT ( 'NONE',  ( -40.11027759654395197, 6.823245743731468416, 34.62590909864994870 ) ) ;
#23373 = CIRCLE ( 'NONE', #29132, 12.36707279061065279 ) ;
#23374 = CARTESIAN_POINT ( 'NONE',  ( -40.47630348341015605, 7.507564784836493033, 38.76982006947343251 ) ) ;
#23375 = ORIENTED_EDGE ( 'NONE', *, *, #31623, .F. ) ;
#23376 = CARTESIAN_POINT ( 'NONE',  ( -42.50976151518963064, 14.59907569580870046, 37.04930799450052348 ) ) ;
#23377 = DIRECTION ( 'NONE',  ( 0.000000000000000000, -0.000000000000000000, -1.000000000000000000 ) ) ;
#23378 = FACE_OUTER_BOUND ( 'NONE', #19032, .T. ) ;
#23379 = ORIENTED_EDGE ( 'NONE', *, *, #25498, .T. ) ;
#23380 = DIRECTION ( 'NONE',  ( -0.000000000000000000, 1.000000000000000000, -0.000000000000000000 ) ) ;
#23381 = DIRECTION ( 'NONE',  ( -0.000000000000000000, 1.000000000000000000, -0.000000000000000000 ) ) ;
#23382 = DIRECTION ( 'NONE',  ( -1.101824276508909887E-16, 1.000000000000000000, -0.000000000000000000 ) ) ;
#23383 = DIRECTION ( 'NONE',  ( -1.101824276508909887E-16, 1.000000000000000000, -0.000000000000000000 ) ) ;
#23384 = EDGE_LOOP ( 'NONE', ( #20771, #1732, #9174, #27638 ) ) ;
#23385 = CARTESIAN_POINT ( 'NONE',  ( 21.09992658989239089, 30.21664230456641675, 47.04930799450051637 ) ) ;
#23386 = ORIENTED_EDGE ( 'NONE', *, *, #303, .T. ) ;
#23387 = TOROIDAL_SURFACE ( 'NONE', #6095, 13.20178401536290913, 0.2000000000000002609 ) ;
#23388 = ORIENTED_EDGE ( 'NONE', *, *, #17675, .T. ) ;
#23389 = EDGE_CURVE ( 'NONE', #32160, #4198, #21439, .T. ) ;
#23390 = ADVANCED_FACE ( 'NONE', ( #13917 ), #16674, .T. ) ;
#23391 = EDGE_CURVE ( 'NONE', #31626, #6406, #22501, .T. ) ;
#23392 = ADVANCED_FACE ( 'NONE', ( #11611 ), #23914, .T. ) ;
#23393 = CIRCLE ( 'NONE', #26006, 12.62506659569710443 ) ;
#23394 = CARTESIAN_POINT ( 'NONE',  ( 48.23388202445966755, 27.52822092656774089, 49.27628909396054979 ) ) ;
#23395 = CARTESIAN_POINT ( 'NONE',  ( -36.43076496478325765, -5.790431667319170472, 78.73662387569818577 ) ) ;
#23396 = FACE_OUTER_BOUND ( 'NONE', #16442, .T. ) ;
#23397 = VERTEX_POINT ( 'NONE', #4379 ) ;
#23398 = CARTESIAN_POINT ( 'NONE',  ( -34.33782038214594223, 11.92558985988973497, 40.19271875144398365 ) ) ;
#23399 = VERTEX_POINT ( 'NONE', #21605 ) ;
#23400 = CARTESIAN_POINT ( 'NONE',  ( -7.324817582041172948, 8.310461108307681144, 106.8025418868326284 ) ) ;
#23401 = CARTESIAN_POINT ( 'NONE',  ( 21.09992658989239089, 24.21664230456639899, 47.04930799450051637 ) ) ;
#23402 = CARTESIAN_POINT ( 'NONE',  ( -31.01600359787390815, 11.71173593729433016, 69.58946823766353873 ) ) ;
#23403 = EDGE_CURVE ( 'NONE', #13392, #10357, #1252, .T. ) ;
#23404 = DIRECTION ( 'NONE',  ( 0.3935310072385435620, 0.5000000000000002220, 0.7714488617801035231 ) ) ;
#23405 = ORIENTED_EDGE ( 'NONE', *, *, #5116, .F. ) ;
#23406 = CARTESIAN_POINT ( 'NONE',  ( -40.15599670534037102, 7.478908884098773413, 38.19144330556764544 ) ) ;
#23407 = FACE_OUTER_BOUND ( 'NONE', #14495, .T. ) ;
#23408 = CARTESIAN_POINT ( 'NONE',  ( 21.09785597605719332, 24.86454579224780304, 67.04930799450050927 ) ) ;
#23410 = LINE ( 'NONE', #3701, #28965 ) ;
#23409 = VECTOR ( 'NONE', #11631, 1000.000000000000114 ) ;
#23411 = EDGE_LOOP ( 'NONE', ( #14232, #28941 ) ) ;
#23412 = DIRECTION ( 'NONE',  ( 0.000000000000000000, 0.000000000000000000, -1.000000000000000000 ) ) ;
#23413 = DIRECTION ( 'NONE',  ( 0.000000000000000000, -0.000000000000000000, -1.000000000000000000 ) ) ;
#23414 = CARTESIAN_POINT ( 'NONE',  ( -40.51045226066063520, 7.589116544599140646, 53.87859731638185679 ) ) ;
#23415 = CARTESIAN_POINT ( 'NONE',  ( 33.72499318558949710, 29.34143805560861296, 47.04930799450051637 ) ) ;
#23416 = CARTESIAN_POINT ( 'NONE',  ( 21.09785597605720753, 13.86454579224779948, 47.04930799450052348 ) ) ;
#23417 = ORIENTED_EDGE ( 'NONE', *, *, #31861, .T. ) ;
#23418 = CARTESIAN_POINT ( 'NONE',  ( 45.52675994804781112, 28.81155426599984892, 49.47108226228597516 ) ) ;
#23419 = CARTESIAN_POINT ( 'NONE',  ( -40.55615437192401629, 7.233232712783719265, 35.22901891019329668 ) ) ;
#23420 = ORIENTED_EDGE ( 'NONE', *, *, #31424, .T. ) ;
#23422 = EDGE_CURVE ( 'NONE', #20095, #12308, #25963, .T. ) ;
#23421 = CARTESIAN_POINT ( 'NONE',  ( 43.09785597605719687, 13.86454579224779948, 47.04930799450052348 ) ) ;
#23423 = EDGE_CURVE ( 'NONE', #4546, #9438, #25564, .T. ) ;
#23424 = CIRCLE ( 'NONE', #28666, 55.53141649511111666 ) ;
#23425 = DIRECTION ( 'NONE',  ( 0.000000000000000000, 0.000000000000000000, -1.000000000000000000 ) ) ;
#23426 = ORIENTED_EDGE ( 'NONE', *, *, #21962, .T. ) ;
#23427 = ORIENTED_EDGE ( 'NONE', *, *, #7757, .T. ) ;
#23428 = CARTESIAN_POINT ( 'NONE',  ( -12.43472240872365475, -3.866180060838604771, 103.2125413378014258 ) ) ;
#23429 = VERTEX_POINT ( 'NONE', #25055 ) ;
#23430 = EDGE_CURVE ( 'NONE', #29694, #6106, #2412, .T. ) ;
#23431 = AXIS2_PLACEMENT_3D ( 'NONE', #23376, #3180, #23216 ) ;
#23432 = ORIENTED_EDGE ( 'NONE', *, *, #8178, .F. ) ;
#23433 = CARTESIAN_POINT ( 'NONE',  ( 36.62540880027166423, 15.19538130838178169, 47.04930799450052348 ) ) ;
#23434 = CIRCLE ( 'NONE', #20518, 0.1999999999999987899 ) ;
#23435 = ORIENTED_EDGE ( 'NONE', *, *, #20480, .T. ) ;
#23436 = CARTESIAN_POINT ( 'NONE',  ( -40.47970302497625994, 7.463434137431151250, 60.44930799450051495 ) ) ;
#23437 = DIRECTION ( 'NONE',  ( 0.000000000000000000, -1.000000000000000000, 0.000000000000000000 ) ) ;
#23438 = DIRECTION ( 'NONE',  ( 0.4544104193609903586, 0.000000000000000000, 0.8907924397839087627 ) ) ;
#23439 = EDGE_CURVE ( 'NONE', #30111, #12384, #22750, .T. ) ;
#23440 = CARTESIAN_POINT ( 'NONE',  ( 45.81741271322955100, 27.80122849631042925, 49.02305402274571122 ) ) ;
#23441 = EDGE_LOOP ( 'NONE', ( #11251, #12088, #25545, #8953 ) ) ;
#23442 = ORIENTED_EDGE ( 'NONE', *, *, #4905, .T. ) ;
#23443 = CARTESIAN_POINT ( 'NONE',  ( -41.02113223168485234, 7.230835263863471418, 34.64930799450051779 ) ) ;
#23444 = ORIENTED_EDGE ( 'NONE', *, *, #18227, .F. ) ;
#23445 = ADVANCED_FACE ( 'NONE', ( #19793 ), #1024, .T. ) ;
#23446 = CARTESIAN_POINT ( 'NONE',  ( 42.05878518372482233, 11.91444431924556469, 99.69513167491371064 ) ) ;
#23447 = CARTESIAN_POINT ( 'NONE',  ( 54.52425928046186954, -0.6709275202869728894, 101.2046830443633354 ) ) ;
#23448 = AXIS2_PLACEMENT_3D ( 'NONE', #28416, #13640, #11334 ) ;
#23449 = CARTESIAN_POINT ( 'NONE',  ( 21.09785597605719332, 25.56454579224779877, 21.04930799450051282 ) ) ;
#23450 = TOROIDAL_SURFACE ( 'NONE', #17685, 12.40141737965280555, 0.1250000000000006939 ) ;
#23451 = CARTESIAN_POINT ( 'NONE',  ( 21.09992658989238734, 31.84164230456639544, 47.04930799450051637 ) ) ;
#23452 = CARTESIAN_POINT ( 'NONE',  ( -42.68334051588268352, -0.7182646751426445819, 62.04930799450052348 ) ) ;
#23453 = EDGE_LOOP ( 'NONE', ( #27688, #25377, #9269, #2839, #15956, #13188 ) ) ;
#23454 = LINE ( 'NONE', #25914, #31284 ) ;
#23456 = EDGE_CURVE ( 'NONE', #18307, #16525, #18310, .T. ) ;
#23455 = DIRECTION ( 'NONE',  ( 1.000000000000000000, -0.000000000000000000, -0.000000000000000000 ) ) ;
#23457 = CIRCLE ( 'NONE', #24503, 12.62506659569710266 ) ;
#23458 = FACE_OUTER_BOUND ( 'NONE', #20321, .T. ) ;
#23459 = EDGE_CURVE ( 'NONE', #3218, #17109, #28283, .T. ) ;
#23460 = CARTESIAN_POINT ( 'NONE',  ( 49.32483701613094240, 25.60322093266652743, 45.91328182968236860 ) ) ;
#23461 = CARTESIAN_POINT ( 'NONE',  ( 46.00908685603032922, 25.53284706826093498, 44.91496614357595263 ) ) ;
#23462 = TOROIDAL_SURFACE ( 'NONE', #5631, 12.40141737965288904, 0.1249999999999998612 ) ;
#23463 = VERTEX_POINT ( 'NONE', #12761 ) ;
#23464 = CARTESIAN_POINT ( 'NONE',  ( -42.50976151518963064, 14.59907569580870046, 36.00717268343339583 ) ) ;
#23465 = CARTESIAN_POINT ( 'NONE',  ( -40.59711871614117484, 7.548154485354792165, 53.86460186241264125 ) ) ;
#23466 = VECTOR ( 'NONE', #17819, 1000.000000000000000 ) ;
#23467 = VERTEX_POINT ( 'NONE', #268 ) ;
#23468 = EDGE_CURVE ( 'NONE', #3078, #2614, #10999, .T. ) ;
#23469 = ORIENTED_EDGE ( 'NONE', *, *, #10656, .T. ) ;
#23470 = CARTESIAN_POINT ( 'NONE',  ( 33.50134396954527460, 24.09164230456639544, 47.04930799450051637 ) ) ;
#23471 = VECTOR ( 'NONE', #16321, 999.9999999999998863 ) ;
#23472 = CARTESIAN_POINT ( 'NONE',  ( 21.09785597605719332, -16.93042895458276575, -37.45571725866892621 ) ) ;
#23473 = CARTESIAN_POINT ( 'NONE',  ( 21.09992658989239089, 24.09164230456639544, 47.04930799450051637 ) ) ;
#23474 = CIRCLE ( 'NONE', #17704, 0.1250000000000001110 ) ;
#23475 = ORIENTED_EDGE ( 'NONE', *, *, #4942, .T. ) ;
#23476 = CARTESIAN_POINT ( 'NONE',  ( 21.09992658989239089, 26.59164230456639899, 47.04930799450051637 ) ) ;
#23477 = VECTOR ( 'NONE', #27378, 1000.000000000000000 ) ;
#23478 = CARTESIAN_POINT ( 'NONE',  ( 81.60586963689938500, -5.935454207752203892, 16.07118271501079576 ) ) ;
#23479 = CARTESIAN_POINT ( 'NONE',  ( 21.09992658989238734, 38.56284415653841791, 47.04930799450051637 ) ) ;
#23480 = EDGE_CURVE ( 'NONE', #22795, #29858, #28791, .T. ) ;
#23481 = EDGE_LOOP ( 'NONE', ( #17985, #21680, #8256, #24443 ) ) ;
#23482 = CARTESIAN_POINT ( 'NONE',  ( 47.86511985000206693, 22.93807716476589320, 48.55339511290479493 ) ) ;
#23483 = ORIENTED_EDGE ( 'NONE', *, *, #16041, .T. ) ;
#23484 = ADVANCED_FACE ( 'NONE', ( #12596 ), #17332, .T. ) ;
#23485 = CARTESIAN_POINT ( 'NONE',  ( 21.09992658989239089, 30.59184655352422411, 47.04930799450051637 ) ) ;
#23486 = CARTESIAN_POINT ( 'NONE',  ( -40.88331355377635390, 6.750204415894309307, 34.54930799450052348 ) ) ;
#23487 = DIRECTION ( 'NONE',  ( -1.188208965918165239E-16, -1.880121038077813132E-16, -1.000000000000000000 ) ) ;
#23488 = FACE_OUTER_BOUND ( 'NONE', #20862, .T. ) ;
#23489 = CARTESIAN_POINT ( 'NONE',  ( -41.01929587258828036, 9.401204285752060130, 38.64930799450052490 ) ) ;
#23490 = ORIENTED_EDGE ( 'NONE', *, *, #24800, .T. ) ;
#23491 = ORIENTED_EDGE ( 'NONE', *, *, #22831, .T. ) ;
#23492 = FACE_OUTER_BOUND ( 'NONE', #16086, .T. ) ;
#23493 = DIRECTION ( 'NONE',  ( 0.000000000000000000, 0.000000000000000000, -1.000000000000000000 ) ) ;
#23494 = EDGE_CURVE ( 'NONE', #28828, #23854, #19879, .T. ) ;
#23495 = ADVANCED_FACE ( 'NONE', ( #15370 ), #32287, .F. ) ;
#23496 = CARTESIAN_POINT ( 'NONE',  ( 53.90149697474231516, 0.9814505390143266617, 99.57122575047146995 ) ) ;
#23497 = EDGE_LOOP ( 'NONE', ( #22977, #5408, #5894, #30487 ) ) ;
#23498 = CARTESIAN_POINT ( 'NONE',  ( 21.09785597605719332, 43.75535478762431296, 18.03093517794834000 ) ) ;
#23499 = CARTESIAN_POINT ( 'NONE',  ( -40.05987053574653345, 7.506472619680473635, 38.70582007960419446 ) ) ;
#23500 = EDGE_LOOP ( 'NONE', ( #4930, #21764, #20182, #19913 ) ) ;
#23501 = DIRECTION ( 'NONE',  ( 7.588956326749211550E-18, -4.206627182996912454E-18, 1.000000000000000000 ) ) ;
#23502 = CARTESIAN_POINT ( 'NONE',  ( 44.09250526802607340, 28.75621246473837189, 46.89322480343881949 ) ) ;
#23503 = AXIS2_PLACEMENT_3D ( 'NONE', #15684, #27960, #30263 ) ;
#23504 = AXIS2_PLACEMENT_3D ( 'NONE', #22987, #19431, #25137 ) ;
#23505 = FACE_OUTER_BOUND ( 'NONE', #10275, .T. ) ;
#23506 = AXIS2_PLACEMENT_3D ( 'NONE', #9569, #4315, #31886 ) ;
#23507 = AXIS2_PLACEMENT_3D ( 'NONE', #25557, #20950, #617 ) ;
#23508 = CIRCLE ( 'NONE', #27677, 12.27641737965284463 ) ;
#23509 = VERTEX_POINT ( 'NONE', #16165 ) ;
#23510 = CARTESIAN_POINT ( 'NONE',  ( 51.99726271649544884, -5.936960083300405699, -13.64809480703120137 ) ) ;
#23511 = FACE_OUTER_BOUND ( 'NONE', #25742, .T. ) ;
#23512 = ORIENTED_EDGE ( 'NONE', *, *, #18729, .F. ) ;
#23513 = DIRECTION ( 'NONE',  ( -0.8746197071393926326, 0.4848096202463430537, 8.676864087101709653E-18 ) ) ;
#23514 = DIRECTION ( 'NONE',  ( 0.000000000000000000, 0.000000000000000000, 1.000000000000000000 ) ) ;
#23515 = EDGE_CURVE ( 'NONE', #7622, #24404, #5747, .T. ) ;
#23516 = DIRECTION ( 'NONE',  ( -1.000000000000000000, -1.101824276508909887E-16, 0.000000000000000000 ) ) ;
#23517 = AXIS2_PLACEMENT_3D ( 'NONE', #5075, #30190, #12636 ) ;
#23518 = TOROIDAL_SURFACE ( 'NONE', #29311, 1.899999999999999467, 0.1000000000000000056 ) ;
#23519 = EDGE_LOOP ( 'NONE', ( #22000, #20259 ) ) ;
#23520 = CYLINDRICAL_SURFACE ( 'NONE', #23298, 12.36707279061065101 ) ;
#23521 = AXIS2_PLACEMENT_3D ( 'NONE', #2670, #17923, #13011 ) ;
#23522 = DIRECTION ( 'NONE',  ( -1.188208965918165239E-16, -1.880121038077813132E-16, -1.000000000000000000 ) ) ;
#23523 = CARTESIAN_POINT ( 'NONE',  ( 21.09992658989238734, 38.56284415653841791, 47.04930799450051637 ) ) ;
#23524 = FACE_OUTER_BOUND ( 'NONE', #28310, .T. ) ;
#23525 = SURFACE_STYLE_FILL_AREA ( #1516 ) ;
#23526 = VERTEX_POINT ( 'NONE', #3530 ) ;
#23527 = CARTESIAN_POINT ( 'NONE',  ( 46.04844006429464542, 22.80400562401889530, 44.99211097489548905 ) ) ;
#23528 = CARTESIAN_POINT ( 'NONE',  ( 21.09785597605719332, 13.74476430820393347, 47.04930799450051637 ) ) ;
#23529 = ADVANCED_FACE ( 'NONE', ( #28645 ), #18224, .F. ) ;
#23530 = TOROIDAL_SURFACE ( 'NONE', #2025, 12.61792373059898864, 0.1249999999999962669 ) ;
#23531 = LINE ( 'NONE', #12900, #11090 ) ;
#23532 = VERTEX_POINT ( 'NONE', #23075 ) ;
#23533 = CARTESIAN_POINT ( 'NONE',  ( 47.20987246576030572, 29.61033276412549142, 44.99785217098620649 ) ) ;
#23534 = DIRECTION ( 'NONE',  ( 0.000000000000000000, -1.000000000000000000, 0.000000000000000000 ) ) ;
#23535 = LINE ( 'NONE', #23218, #26926 ) ;
#23536 = VERTEX_POINT ( 'NONE', #25539 ) ;
#23537 = DIRECTION ( 'NONE',  ( -0.9612616959383221138, -0.2756373558169876170, 0.000000000000000000 ) ) ;
#23538 = CARTESIAN_POINT ( 'NONE',  ( 21.09785597605719687, 43.56454579224774193, 77.04930799450052348 ) ) ;
#23539 = CARTESIAN_POINT ( 'NONE',  ( -43.29662792673756400, 1.063067023446606196, 60.44930799450051495 ) ) ;
#23540 = DIRECTION ( 'NONE',  ( -1.000000000000000000, 0.000000000000000000, 0.000000000000000000 ) ) ;
#23541 = VERTEX_POINT ( 'NONE', #21086 ) ;
#23542 = CARTESIAN_POINT ( 'NONE',  ( -40.51522877113607279, 7.610537050327685904, 60.19811137623720754 ) ) ;
#23543 = VERTEX_POINT ( 'NONE', #5854 ) ;
#23544 = CIRCLE ( 'NONE', #27216, 12.62506659569710266 ) ;
#23545 = ORIENTED_EDGE ( 'NONE', *, *, #18120, .T. ) ;
#23546 =( BOUNDED_CURVE ( )  B_SPLINE_CURVE ( 2, ( #25100, #27724, #22789, #19837, #4579, #27228, #2289, #4917, #5242 ),
 .UNSPECIFIED., .F., .F. ) 
 B_SPLINE_CURVE_WITH_KNOTS ( ( 3, 2, 2, 2, 3 ),
 ( 0.6071428583041297289, 0.6190476190476190688, 0.6428571428571429047, 0.6666666666666666297, 0.6785714297327011257 ),
 .UNSPECIFIED. ) 
 CURVE ( )  GEOMETRIC_REPRESENTATION_ITEM ( )  RATIONAL_B_SPLINE_CURVE ( ( 0.9330127018922200755, 0.9330127084266224280, 1.000000000000000000, 0.8660254037844388186, 1.000000000000000000, 0.8660254037844388186, 1.000000000000000000, 0.9330126953578163906, 0.9330127018922200755 ) ) 
 REPRESENTATION_ITEM ( '' )  );
#23547 = PRODUCT_RELATED_PRODUCT_CATEGORY ( 'part', '', ( #7490 ) ) ;
#23548 = AXIS2_PLACEMENT_3D ( 'NONE', #28390, #7722, #15579 ) ;
#23549 = AXIS2_PLACEMENT_3D ( 'NONE', #1786, #17035, #21953 ) ;
#23550 = DIRECTION ( 'NONE',  ( 0.9612616959383205595, 0.2756373558169932236, -1.660411357259282445E-16 ) ) ;
#23551 = CARTESIAN_POINT ( 'NONE',  ( 49.19517401419062708, 26.88655426599985887, 48.40991706654173754 ) ) ;
#23552 = ORIENTED_EDGE ( 'NONE', *, *, #11315, .F. ) ;
#23553 = DIRECTION ( 'NONE',  ( -0.1949050434465268433, 0.6797146636928679264, 0.7071067811865469066 ) ) ;
#23554 = ORIENTED_EDGE ( 'NONE', *, *, #30815, .T. ) ;
#23555 = DIRECTION ( 'NONE',  ( -1.101824276508909887E-16, 1.000000000000000000, -0.000000000000000000 ) ) ;
#23556 = DIRECTION ( 'NONE',  ( -1.101824276508909887E-16, 1.000000000000000000, -0.000000000000000000 ) ) ;
#23557 = CARTESIAN_POINT ( 'NONE',  ( 33.72499318558949000, 38.56284415653841791, 47.04930799450051637 ) ) ;
#23558 = LINE ( 'NONE', #30644, #31512 ) ;
#23559 = ORIENTED_EDGE ( 'NONE', *, *, #13788, .T. ) ;
#23560 = FACE_OUTER_BOUND ( 'NONE', #11469, .T. ) ;
#23561 = ORIENTED_EDGE ( 'NONE', *, *, #7781, .T. ) ;
#23562 = CARTESIAN_POINT ( 'NONE',  ( -43.29088418437023478, 1.073429008971242382, 34.64930799450052490 ) ) ;
#23563 = CARTESIAN_POINT ( 'NONE',  ( 21.09785597605720753, 13.86454579224779948, 47.04930799450052348 ) ) ;
#23564 = CIRCLE ( 'NONE', #14153, 0.1250000000000001110 ) ;
#23565 = ORIENTED_EDGE ( 'NONE', *, *, #931, .T. ) ;
#23566 = DIRECTION ( 'NONE',  ( 0.8746197071393858602, -0.4848096202463547666, 0.000000000000000000 ) ) ;
#23568 = ADVANCED_FACE ( 'NONE', ( #3372 ), #20774, .T. ) ;
#23567 = CIRCLE ( 'NONE', #3630, 1.142135311067127512 ) ;
#23569 = DIRECTION ( 'NONE',  ( 0.000000000000000000, 1.000000000000000000, 1.446921688628131436E-16 ) ) ;
#23570 = DIRECTION ( 'NONE',  ( -1.101824276508909887E-16, 1.000000000000000000, -0.000000000000000000 ) ) ;
#23571 = ADVANCED_FACE ( 'NONE', ( #1075 ), #10452, .F. ) ;
#23572 = EDGE_CURVE ( 'NONE', #29304, #7835, #24593, .T. ) ;
#23573 = CARTESIAN_POINT ( 'NONE',  ( 45.24946171279598417, 25.62124452788248874, 47.99220971130007030 ) ) ;
#23574 = EDGE_CURVE ( 'NONE', #5630, #10357, #31034, .T. ) ;
#23575 = ORIENTED_EDGE ( 'NONE', *, *, #13179, .T. ) ;
#23576 = CARTESIAN_POINT ( 'NONE',  ( 21.09992658989239089, 25.47145308207319303, 47.04930799450051637 ) ) ;
#23577 = DIRECTION ( 'NONE',  ( -1.101824276508909887E-16, 1.000000000000000000, -0.000000000000000000 ) ) ;
#23578 = EDGE_CURVE ( 'NONE', #28996, #26728, #5230, .T. ) ;
#23579 = ORIENTED_EDGE ( 'NONE', *, *, #10165, .T. ) ;
#23580 = CARTESIAN_POINT ( 'NONE',  ( 47.94855545692534093, 23.24793988701932435, 46.58741075937935250 ) ) ;
#23581 = VECTOR ( 'NONE', #24999, 1000.000000000000227 ) ;
#23582 = CIRCLE ( 'NONE', #5237, 0.1250000000000001110 ) ;
#23583 = CARTESIAN_POINT ( 'NONE',  ( 21.09992658989239089, 28.59164230456639544, 47.04930799450051637 ) ) ;
#23584 = ORIENTED_EDGE ( 'NONE', *, *, #6710, .T. ) ;
#23585 = CIRCLE ( 'NONE', #8904, 1.500000000000001332 ) ;
#23586 = ORIENTED_EDGE ( 'NONE', *, *, #30909, .T. ) ;
#23587 = CARTESIAN_POINT ( 'NONE',  ( -40.05987053574653345, 7.506472619680472746, 38.70582007960419446 ) ) ;
#23588 = AXIS2_PLACEMENT_3D ( 'NONE', #14017, #8756, #24015 ) ;
#23589 = PRODUCT_DEFINITION_CONTEXT ( 'detailed design', #1945, 'design' ) ;
#23590 = ORIENTED_EDGE ( 'NONE', *, *, #27759, .T. ) ;
#23591 = TOROIDAL_SURFACE ( 'NONE', #7329, 12.40141737965285529, 0.1250000000000000555 ) ;
#23592 = EDGE_LOOP ( 'NONE', ( #12234, #32448, #2369, #1944 ) ) ;
#23593 = CARTESIAN_POINT ( 'NONE',  ( 80.77181806311266143, 9.702389020015065313, 20.34850893876557976 ) ) ;
#23594 = EDGE_CURVE ( 'NONE', #20651, #22795, #21955, .T. ) ;
#23595 = TOROIDAL_SURFACE ( 'NONE', #5267, 23.50000000000000000, 1.500000000000001332 ) ;
#23596 = EDGE_LOOP ( 'NONE', ( #214, #20065, #13085, #17402 ) ) ;
#23597 = CARTESIAN_POINT ( 'NONE',  ( 48.15269122424245296, 22.93328494799376216, 48.40553779021257697 ) ) ;
#23598 = AXIS2_PLACEMENT_3D ( 'NONE', #27077, #24781, #14293 ) ;
#23599 = FACE_OUTER_BOUND ( 'NONE', #15206, .T. ) ;
#23600 = DIRECTION ( 'NONE',  ( -1.101824276508909887E-16, 1.000000000000000000, -0.000000000000000000 ) ) ;
#23601 = CARTESIAN_POINT ( 'NONE',  ( 48.16694854572211426, 25.11789516297710279, 49.14507740233662503 ) ) ;
#23602 = AXIS2_PLACEMENT_3D ( 'NONE', #1833, #18892, #24314 ) ;
#23603 = VECTOR ( 'NONE', #7450, 1000.000000000000227 ) ;
#23604 = ORIENTED_EDGE ( 'NONE', *, *, #7458, .F. ) ;
#23605 = ORIENTED_EDGE ( 'NONE', *, *, #13398, .F. ) ;
#23606 = MECHANICAL_DESIGN_GEOMETRIC_PRESENTATION_REPRESENTATION (  '', ( #1066 ), #20473 ) ;
#23607 = EDGE_LOOP ( 'NONE', ( #31049, #835, #16365, #8882 ) ) ;
#23608 = CARTESIAN_POINT ( 'NONE',  ( -40.59768508530202524, 7.003142309055506054, 39.05686288009237472 ) ) ;
#23609 = CARTESIAN_POINT ( 'NONE',  ( -40.68642432603660808, 6.803331639906144090, 39.34088707671027407 ) ) ;
#23610 = DIRECTION ( 'NONE',  ( 0.5319835227803570987, 0.2110602665713105230, -0.8200287161831887328 ) ) ;
#23611 = EDGE_CURVE ( 'NONE', #30294, #3737, #14133, .T. ) ;
#23612 = EDGE_CURVE ( 'NONE', #32203, #22254, #20938, .T. ) ;
#23613 = DIRECTION ( 'NONE',  ( -0.000000000000000000, -1.000000000000000000, -0.000000000000000000 ) ) ;
#23614 = DIRECTION ( 'NONE',  ( -1.101824276508909887E-16, 1.000000000000000000, -0.000000000000000000 ) ) ;
#23615 = EDGE_CURVE ( 'NONE', #24681, #7753, #23242, .T. ) ;
#23616 = ORIENTED_EDGE ( 'NONE', *, *, #16733, .F. ) ;
#23617 = DIRECTION ( 'NONE',  ( -1.000000000000000000, 0.000000000000000000, 0.000000000000000000 ) ) ;
#23618 = CARTESIAN_POINT ( 'NONE',  ( -36.24635750042178728, -5.700102882051749198, 15.13141875408116022 ) ) ;
#23619 = VECTOR ( 'NONE', #11533, 1000.000000000000000 ) ;
#23620 = CARTESIAN_POINT ( 'NONE',  ( 21.09992658989239089, 29.34164230456639899, 47.04930799450051637 ) ) ;
#23621 = DIRECTION ( 'NONE',  ( 0.9612616959383221138, 0.2756373558169876170, 0.000000000000000000 ) ) ;
#23622 = PLANE ( 'NONE',  #21427 ) ;
#23623 = CYLINDRICAL_SURFACE ( 'NONE', #2513, 12.36707279061065101 ) ;
#23624 = ORIENTED_EDGE ( 'NONE', *, *, #18727, .F. ) ;
#23625 = CARTESIAN_POINT ( 'NONE',  ( -41.91739890389096956, 13.90674392281398930, 59.49868301348410426 ) ) ;
#23626 = DIRECTION ( 'NONE',  ( 0.9612616959383200044, 0.2756373558169954996, -1.660411357259285896E-16 ) ) ;
#23627 = TOROIDAL_SURFACE ( 'NONE', #3705, 12.61792373059859962, 0.1250000000000011380 ) ;
#23628 = ORIENTED_EDGE ( 'NONE', *, *, #28051, .T. ) ;
#23629 = TOROIDAL_SURFACE ( 'NONE', #9461, 17.50000000000000000, 1.499999999999998668 ) ;
#23630 = CIRCLE ( 'NONE', #3194, 0.1250000000000001110 ) ;
#23631 = AXIS2_PLACEMENT_3D ( 'NONE', #10756, #28304, #1047 ) ;
#23632 = EDGE_CURVE ( 'NONE', #26531, #22668, #8306, .T. ) ;
#23633 = VERTEX_POINT ( 'NONE', #11102 ) ;
#23634 = CARTESIAN_POINT ( 'NONE',  ( 48.15243707092404435, 22.93807716476589675, 45.72078620869762489 ) ) ;
#23635 = EDGE_CURVE ( 'NONE', #1229, #14267, #26167, .T. ) ;
#23636 = DIRECTION ( 'NONE',  ( -1.101824276508909887E-16, 1.000000000000000000, -0.000000000000000000 ) ) ;
#23637 = CARTESIAN_POINT ( 'NONE',  ( -35.12632216515691397, 11.92558985988973674, 54.04930799450053769 ) ) ;
#23638 = CIRCLE ( 'NONE', #17856, 0.1000000000000008243 ) ;
#23639 = ADVANCED_FACE ( 'NONE', ( #18778 ), #26663, .T. ) ;
#23640 = ORIENTED_EDGE ( 'NONE', *, *, #1016, .F. ) ;
#23641 = CARTESIAN_POINT ( 'NONE',  ( -23.27936906821728158, -13.30632128221581212, 81.09457859485948461 ) ) ;
#23642 = CARTESIAN_POINT ( 'NONE',  ( 49.09785597605720397, -5.098646251524523443, 47.04930799450052348 ) ) ;
#23643 = CARTESIAN_POINT ( 'NONE',  ( 21.09785597605720753, 14.46497581658974063, 47.04930799450052348 ) ) ;
#23644 = ORIENTED_EDGE ( 'NONE', *, *, #8418, .F. ) ;
#23645 = DIRECTION ( 'NONE',  ( -1.000000000000000000, -1.101824276508910010E-16, 0.000000000000000000 ) ) ;
#23646 = EDGE_LOOP ( 'NONE', ( #27503, #28113, #11820 ) ) ;
#23647 = LINE ( 'NONE', #9147, #24358 ) ;
#23648 = CARTESIAN_POINT ( 'NONE',  ( 21.09992658989239089, 30.22145308207317527, 47.04930799450051637 ) ) ;
#23649 = CARTESIAN_POINT ( 'NONE',  ( 46.99448882228015378, 29.20566913182630131, 44.58373285574925404 ) ) ;
#23650 = CIRCLE ( 'NONE', #7918, 45.93251711706293605 ) ;
#23651 = DIRECTION ( 'NONE',  ( -1.101824276508909887E-16, 1.000000000000000000, -0.000000000000000000 ) ) ;
#23652 = PRESENTATION_LAYER_ASSIGNMENT (  '', '', ( #23140 ) ) ;
#23653 = ADVANCED_FACE ( 'NONE', ( #4017 ), #19437, .F. ) ;
#23654 = EDGE_LOOP ( 'NONE', ( #20128, #26084, #25441, #2626 ) ) ;
#23655 = ORIENTED_EDGE ( 'NONE', *, *, #29021, .F. ) ;
#23656 = DIRECTION ( 'NONE',  ( -0.4848096202463424431, -0.8746197071393927436, 2.220446049250312588E-16 ) ) ;
#23657 = VECTOR ( 'NONE', #12443, 1000.000000000000000 ) ;
#23658 = LINE ( 'NONE', #8399, #31381 ) ;
#23659 = CARTESIAN_POINT ( 'NONE',  ( 33.46699938050303302, 38.56284415653841791, 47.04930799450051637 ) ) ;
#23660 = ORIENTED_EDGE ( 'NONE', *, *, #27050, .F. ) ;
#23661 = CARTESIAN_POINT ( 'NONE',  ( -36.18493864628602807, 8.798967949527998655, 53.54930799450051637 ) ) ;
#23662 = DIRECTION ( 'NONE',  ( 0.000000000000000000, 1.000000000000000000, 0.000000000000000000 ) ) ;
#23663 = ORIENTED_EDGE ( 'NONE', *, *, #27057, .T. ) ;
#23664 = CARTESIAN_POINT ( 'NONE',  ( -40.69571722278731585, 6.786566810383049209, 39.44930799450052206 ) ) ;
#23665 = CARTESIAN_POINT ( 'NONE',  ( 46.96268396749378127, 26.83121246473837473, 49.65201805493727960 ) ) ;
#23666 = TOROIDAL_SURFACE ( 'NONE', #27872, 12.40141737965283930, 0.1250000000000007216 ) ;
#23667 = DIRECTION ( 'NONE',  ( 0.05186525298099653458, 6.405245952009083202E-18, -0.9986540920324801229 ) ) ;
#23668 = EDGE_CURVE ( 'NONE', #3952, #12727, #32481, .T. ) ;
#23669 = EDGE_CURVE ( 'NONE', #3912, #14963, #5207, .T. ) ;
#23670 = EDGE_LOOP ( 'NONE', ( #18761, #19526, #22123, #4248 ) ) ;
#23671 = PRESENTATION_LAYER_ASSIGNMENT (  '', '', ( #25252 ) ) ;
#23672 = CIRCLE ( 'NONE', #24708, 22.50178251985260758 ) ;
#23673 = AXIS2_PLACEMENT_3D ( 'NONE', #9566, #7097, #17098 ) ;
#23674 = CARTESIAN_POINT ( 'NONE',  ( -36.45222641229887017, 9.925589859889724309, 52.04930799450051637 ) ) ;
#23675 = EDGE_CURVE ( 'NONE', #12822, #15058, #2061, .T. ) ;
#23676 = FACE_OUTER_BOUND ( 'NONE', #22799, .T. ) ;
#23677 = CARTESIAN_POINT ( 'NONE',  ( -43.64647580959332629, 1.256990871545142330, 53.64930799450051779 ) ) ;
#23678 = ADVANCED_FACE ( 'NONE', ( #4350 ), #19103, .T. ) ;
#23679 = ORIENTED_EDGE ( 'NONE', *, *, #10285, .T. ) ;
#23680 = CARTESIAN_POINT ( 'NONE',  ( 21.09992658989239089, 25.59164230456639899, 47.04930799450051637 ) ) ;
#23681 = FACE_OUTER_BOUND ( 'NONE', #25789, .T. ) ;
#23682 = CIRCLE ( 'NONE', #21043, 12.27641737965285174 ) ;
#23683 = DIRECTION ( 'NONE',  ( 0.000000000000000000, -0.000000000000000000, -1.000000000000000000 ) ) ;
#23684 = VERTEX_POINT ( 'NONE', #16640 ) ;
#23685 = FACE_OUTER_BOUND ( 'NONE', #12568, .T. ) ;
#23686 = CARTESIAN_POINT ( 'NONE',  ( 8.732853799281738105, 27.21183152705960495, 47.04930799450051637 ) ) ;
#23687 = DIRECTION ( 'NONE',  ( -1.101824276508909887E-16, 1.000000000000000000, -0.000000000000000000 ) ) ;
#23688 = EDGE_CURVE ( 'NONE', #28361, #3559, #18807, .T. ) ;
#23689 = ORIENTED_EDGE ( 'NONE', *, *, #24108, .T. ) ;
#23690 = LINE ( 'NONE', #3663, #12365 ) ;
#23691 = CARTESIAN_POINT ( 'NONE',  ( 47.20547626766765603, 26.78791119454915659, 44.97710074790751378 ) ) ;
#23692 = DIRECTION ( 'NONE',  ( -1.101824276508909887E-16, 1.000000000000000000, -0.000000000000000000 ) ) ;
#23693 = DIRECTION ( 'NONE',  ( -0.000000000000000000, -1.000000000000000000, -0.000000000000000000 ) ) ;
#23694 = CARTESIAN_POINT ( 'NONE',  ( 45.96182992765472619, 26.47822092656774728, 44.82232689504103007 ) ) ;
#23695 = VERTEX_POINT ( 'NONE', #1389 ) ;
#23696 = AXIS2_PLACEMENT_3D ( 'NONE', #26638, #4322, #23852 ) ;
#23697 = CARTESIAN_POINT ( 'NONE',  ( 47.15748190832469078, 29.60686683473450742, 44.99247469298313717 ) ) ;
#23698 = CARTESIAN_POINT ( 'NONE',  ( -41.56459318755936749, 7.281738416154046156, 60.44930799450051495 ) ) ;
#23699 = DIRECTION ( 'NONE',  ( 0.000000000000000000, 0.000000000000000000, -1.000000000000000000 ) ) ;
#23700 = ORIENTED_EDGE ( 'NONE', *, *, #14276, .T. ) ;
#23701 = DIRECTION ( 'NONE',  ( 0.8746197071393925215, -0.4848096202463429982, -8.676864087101708112E-18 ) ) ;
#23702 = DIRECTION ( 'NONE',  ( -1.000000000000000000, -1.101824276508909887E-16, 0.000000000000000000 ) ) ;
#23703 = DIRECTION ( 'NONE',  ( 0.000000000000000000, 0.000000000000000000, 1.000000000000000000 ) ) ;
#23704 = CARTESIAN_POINT ( 'NONE',  ( 54.75611978667879498, -3.386628651588837524, -8.728176170384978505 ) ) ;
#23705 = ORIENTED_EDGE ( 'NONE', *, *, #3551, .T. ) ;
#23706 = CARTESIAN_POINT ( 'NONE',  ( 48.10030433005226769, 29.45850404830353142, 49.01443330185325920 ) ) ;
#23707 = VERTEX_POINT ( 'NONE', #1549 ) ;
#23708 = ADVANCED_FACE ( 'NONE', ( #13881 ), #29859, .T. ) ;
#23709 = ADVANCED_FACE ( 'NONE', ( #6322 ), #11019, .F. ) ;
#23710 = ORIENTED_EDGE ( 'NONE', *, *, #23938, .T. ) ;
#23711 = VECTOR ( 'NONE', #22467, 1000.000000000000000 ) ;
#23712 = EDGE_CURVE ( 'NONE', #6391, #6454, #19385, .T. ) ;
#23713 = AXIS2_PLACEMENT_3D ( 'NONE', #23772, #28876, #15312 ) ;
#23714 = FACE_OUTER_BOUND ( 'NONE', #30115, .T. ) ;
#23715 = DIRECTION ( 'NONE',  ( -1.224646799147353207E-16, 0.000000000000000000, 1.000000000000000000 ) ) ;
#23716 = CARTESIAN_POINT ( 'NONE',  ( 21.09992658989239089, 25.97145308207318593, 47.04930799450051637 ) ) ;
#23717 = ORIENTED_EDGE ( 'NONE', *, *, #15128, .F. ) ;
#23718 = DIRECTION ( 'NONE',  ( -0.000000000000000000, -1.000000000000000000, 0.000000000000000000 ) ) ;
#23719 = EDGE_LOOP ( 'NONE', ( #26829, #27876, #6988, #719 ) ) ;
#23720 = DIRECTION ( 'NONE',  ( -1.101824276508909887E-16, 1.000000000000000000, -0.000000000000000000 ) ) ;
#23721 = CARTESIAN_POINT ( 'NONE',  ( -42.36691375901575185, 13.72999064396537250, 54.61480954800870791 ) ) ;
#23722 = CARTESIAN_POINT ( 'NONE',  ( 21.09785597605719332, -5.986312001189870280, -20.31486511684159879 ) ) ;
#23723 = EDGE_LOOP ( 'NONE', ( #9746, #21912, #30710, #13285 ) ) ;
#23724 = DIRECTION ( 'NONE',  ( -0.000000000000000000, -1.000000000000000000, -0.000000000000000000 ) ) ;
#23725 = DIRECTION ( 'NONE',  ( -1.000000000000000000, -1.101824276508909887E-16, 0.000000000000000000 ) ) ;
#23726 = DIRECTION ( 'NONE',  ( -0.9612616959383205595, -0.2756373558169931681, 1.660411357259282445E-16 ) ) ;
#23727 = DIRECTION ( 'NONE',  ( -1.101824276508909887E-16, 1.000000000000000000, -0.000000000000000000 ) ) ;
#23728 = ORIENTED_EDGE ( 'NONE', *, *, #8744, .T. ) ;
#23729 = CARTESIAN_POINT ( 'NONE',  ( 33.50134396954518934, 31.84164230456639544, 47.04930799450051637 ) ) ;
#23730 = DIRECTION ( 'NONE',  ( -1.101824276508909887E-16, 1.000000000000000000, -0.000000000000000000 ) ) ;
#23731 = DIRECTION ( 'NONE',  ( -1.224646799147353207E-16, -1.349345573449484691E-32, 1.000000000000000000 ) ) ;
#23732 = FACE_OUTER_BOUND ( 'NONE', #1480, .T. ) ;
#23733 = AXIS2_PLACEMENT_3D ( 'NONE', #3264, #31164, #28062 ) ;
#23734 = EDGE_LOOP ( 'NONE', ( #27025, #31974, #23435, #31801 ) ) ;
#23735 = CARTESIAN_POINT ( 'NONE',  ( 21.09785597605720042, -16.03545420775220265, 47.04930799450051637 ) ) ;
#23736 = CARTESIAN_POINT ( 'NONE',  ( -40.47576471041902124, 7.229986682739586890, 35.21321334501939049 ) ) ;
#23737 = EDGE_LOOP ( 'NONE', ( #12258, #16028, #26504, #8653 ) ) ;
#23738 = CARTESIAN_POINT ( 'NONE',  ( -43.62623615455565584, -4.423456490293570020, 42.00470062833824869 ) ) ;
#23739 = DIRECTION ( 'NONE',  ( -0.8746197071393927436, 0.4848096202463423876, 1.277302113040827440E-17 ) ) ;
#23740 = EDGE_LOOP ( 'NONE', ( #27168, #30290, #31890, #26001 ) ) ;
#23741 =( BOUNDED_CURVE ( )  B_SPLINE_CURVE ( 2, ( #5508, #26159, #31102, #18129, #30459, #17967, #15513 ),
 .UNSPECIFIED., .F., .F. ) 
 B_SPLINE_CURVE_WITH_KNOTS ( ( 3, 2, 2, 3 ),
 ( 0.7499999988387272554, 0.7619047619047618625, 0.7857142857142856984, 0.7981887600530632731 ),
 .UNSPECIFIED. ) 
 CURVE ( )  GEOMETRIC_REPRESENTATION_ITEM ( )  RATIONAL_B_SPLINE_CURVE ( ( 0.9330127018922199644, 0.9330126953578153914, 1.000000000000000000, 0.8660254037844387076, 1.000000000000000000, 0.9298069681733576175, 0.9331661149864407534 ) ) 
 REPRESENTATION_ITEM ( '' )  );
#23742 = EDGE_LOOP ( 'NONE', ( #5171, #6122, #17087, #26339 ) ) ;
#23743 = ORIENTED_EDGE ( 'NONE', *, *, #29615, .T. ) ;
#23744 = ADVANCED_FACE ( 'NONE', ( #19264 ), #25682, .T. ) ;
#23745 = ADVANCED_FACE ( 'NONE', ( #14207 ), #8388, .T. ) ;
#23746 = VECTOR ( 'NONE', #17674, 1000.000000000000000 ) ;
#23747 = ORIENTED_EDGE ( 'NONE', *, *, #2271, .F. ) ;
#23748 = TOROIDAL_SURFACE ( 'NONE', #4877, 38.50000000000000000, 0.9999999999999974465 ) ;
#23749 = DIRECTION ( 'NONE',  ( 0.000000000000000000, 1.000000000000000000, 0.000000000000000000 ) ) ;
#23750 = APPLICATION_CONTEXT ( 'automotive_design' ) ;
#23751 = EDGE_LOOP ( 'NONE', ( #1368, #30272, #7602, #27415 ) ) ;
#23752 = AXIS2_PLACEMENT_3D ( 'NONE', #5021, #27656, #2393 ) ;
#23753 = CARTESIAN_POINT ( 'NONE',  ( 47.87652597323660331, 22.99884124225578219, 48.23166275730290664 ) ) ;
#23754 = VECTOR ( 'NONE', #14745, 1000.000000000000000 ) ;
#23755 = CARTESIAN_POINT ( 'NONE',  ( 21.09785597605720753, 13.86454579224779948, 47.04930799450052348 ) ) ;
#23756 = DIRECTION ( 'NONE',  ( 0.000000000000000000, 0.000000000000000000, 1.000000000000000000 ) ) ;
#23757 = CARTESIAN_POINT ( 'NONE',  ( 46.99218062947583974, 27.90286309983298096, 49.08406571254116102 ) ) ;
#23758 = ORIENTED_EDGE ( 'NONE', *, *, #13279, .T. ) ;
#23759 = ORIENTED_EDGE ( 'NONE', *, *, #81, .F. ) ;
#23760 = ORIENTED_EDGE ( 'NONE', *, *, #10686, .F. ) ;
#23761 = DIRECTION ( 'NONE',  ( 0.000000000000000000, 1.000000000000000000, -0.000000000000000000 ) ) ;
#23762 = FACE_OUTER_BOUND ( 'NONE', #17939, .T. ) ;
#23763 = CARTESIAN_POINT ( 'NONE',  ( -43.64647580959332629, 1.256990871545142330, 53.54930799450051637 ) ) ;
#23764 = CARTESIAN_POINT ( 'NONE',  ( 8.482002859293412911, 25.71664230456640254, 47.04930799450051637 ) ) ;
#23765 = CARTESIAN_POINT ( 'NONE',  ( 21.09785597605720753, 14.86454579224779948, 47.04930799450052348 ) ) ;
#23766 = CARTESIAN_POINT ( 'NONE',  ( 100.3079064823960493, -15.93545420775219945, 47.04930799450134771 ) ) ;
#23767 = ITEM_DEFINED_TRANSFORMATION ( 'NONE', 'NONE', #25476,  #8172 ) ;
#23768 = VERTEX_POINT ( 'NONE', #18940 ) ;
#23769 = DIRECTION ( 'NONE',  ( -1.101824276508909887E-16, 1.000000000000000000, -0.000000000000000000 ) ) ;
#23770 = FACE_OUTER_BOUND ( 'NONE', #27678, .T. ) ;
#23771 = FACE_OUTER_BOUND ( 'NONE', #27919, .T. ) ;
#23772 = CARTESIAN_POINT ( 'NONE',  ( 21.09992658989239089, 30.09164230456639544, 47.04930799450051637 ) ) ;
#23773 = FACE_BOUND ( 'NONE', #5883, .T. ) ;
#23774 = AXIS2_PLACEMENT_3D ( 'NONE', #23677, #28598, #15637 ) ;
#23775 = ORIENTED_EDGE ( 'NONE', *, *, #31104, .F. ) ;
#23776 = CARTESIAN_POINT ( 'NONE',  ( 21.09785597605718266, 14.77310068074637961, 60.28471078280082907 ) ) ;
#23777 = ORIENTED_EDGE ( 'NONE', *, *, #6028, .T. ) ;
#23778 = DIRECTION ( 'NONE',  ( -1.000000000000000000, 0.000000000000000000, 0.000000000000000000 ) ) ;
#23779 = DIRECTION ( 'NONE',  ( -0.7141240004913198547, 0.3958453973320100738, 0.5773502691896283956 ) ) ;
#23780 = CIRCLE ( 'NONE', #31636, 2.500000000000002220 ) ;
#23781 = ORIENTED_EDGE ( 'NONE', *, *, #18045, .F. ) ;
#23782 = AXIS2_PLACEMENT_3D ( 'NONE', #5626, #23667, #20393 ) ;
#23783 = ADVANCED_FACE ( 'NONE', ( #28972 ), #6488, .T. ) ;
#23784 = EDGE_CURVE ( 'NONE', #28525, #2007, #24102, .T. ) ;
#23785 = EDGE_CURVE ( 'NONE', #11711, #20495, #5257, .T. ) ;
#23786 = EDGE_LOOP ( 'NONE', ( #2916, #14397, #24424, #2762 ) ) ;
#23787 = ADVANCED_FACE ( 'NONE', ( #32415 ), #1055, .T. ) ;
#23788 = CARTESIAN_POINT ( 'NONE',  ( -42.36153388572594736, 13.68895619636815653, 59.44930799450051495 ) ) ;
#23789 = CARTESIAN_POINT ( 'NONE',  ( -40.72710635398858869, 8.382218338248518918, 40.36793714460204541 ) ) ;
#23790 = DIRECTION ( 'NONE',  ( -0.000000000000000000, -1.000000000000000000, 0.000000000000000000 ) ) ;
#23791 = ORIENTED_EDGE ( 'NONE', *, *, #30850, .T. ) ;
#23792 = AXIS2_PLACEMENT_3D ( 'NONE', #18253, #10737, #13677 ) ;
#23793 = CARTESIAN_POINT ( 'NONE',  ( -63.90214402394282445, 9.925589859889724309, 52.04930799450051637 ) ) ;
#23794 = CARTESIAN_POINT ( 'NONE',  ( -35.27310491972505702, 11.80858882337094329, 40.73717082040712256 ) ) ;
#23795 = DIRECTION ( 'NONE',  ( -1.000000000000000000, 0.000000000000000000, 0.000000000000000000 ) ) ;
#23796 = ORIENTED_EDGE ( 'NONE', *, *, #5187, .T. ) ;
#23797 = DIRECTION ( 'NONE',  ( -0.8746197071393926326, 0.4848096202463430537, 8.676864087101709653E-18 ) ) ;
#23798 = VERTEX_POINT ( 'NONE', #75 ) ;
#23799 = DIRECTION ( 'NONE',  ( 0.000000000000000000, 0.000000000000000000, -1.000000000000000000 ) ) ;
#23800 = FACE_OUTER_BOUND ( 'NONE', #31119, .T. ) ;
#23801 = CARTESIAN_POINT ( 'NONE',  ( -42.21246928125516718, 14.65068104870687726, 37.04930799450052348 ) ) ;
#23802 = FILL_AREA_STYLE ('',( #15783 ) ) ;
#23803 = VERTEX_POINT ( 'NONE', #17788 ) ;
#23804 = ORIENTED_EDGE ( 'NONE', *, *, #31470, .F. ) ;
#23805 = CARTESIAN_POINT ( 'NONE',  ( -10.40214402394279425, 14.86454579224779948, 47.04930799450052348 ) ) ;
#23806 = FACE_OUTER_BOUND ( 'NONE', #18535, .T. ) ;
#23807 = CARTESIAN_POINT ( 'NONE',  ( -9.869916472764515447, -5.940946157296537855, 106.6954391641310309 ) ) ;
#23808 = EDGE_LOOP ( 'NONE', ( #31479, #23491, #12631, #27813 ) ) ;
#23809 = DIRECTION ( 'NONE',  ( -1.000000000000000000, -1.101824276508909887E-16, 0.000000000000000000 ) ) ;
#23810 = DIRECTION ( 'NONE',  ( -1.000000000000000000, -1.101824276508909887E-16, 0.000000000000000000 ) ) ;
#23811 = ORIENTED_EDGE ( 'NONE', *, *, #30183, .F. ) ;
#23812 = CARTESIAN_POINT ( 'NONE',  ( 21.09992658989239089, 29.59164230456639899, 47.04930799450051637 ) ) ;
#23813 = CARTESIAN_POINT ( 'NONE',  ( 46.96268396749378127, 28.23121246473836976, 49.65201805493727960 ) ) ;
#23814 = EDGE_CURVE ( 'NONE', #25906, #231, #23564, .T. ) ;
#23815 = ADVANCED_FACE ( 'NONE', ( #27485 ), #23591, .T. ) ;
#23816 = DIRECTION ( 'NONE',  ( -1.101824276508909887E-16, 1.000000000000000000, -0.000000000000000000 ) ) ;
#23817 = CIRCLE ( 'NONE', #13868, 1.199999999999999734 ) ;
#23818 = CIRCLE ( 'NONE', #13870, 2.000000000000001776 ) ;
#23819 = CIRCLE ( 'NONE', #11764, 0.3000000000000017653 ) ;
#23820 = AXIS2_PLACEMENT_3D ( 'NONE', #1761, #6855, #4230 ) ;
#23821 = TOROIDAL_SURFACE ( 'NONE', #8121, 70.59901951359279337, 0.6000000000000020872 ) ;
#23822 = AXIS2_PLACEMENT_3D ( 'NONE', #24642, #4459, #4295 ) ;
#23823 = ORIENTED_EDGE ( 'NONE', *, *, #20448, .F. ) ;
#23824 = CARTESIAN_POINT ( 'NONE',  ( 106.0978559760574313, 11.92558985988973497, 67.46350265493050813 ) ) ;
#23825 = EDGE_CURVE ( 'NONE', #26196, #12159, #22534, .T. ) ;
#23826 = CARTESIAN_POINT ( 'NONE',  ( 21.09992658989239089, 28.84164230456639544, 47.04930799450051637 ) ) ;
#23827 = CARTESIAN_POINT ( 'NONE',  ( 48.83059987400639557, 28.38213139976339860, 48.97189179988551899 ) ) ;
#23828 = CARTESIAN_POINT ( 'NONE',  ( 44.70507715278255745, 29.14951373492759146, 46.92503878583764987 ) ) ;
#23829 = ORIENTED_EDGE ( 'NONE', *, *, #5126, .F. ) ;
#23830 = DIRECTION ( 'NONE',  ( 0.000000000000000000, 1.000000000000000000, -0.000000000000000000 ) ) ;
#23831 = DIRECTION ( 'NONE',  ( 0.000000000000000000, -1.000000000000000000, 0.000000000000000000 ) ) ;
#23832 = CARTESIAN_POINT ( 'NONE',  ( 66.59450633559774246, 13.78276522714992147, 47.04930799450051637 ) ) ;
#23833 = ORIENTED_EDGE ( 'NONE', *, *, #30721, .F. ) ;
#23834 = DIRECTION ( 'NONE',  ( -1.000000000000000000, -1.101824276508909887E-16, 0.000000000000000000 ) ) ;
#23835 = DIRECTION ( 'NONE',  ( -0.4848096202463427762, -0.8746197071393926326, 0.000000000000000000 ) ) ;
#23836 = CARTESIAN_POINT ( 'NONE',  ( -40.40505316653322865, 8.317079188576510518, 59.54930799450052348 ) ) ;
#23837 = AXIS2_PLACEMENT_3D ( 'NONE', #22943, #23282, #793 ) ;
#23838 = EDGE_CURVE ( 'NONE', #25211, #25249, #22383, .T. ) ;
#23839 = VECTOR ( 'NONE', #2334, 1000.000000000000000 ) ;
#23840 = ORIENTED_EDGE ( 'NONE', *, *, #8021, .F. ) ;
#23841 = PLANE ( 'NONE',  #16030 ) ;
#23842 = CARTESIAN_POINT ( 'NONE',  ( 46.99023568444673060, 28.53791119454914949, 49.12151524109405898 ) ) ;
#23843 = TOROIDAL_SURFACE ( 'NONE', #9709, 13.48414152717812797, 1.000000000001010525 ) ;
#23844 = VECTOR ( 'NONE', #4023, 1000.000000000000000 ) ;
#23845 = CYLINDRICAL_SURFACE ( 'NONE', #5162, 12.62506659569710266 ) ;
#23846 = EDGE_CURVE ( 'NONE', #31307, #23684, #9446, .T. ) ;
#23847 = CARTESIAN_POINT ( 'NONE',  ( 21.09785597605720753, -13.37218737171702543, -8.638398481670979123 ) ) ;
#23848 = VECTOR ( 'NONE', #32161, 1000.000000000000000 ) ;
#23849 = DIRECTION ( 'NONE',  ( -1.000000000000000000, 0.000000000000000000, 0.000000000000000000 ) ) ;
#23850 = EDGE_LOOP ( 'NONE', ( #8674, #32130, #29657, #14407 ) ) ;
#23851 = CARTESIAN_POINT ( 'NONE',  ( 47.41914917073021485, 29.61434127664690763, 45.02321843626506137 ) ) ;
#23852 = DIRECTION ( 'NONE',  ( 0.000000000000000000, 0.000000000000000000, 1.000000000000000000 ) ) ;
#23853 = DIRECTION ( 'NONE',  ( -1.101824276508909887E-16, 1.000000000000000000, -0.000000000000000000 ) ) ;
#23854 = VERTEX_POINT ( 'NONE', #7634 ) ;
#23855 = CARTESIAN_POINT ( 'NONE',  ( -43.38408989745150990, 1.111547985471240008, 53.54930799450051637 ) ) ;
#23856 = FACE_OUTER_BOUND ( 'NONE', #23441, .T. ) ;
#23857 = EDGE_CURVE ( 'NONE', #29931, #9420, #15720, .T. ) ;
#23858 = EDGE_CURVE ( 'NONE', #9599, #11721, #8034, .T. ) ;
#23859 = DIRECTION ( 'NONE',  ( 1.000000000000000000, 0.000000000000000000, 0.000000000000000000 ) ) ;
#23860 = CARTESIAN_POINT ( 'NONE',  ( 21.09785597605720042, -13.98292989133646103, 47.04930799450051637 ) ) ;
#23861 = EDGE_CURVE ( 'NONE', #25724, #26085, #9423, .T. ) ;
#23862 = VERTEX_POINT ( 'NONE', #5165 ) ;
#23863 = CARTESIAN_POINT ( 'NONE',  ( -41.01929587258828747, 9.401204285752060130, 39.44930799450052206 ) ) ;
#23864 = ORIENTED_EDGE ( 'NONE', *, *, #27068, .T. ) ;
#23865 = ORIENTED_EDGE ( 'NONE', *, *, #32030, .F. ) ;
#23866 = VECTOR ( 'NONE', #7547, 1000.000000000000000 ) ;
#23867 = AXIS2_PLACEMENT_3D ( 'NONE', #21324, #19027, #26430 ) ;
#23868 = EDGE_CURVE ( 'NONE', #18864, #19298, #26733, .T. ) ;
#23869 = AXIS2_PLACEMENT_3D ( 'NONE', #21207, #26146, #21052 ) ;
#23870 = VECTOR ( 'NONE', #5490, 1000.000000000000000 ) ;
#23871 = AXIS2_PLACEMENT_3D ( 'NONE', #12394, #5160, #22381 ) ;
#23872 = LINE ( 'NONE', #1382, #14500 ) ;
#23873 = DIRECTION ( 'NONE',  ( 0.4848096202463636484, 0.8746197071393810862, 0.000000000000000000 ) ) ;
#23874 = DIRECTION ( 'NONE',  ( -1.101824276508909887E-16, 1.000000000000000000, -0.000000000000000000 ) ) ;
#23875 = CIRCLE ( 'NONE', #8689, 0.1249999999999931721 ) ;
#23876 = ORIENTED_EDGE ( 'NONE', *, *, #22746, .F. ) ;
#23877 = DIRECTION ( 'NONE',  ( -0.000000000000000000, -1.000000000000000000, 0.000000000000000000 ) ) ;
#23878 = ORIENTED_EDGE ( 'NONE', *, *, #8535, .F. ) ;
#23879 = DIRECTION ( 'NONE',  ( -1.101824276508909887E-16, 1.000000000000000000, -0.000000000000000000 ) ) ;
#23880 = DIRECTION ( 'NONE',  ( 0.000000000000000000, 0.000000000000000000, -1.000000000000000000 ) ) ;
#23881 = EDGE_CURVE ( 'NONE', #8349, #802, #9955, .T. ) ;
#23882 = FILL_AREA_STYLE_COLOUR ( '', #15782 ) ;
#23883 = ORIENTED_EDGE ( 'NONE', *, *, #14234, .F. ) ;
#23884 = LINE ( 'NONE', #8477, #29102 ) ;
#23885 = CARTESIAN_POINT ( 'NONE',  ( 21.09992658989238734, 38.56284415653841791, 47.04930799450051637 ) ) ;
#23886 = CARTESIAN_POINT ( 'NONE',  ( 21.09785597605719332, 6.671061906060458568, 47.04930799450051637 ) ) ;
#23887 = CARTESIAN_POINT ( 'NONE',  ( 45.45032030167665482, 22.91413368675619111, 46.31675765204602868 ) ) ;
#23888 = ORIENTED_EDGE ( 'NONE', *, *, #12216, .T. ) ;
#23889 = CARTESIAN_POINT ( 'NONE',  ( 21.09785597605719332, -6.314304012688826795, 47.04930799450051637 ) ) ;
#23890 = EDGE_CURVE ( 'NONE', #6391, #5554, #2699, .T. ) ;
#23891 = CARTESIAN_POINT ( 'NONE',  ( -40.73091736380679606, 9.483895492497156354, 35.44930799450052206 ) ) ;
#23892 = CARTESIAN_POINT ( 'NONE',  ( 21.09785597605719332, 34.59164230456639899, 47.04930799450051637 ) ) ;
#23893 = CARTESIAN_POINT ( 'NONE',  ( -43.90780810587784089, -0.03953120679776531143, 47.04930799450051637 ) ) ;
#23894 = CARTESIAN_POINT ( 'NONE',  ( 21.09785597605719332, 14.77459629858661572, 47.04930799450051637 ) ) ;
#23895 = ORIENTED_EDGE ( 'NONE', *, *, #5049, .F. ) ;
#23896 = DIRECTION ( 'NONE',  ( 0.000000000000000000, 0.000000000000000000, 1.000000000000000000 ) ) ;
#23897 = CARTESIAN_POINT ( 'NONE',  ( 47.09785597605719687, 15.77906836436399374, 47.04930799450078638 ) ) ;
#23898 = EDGE_LOOP ( 'NONE', ( #11598, #21537, #16164, #336 ) ) ;
#23899 = LINE ( 'NONE', #13575, #26640 ) ;
#23900 = CIRCLE ( 'NONE', #15007, 0.1250000000000001110 ) ;
#23901 = AXIS2_PLACEMENT_3D ( 'NONE', #3494, #21050, #19566 ) ;
#23902 = EDGE_CURVE ( 'NONE', #24243, #29052, #25169, .T. ) ;
#23903 = CARTESIAN_POINT ( 'NONE',  ( 21.09992658989239089, 25.59164230456639899, 47.04930799450051637 ) ) ;
#23904 = ADVANCED_FACE ( 'NONE', ( #20248 ), #20427, .T. ) ;
#23905 = ORIENTED_EDGE ( 'NONE', *, *, #24033, .T. ) ;
#23906 = VERTEX_POINT ( 'NONE', #24525 ) ;
#23907 = UNCERTAINTY_MEASURE_WITH_UNIT (LENGTH_MEASURE( 1.000000000000000082E-05 ), #18947, 'distance_accuracy_value', 'NONE');
#23908 = CIRCLE ( 'NONE', #13959, 13.81487396812510937 ) ;
#23909 = ORIENTED_EDGE ( 'NONE', *, *, #14382, .F. ) ;
#23910 = FACE_OUTER_BOUND ( 'NONE', #14786, .T. ) ;
#23911 = CIRCLE ( 'NONE', #14515, 0.1250000000000001110 ) ;
#23912 = EDGE_LOOP ( 'NONE', ( #1254, #29142, #1355, #13850 ) ) ;
#23913 = DIRECTION ( 'NONE',  ( 0.2756373558169954996, -0.9612616959383200044, 2.463803012461673974E-31 ) ) ;
#23914 = SPHERICAL_SURFACE ( 'NONE', #30908, 0.1000000000000000056 ) ;
#23915 = FACE_OUTER_BOUND ( 'NONE', #15047, .T. ) ;
#23916 = CARTESIAN_POINT ( 'NONE',  ( -42.21195563036361875, 4.051200314738730768, 37.04930799450052348 ) ) ;
#23917 = CARTESIAN_POINT ( 'NONE',  ( 48.80717017713595141, 26.61952976649964953, 48.15820438821415195 ) ) ;
#23918 = VERTEX_POINT ( 'NONE', #2045 ) ;
#23919 = ORIENTED_EDGE ( 'NONE', *, *, #7272, .F. ) ;
#23920 = CARTESIAN_POINT ( 'NONE',  ( -11.87053376181319386, 0.6013300790671924911, -5.618057101110695228 ) ) ;
#23921 = ORIENTED_EDGE ( 'NONE', *, *, #21884, .T. ) ;
#23922 = CARTESIAN_POINT ( 'NONE',  ( 33.71785032049132980, 29.46664230456640254, 47.04930799450051637 ) ) ;
#23923 = CIRCLE ( 'NONE', #21291, 0.1000000000000028644 ) ;
#23924 = CARTESIAN_POINT ( 'NONE',  ( -40.54123211584759190, 7.002658380791086046, 39.07840589319199864 ) ) ;
#23925 = CARTESIAN_POINT ( 'NONE',  ( -40.69503817910556620, 6.787791837612842549, 39.43724091009085697 ) ) ;
#23926 = CARTESIAN_POINT ( 'NONE',  ( -40.86580004447909431, 8.503105189880381332, 39.44930799450052206 ) ) ;
#23927 = CARTESIAN_POINT ( 'NONE',  ( 46.96268396749378127, 26.13121246473837544, 49.65201805493727960 ) ) ;
#23928 = DIRECTION ( 'NONE',  ( 0.8746197071393926326, -0.4848096202463430537, -8.676864087101709653E-18 ) ) ;
#23929 = CARTESIAN_POINT ( 'NONE',  ( -41.24971778908466291, 11.62557032131817358, 58.05249952744806308 ) ) ;
#23930 = ORIENTED_EDGE ( 'NONE', *, *, #7415, .F. ) ;
#23931 = DIRECTION ( 'NONE',  ( 0.1949050434465247617, -0.6797146636928672603, -0.7071067811865480168 ) ) ;
#23932 = FACE_OUTER_BOUND ( 'NONE', #24138, .T. ) ;
#23933 = DIRECTION ( 'NONE',  ( 0.000000000000000000, 0.000000000000000000, 1.000000000000000000 ) ) ;
#23934 = ADVANCED_FACE ( 'NONE', ( #29628 ), #19911, .T. ) ;
#23935 = DIRECTION ( 'NONE',  ( 0.8746197071393926326, -0.4848096202463430537, -8.676864087101709653E-18 ) ) ;
#23936 = EDGE_CURVE ( 'NONE', #15830, #7227, #4840, .T. ) ;
#23937 = CARTESIAN_POINT ( 'NONE',  ( 8.732853799281738105, 26.21183152705960140, 47.04930799450051637 ) ) ;
#23938 = EDGE_CURVE ( 'NONE', #18375, #20946, #31950, .T. ) ;
#23939 = ORIENTED_EDGE ( 'NONE', *, *, #25011, .T. ) ;
#23940 = CARTESIAN_POINT ( 'NONE',  ( 8.474859994195286461, 26.34184655352419213, 47.04930799450051637 ) ) ;
#23941 = EDGE_LOOP ( 'NONE', ( #23624, #15918, #31012, #30517 ) ) ;
#23942 = DIRECTION ( 'NONE',  ( 0.5442436726714897643, 6.721291001053910056E-17, -0.8389271868029121171 ) ) ;
#23943 = CARTESIAN_POINT ( 'NONE',  ( 100.3079064823960493, 25.56454579224780232, 44.54930799450134771 ) ) ;
#23944 = AXIS2_PLACEMENT_3D ( 'NONE', #7187, #21946, #19812 ) ;
#23945 = ORIENTED_EDGE ( 'NONE', *, *, #31531, .T. ) ;
#23946 = VERTEX_POINT ( 'NONE', #30603 ) ;
#23947 = DIRECTION ( 'NONE',  ( -1.000000000000000000, 0.000000000000000000, -1.926892052941620175E-16 ) ) ;
#23948 = CARTESIAN_POINT ( 'NONE',  ( 21.09992658989238734, 32.21183152705962272, 47.04930799450051637 ) ) ;
#23949 = CARTESIAN_POINT ( 'NONE',  ( -40.78148461367150901, 8.178669543025179678, 59.57859731638185963 ) ) ;
#23950 = ORIENTED_EDGE ( 'NONE', *, *, #17621, .F. ) ;
#23951 = LINE ( 'NONE', #21482, #17202 ) ;
#23952 = CARTESIAN_POINT ( 'NONE',  ( 21.09992658989239089, 30.22145308207317527, 47.04930799450051637 ) ) ;
#23953 = CARTESIAN_POINT ( 'NONE',  ( 77.22212800161737789, -3.812314126620147459, 13.51013469878526152 ) ) ;
#23954 = CIRCLE ( 'NONE', #9828, 54.21005050633881694 ) ;
#23955 = EDGE_LOOP ( 'NONE', ( #30989, #19460, #32310, #2974, #3501 ) ) ;
#23956 = CARTESIAN_POINT ( 'NONE',  ( -40.09211399732166115, 9.667069410243957606, 35.44930799450052206 ) ) ;
#23957 = VERTEX_POINT ( 'NONE', #18426 ) ;
#23958 = CARTESIAN_POINT ( 'NONE',  ( -42.46007270772396680, 14.70100007970371792, 58.95278695508191191 ) ) ;
#23959 = CARTESIAN_POINT ( 'NONE',  ( 49.19517401419062708, 29.10920399681022630, 48.40991706654173754 ) ) ;
#23960 = TOROIDAL_SURFACE ( 'NONE', #15079, 12.61792373059899397, 0.1249999999999959616 ) ;
#23961 = DIRECTION ( 'NONE',  ( 0.4848096202463645921, 0.8746197071393805311, 0.000000000000000000 ) ) ;
#23962 = SHAPE_REPRESENTATION_RELATIONSHIP ( 'NONE' , 'NONE' ,  #5723, #30825 ) ;
#23963 = ORIENTED_EDGE ( 'NONE', *, *, #21959, .F. ) ;
#23964 = ORIENTED_EDGE ( 'NONE', *, *, #10572, .F. ) ;
#23965 = CARTESIAN_POINT ( 'NONE',  ( 45.83138912416442423, -13.30632128221581212, -3.117123918615745115 ) ) ;
#23966 = CYLINDRICAL_SURFACE ( 'NONE', #5705, 12.62506659569710266 ) ;
#23967 = ADVANCED_FACE ( 'NONE', ( #18262 ), #873, .T. ) ;
#23968 = EDGE_CURVE ( 'NONE', #28177, #26439, #2628, .T. ) ;
#23969 = DIRECTION ( 'NONE',  ( -1.101824276508909887E-16, 1.000000000000000000, -0.000000000000000000 ) ) ;
#23970 = EDGE_CURVE ( 'NONE', #31321, #18652, #15497, .T. ) ;
#23971 = EDGE_CURVE ( 'NONE', #27727, #18298, #6817, .T. ) ;
#23972 = ORIENTED_EDGE ( 'NONE', *, *, #23675, .F. ) ;
#23973 = CARTESIAN_POINT ( 'NONE',  ( 21.09785597605719332, -16.63545420775219696, 47.04930799450051637 ) ) ;
#23974 = DIRECTION ( 'NONE',  ( -1.101824276508909887E-16, 1.000000000000000000, -0.000000000000000000 ) ) ;
#23975 = EDGE_CURVE ( 'NONE', #9470, #4922, #17806, .T. ) ;
#23976 = VERTEX_POINT ( 'NONE', #8590 ) ;
#23977 = EDGE_CURVE ( 'NONE', #15887, #11490, #31081, .T. ) ;
#23978 = CARTESIAN_POINT ( 'NONE',  ( 48.73570333863616355, 29.22287913140504045, 44.52463952959527660 ) ) ;
#23979 = CARTESIAN_POINT ( 'NONE',  ( 21.09992658989238734, 38.56284415653841791, 47.04930799450051637 ) ) ;
#23980 = CIRCLE ( 'NONE', #13524, 12.62506659569710443 ) ;
#23981 = AXIS2_PLACEMENT_3D ( 'NONE', #1281, #18196, #28227 ) ;
#23982 = ORIENTED_EDGE ( 'NONE', *, *, #11257, .T. ) ;
#23983 = CIRCLE ( 'NONE', #25049, 0.1000000000000014905 ) ;
#23984 = CYLINDRICAL_SURFACE ( 'NONE', #3856, 12.36707279061065101 ) ;
#23985 = CARTESIAN_POINT ( 'NONE',  ( 21.09785597605720753, 13.86454579224779948, 47.04930799450052348 ) ) ;
#23986 = CARTESIAN_POINT ( 'NONE',  ( -40.59298576501942790, 7.024321269945727586, 35.15525576937660190 ) ) ;
#23987 = CARTESIAN_POINT ( 'NONE',  ( 45.24946171279598417, 29.90784706826092076, 47.99220971130007030 ) ) ;
#23988 = AXIS2_PLACEMENT_3D ( 'NONE', #69, #2373, #27806 ) ;
#23989 = VERTEX_POINT ( 'NONE', #25507 ) ;
#23990 = CARTESIAN_POINT ( 'NONE',  ( 33.46699938050304013, 23.96183152705959785, 47.04930799450051637 ) ) ;
#23991 = DIRECTION ( 'NONE',  ( -0.8746197071393925215, 0.4848096202463429982, 8.676864087101708112E-18 ) ) ;
#23992 = ADVANCED_FACE ( 'NONE', ( #13520 ), #23033, .T. ) ;
#23993 = B_SPLINE_CURVE_WITH_KNOTS ( 'NONE', 3,
 ( #19036, #23807, #16578, #4282, #16261, #4108, #1009, #3632 ),
 .UNSPECIFIED., .F., .F.,
 ( 4, 2, 2, 4 ),
 ( 6.938893903907228378E-18, 0.0004427811193176627936, 0.0008855622386353186482, 0.001771124477270593061 ),
 .UNSPECIFIED. ) ;
#23994 = DIRECTION ( 'NONE',  ( -1.101824276508909887E-16, 1.000000000000000000, -0.000000000000000000 ) ) ;
#23995 = FACE_OUTER_BOUND ( 'NONE', #29671, .T. ) ;
#23996 = DIRECTION ( 'NONE',  ( -1.000000000000000000, 0.000000000000000000, 0.000000000000000000 ) ) ;
#23997 = DIRECTION ( 'NONE',  ( 0.9612616959383207815, 0.2756373558169926685, 8.795445018804289444E-19 ) ) ;
#23998 = DIRECTION ( 'NONE',  ( -1.000000000000000000, 0.000000000000000000, 0.000000000000000000 ) ) ;
#23999 = SURFACE_SIDE_STYLE ('',( #23525 ) ) ;
#24000 = ORIENTED_EDGE ( 'NONE', *, *, #11266, .T. ) ;
#24001 = CARTESIAN_POINT ( 'NONE',  ( 45.61530479625130852, 22.89977464660286444, 45.91938710987583505 ) ) ;
#24003 = CARTESIAN_POINT ( 'NONE',  ( 49.49063479933183629, 28.71291119454914664, 47.17357720316391578 ) ) ;
#24002 = AXIS2_PLACEMENT_3D ( 'NONE', #10684, #2946, #12977 ) ;
#24004 = DIRECTION ( 'NONE',  ( -1.101824276508909887E-16, 1.000000000000000000, -0.000000000000000000 ) ) ;
#24005 = CARTESIAN_POINT ( 'NONE',  ( -40.11729073372970333, 6.802967823440400075, 34.64930799450051779 ) ) ;
#24006 = AXIS2_PLACEMENT_3D ( 'NONE', #4806, #25317, #48 ) ;
#24007 = DIRECTION ( 'NONE',  ( -1.101824276508909887E-16, 1.000000000000000000, -0.000000000000000000 ) ) ;
#24008 = EDGE_CURVE ( 'NONE', #5510, #20520, #21983, .T. ) ;
#24009 = EDGE_LOOP ( 'NONE', ( #6971, #30255, #21945, #3232 ) ) ;
#24010 = CARTESIAN_POINT ( 'NONE',  ( -39.57300472050416573, -5.936086065851251092, 77.91551484630795699 ) ) ;
#24011 = DIRECTION ( 'NONE',  ( -2.779292025043186357E-18, 1.288349127009862211E-17, -1.000000000000000000 ) ) ;
#24012 = DIRECTION ( 'NONE',  ( -1.000000000000000000, 0.000000000000000000, 0.000000000000000000 ) ) ;
#24013 = VECTOR ( 'NONE', #3550, 1000.000000000000000 ) ;
#24014 = ORIENTED_EDGE ( 'NONE', *, *, #23271, .F. ) ;
#24015 = DIRECTION ( 'NONE',  ( -1.000000000000000000, -1.101824276508910010E-16, 0.000000000000000000 ) ) ;
#24016 = EDGE_CURVE ( 'NONE', #11676, #13013, #3124, .T. ) ;
#24017 = FACE_OUTER_BOUND ( 'NONE', #25113, .T. ) ;
#24018 = DIRECTION ( 'NONE',  ( -1.000000000000000000, 0.000000000000000000, 0.000000000000000000 ) ) ;
#24019 = CIRCLE ( 'NONE', #28731, 39.93581437244897359 ) ;
#24020 = ORIENTED_EDGE ( 'NONE', *, *, #16438, .F. ) ;
#24021 = DIRECTION ( 'NONE',  ( 0.000000000000000000, 0.000000000000000000, -1.000000000000000000 ) ) ;
#24022 = ORIENTED_EDGE ( 'NONE', *, *, #21210, .F. ) ;
#24023 = ORIENTED_EDGE ( 'NONE', *, *, #13583, .T. ) ;
#24024 = VECTOR ( 'NONE', #13874, 1000.000000000000000 ) ;
#24025 = ADVANCED_FACE ( 'NONE', ( #18581 ), #10583, .F. ) ;
#24026 = AXIS2_PLACEMENT_3D ( 'NONE', #27911, #12980, #5100 ) ;
#24027 = AXIS2_PLACEMENT_3D ( 'NONE', #15944, #1322, #25948 ) ;
#24028 = AXIS2_PLACEMENT_3D ( 'NONE', #29804, #2060, #7317 ) ;
#24029 = CYLINDRICAL_SURFACE ( 'NONE', #4534, 12.98419020052702599 ) ;
#24030 = CARTESIAN_POINT ( 'NONE',  ( -30.46736936537216067, 11.87712387757214927, 68.60098163695475648 ) ) ;
#24031 = CARTESIAN_POINT ( 'NONE',  ( -40.49636040740121956, 6.939949491715666774, 34.54930799450052348 ) ) ;
#24032 = EDGE_CURVE ( 'NONE', #777, #3764, #30442, .T. ) ;
#24033 = EDGE_CURVE ( 'NONE', #1812, #2291, #25347, .T. ) ;
#24034 = VERTEX_POINT ( 'NONE', #386 ) ;
#24035 = TOROIDAL_SURFACE ( 'NONE', #458, 67.99999999999997158, 4.000000000000000000 ) ;
#24036 = DIRECTION ( 'NONE',  ( -0.000000000000000000, -1.000000000000000000, -0.000000000000000000 ) ) ;
#24037 = VERTEX_POINT ( 'NONE', #722 ) ;
#24038 = DIRECTION ( 'NONE',  ( 0.000000000000000000, 1.000000000000000000, 0.000000000000000000 ) ) ;
#24039 = ORIENTED_EDGE ( 'NONE', *, *, #32359, .F. ) ;
#24040 = CARTESIAN_POINT ( 'NONE',  ( 21.09785597605719332, 12.06852548259731961, 47.04930799450051637 ) ) ;
#24041 = DIRECTION ( 'NONE',  ( -1.000000000000000000, 0.000000000000000000, 0.000000000000000000 ) ) ;
#24042 = LINE ( 'NONE', #31924, #30685 ) ;
#24043 = CARTESIAN_POINT ( 'NONE',  ( 47.09785597605719687, 19.86454579224779948, 47.04930799450078638 ) ) ;
#24044 = ORIENTED_EDGE ( 'NONE', *, *, #5227, .T. ) ;
#24045 = CYLINDRICAL_SURFACE ( 'NONE', #31545, 13.00000000000000533 ) ;
#24046 = DIRECTION ( 'NONE',  ( 0.4848096202463429427, 0.8746197071393925215, -2.352477780477436294E-16 ) ) ;
#24047 = DIRECTION ( 'NONE',  ( 1.000000000000000000, 0.000000000000000000, 0.000000000000000000 ) ) ;
#24048 = DIRECTION ( 'NONE',  ( -0.000000000000000000, -1.000000000000000000, 0.000000000000000000 ) ) ;
#24049 = DIRECTION ( 'NONE',  ( -1.101824276508909887E-16, 1.000000000000000000, -0.000000000000000000 ) ) ;
#24050 = ORIENTED_EDGE ( 'NONE', *, *, #10247, .T. ) ;
#24051 = CARTESIAN_POINT ( 'NONE',  ( 33.50134396954525329, 25.84164230456639899, 47.04930799450051637 ) ) ;
#24052 = DIRECTION ( 'NONE',  ( -1.224646799147353207E-16, 0.000000000000000000, -1.000000000000000000 ) ) ;
#24053 = ORIENTED_EDGE ( 'NONE', *, *, #8385, .F. ) ;
#24054 = EDGE_CURVE ( 'NONE', #25102, #18493, #8897, .T. ) ;
#24055 = DIRECTION ( 'NONE',  ( 0.000000000000000000, 1.000000000000000000, -0.000000000000000000 ) ) ;
#24056 = AXIS2_PLACEMENT_3D ( 'NONE', #31521, #2125, #12144 ) ;
#24057 = CIRCLE ( 'NONE', #30892, 12.48414152717711190 ) ;
#24058 = DIRECTION ( 'NONE',  ( 0.000000000000000000, 0.000000000000000000, 1.000000000000000000 ) ) ;
#24059 = ORIENTED_EDGE ( 'NONE', *, *, #4708, .F. ) ;
#24060 = ORIENTED_EDGE ( 'NONE', *, *, #24761, .F. ) ;
#24061 = AXIS2_PLACEMENT_3D ( 'NONE', #15426, #167, #30209 ) ;
#24062 = EDGE_LOOP ( 'NONE', ( #19085, #17648, #22645, #22891 ) ) ;
#24063 = AXIS2_PLACEMENT_3D ( 'NONE', #11470, #8846, #23778 ) ;
#24064 = EDGE_CURVE ( 'NONE', #25197, #22536, #2108, .T. ) ;
#24065 = ADVANCED_FACE ( 'NONE', ( #18110 ), #28295, .T. ) ;
#24066 = CARTESIAN_POINT ( 'NONE',  ( 21.09785597605720753, 14.86454579224779948, 47.04930799450052348 ) ) ;
#24067 = EDGE_CURVE ( 'NONE', #6401, #11200, #24323, .T. ) ;
#24068 = AXIS2_PLACEMENT_3D ( 'NONE', #21222, #31259, #8757 ) ;
#24069 = ORIENTED_EDGE ( 'NONE', *, *, #12826, .F. ) ;
#24070 = DIRECTION ( 'NONE',  ( 0.000000000000000000, -0.000000000000000000, -1.000000000000000000 ) ) ;
#24071 = EDGE_CURVE ( 'NONE', #25102, #13965, #6284, .T. ) ;
#24072 = DIRECTION ( 'NONE',  ( 0.000000000000000000, 0.000000000000000000, -1.000000000000000000 ) ) ;
#24073 = DIRECTION ( 'NONE',  ( -1.000000000000000000, 0.000000000000000000, 0.000000000000000000 ) ) ;
#24074 = DIRECTION ( 'NONE',  ( 0.000000000000000000, 1.000000000000000000, -0.000000000000000000 ) ) ;
#24075 = CARTESIAN_POINT ( 'NONE',  ( 49.44739180854976013, 29.47786309983297670, 47.17133137409169308 ) ) ;
#24076 = ORIENTED_EDGE ( 'NONE', *, *, #31628, .T. ) ;
#24077 = ORIENTED_EDGE ( 'NONE', *, *, #1295, .T. ) ;
#24078 = DIRECTION ( 'NONE',  ( 0.4848096202463673676, 0.8746197071393789768, 0.000000000000000000 ) ) ;
#24079 = ORIENTED_EDGE ( 'NONE', *, *, #11852, .T. ) ;
#24080 = CARTESIAN_POINT ( 'NONE',  ( 21.09785597605719332, 13.74476430820393347, 103.0493079945005093 ) ) ;
#24081 = CARTESIAN_POINT ( 'NONE',  ( -39.84249199961863042, 8.796534049953976364, 39.44930799450052206 ) ) ;
#24082 = VECTOR ( 'NONE', #26441, 1000.000000000000000 ) ;
#24083 = CIRCLE ( 'NONE', #492, 13.30165371409683850 ) ;
#24084 = CARTESIAN_POINT ( 'NONE',  ( -40.62121046050631179, 6.937850113512377348, 39.13688957799512025 ) ) ;
#24085 = DIRECTION ( 'NONE',  ( -1.000000000000000000, 0.000000000000000000, 0.000000000000000000 ) ) ;
#24086 = FACE_OUTER_BOUND ( 'NONE', #10153, .T. ) ;
#24087 = CARTESIAN_POINT ( 'NONE',  ( 48.46535932150934656, 24.78954579807171754, 49.73005965046827015 ) ) ;
#24088 = AXIS2_PLACEMENT_3D ( 'NONE', #19825, #12791, #5066 ) ;
#24089 = CARTESIAN_POINT ( 'NONE',  ( 46.61092110408701217, 23.04411657098542676, 48.07511952990385851 ) ) ;
#24090 = FACE_OUTER_BOUND ( 'NONE', #30181, .T. ) ;
#24091 = VERTEX_POINT ( 'NONE', #26142 ) ;
#24092 = CARTESIAN_POINT ( 'NONE',  ( 8.474859994195286461, 26.59143805560860940, 47.04930799450051637 ) ) ;
#24093 = AXIS2_PLACEMENT_3D ( 'NONE', #13535, #31581, #23537 ) ;
#24094 = FACE_OUTER_BOUND ( 'NONE', #29557, .T. ) ;
#24095 = CARTESIAN_POINT ( 'NONE',  ( 21.09785597605720753, 14.86454579224779948, 47.04930799450052348 ) ) ;
#24096 = DIRECTION ( 'NONE',  ( 0.000000000000000000, 0.000000000000000000, -1.000000000000000000 ) ) ;
#24097 = EDGE_LOOP ( 'NONE', ( #7040, #14502, #13808, #528 ) ) ;
#24098 = CARTESIAN_POINT ( 'NONE',  ( 33.72499318558949710, 24.84143805560860940, 47.04930799450051637 ) ) ;
#24099 = ORIENTED_EDGE ( 'NONE', *, *, #18618, .F. ) ;
#24100 = DIRECTION ( 'NONE',  ( -1.101824276508909887E-16, 1.000000000000000000, -0.000000000000000000 ) ) ;
#24101 = DIRECTION ( 'NONE',  ( 0.4848096202463673121, 0.8746197071393789768, 0.000000000000000000 ) ) ;
#24102 = CIRCLE ( 'NONE', #505, 0.1250000000000001110 ) ;
#24103 = AXIS2_PLACEMENT_3D ( 'NONE', #25976, #3486, #13999 ) ;
#24104 = ORIENTED_EDGE ( 'NONE', *, *, #18651, .F. ) ;
#24105 = EDGE_CURVE ( 'NONE', #9695, #7978, #14001, .T. ) ;
#24106 = AXIS2_PLACEMENT_3D ( 'NONE', #9648, #17517, #2580 ) ;
#24107 = AXIS2_PLACEMENT_3D ( 'NONE', #699, #2835, #8098 ) ;
#24108 = EDGE_CURVE ( 'NONE', #25827, #17347, #28938, .T. ) ;
#24109 = VECTOR ( 'NONE', #15496, 1000.000000000000000 ) ;
#24110 = EDGE_LOOP ( 'NONE', ( #1760, #4712, #30534, #25485 ) ) ;
#24111 = VECTOR ( 'NONE', #16276, 1000.000000000000000 ) ;
#24112 = DIRECTION ( 'NONE',  ( -1.101824276508909887E-16, 1.000000000000000000, -0.000000000000000000 ) ) ;
#24113 = DIRECTION ( 'NONE',  ( -1.101824276508909887E-16, 1.000000000000000000, -0.000000000000000000 ) ) ;
#24114 = DIRECTION ( 'NONE',  ( -0.1949050434465251780, 0.6797146636928671493, -0.7071067811865481278 ) ) ;
#24115 = EDGE_CURVE ( 'NONE', #9682, #23707, #3675, .T. ) ;
#24116 = ORIENTED_EDGE ( 'NONE', *, *, #31907, .F. ) ;
#24117 = DIRECTION ( 'NONE',  ( 0.9612616959383206705, 0.2756373558169926130, 8.795445018804289444E-19 ) ) ;
#24118 =( BOUNDED_SURFACE ( )  B_SPLINE_SURFACE ( 1, 2, ( 
 ( #7751, #13171, #30728, #17753, #7921, #8239, #2821, #27771, #12848, #22839, #5610, #353, #27937, #5456, #15458, #25470, #22998, #25629, #512, #10550, #30570, #3131, #21453, #18825, #29022, #4239, #16375, #14256, #9318, #24251, #29342, #9491, #28865, #24414, #16863, #13933, #12120, #6376, #27042, #26881, #26717, #11946, #7022, #9158, #6694, #19489, #1771, #6537, #29516, #26397, #17016, #19156, #14413, #8997, #4556, #14574, #1605, #21942, #23927, #24578, #31655, #14092, #11626, #31489, #4394, #3906, #1439, #11788, #31970, #11456, #26555, #21622, #2094, #16536, #19318, #29182, #18992, #22110, #21784, #4063, #31808, #24087, #6866, #32140, #16692 ),
 ( #1928, #17352, #12777, #7684, #9651, #17841, #22923, #20295, #5055, #29677, #19978, #27536, #30007, #15386, #27864, #24914, #27694, #30170, #15065, #2262, #20139, #25071, #7519, #9814, #9978, #125, #5383, #27373, #12282, #10143, #4890, #2583, #30327, #5215, #15223, #12936, #2429, #22765, #14905, #17520, #7841, #24748, #12612, #17676, #25393, #282, #2905, #22603, #19808, #12445, #29842, #22273, #25239, #7351, #2751, #10308, #19644, #7183, #17180, #32304, #27200, #4724, #14742, #22428, #32465, #16178, #3386, #3545, #26192, #3711, #8320, #25877, #23573, #13736, #18159, #20464, #1088, #20789, #15702, #441, #8646, #6023, #13419, #10470, #30495 ) ),
 .UNSPECIFIED., .F., .F., .F. ) 
 B_SPLINE_SURFACE_WITH_KNOTS ( ( 2, 2 ),
 ( 3, 2, 2, 2, 2, 2, 2, 2, 2, 2, 2, 2, 2, 2, 2, 2, 2, 2, 2, 2, 2, 2, 2, 2, 2, 2, 2, 2, 2, 2, 2, 2, 2, 2, 2, 2, 2, 2, 2, 2, 2, 2, 3 ),
 ( 0.000000000000000000, 1.000000000000000000 ),
 ( 0.000000000000000000, 0.02380952380952380820, 0.04761904761904761640, 0.07142857142857142461, 0.09523809523809523281, 0.1190476190476190410, 0.1428571428571428492, 0.1666666666666666574, 0.1904761904761904656, 0.2142857142857142738, 0.2380952380952380820, 0.2619047619047619180, 0.2857142857142856984, 0.3095238095238095344, 0.3333333333333333148, 0.3571428571428571508, 0.3809523809523809312, 0.4047619047619047672, 0.4285714285714285476, 0.4523809523809523836, 0.4761904761904761640, 0.5000000000000000000, 0.5238095238095238360, 0.5476190476190476719, 0.5714285714285713969, 0.5952380952380952328, 0.6190476190476190688, 0.6428571428571429047, 0.6666666666666666297, 0.6904761904761904656, 0.7142857142857143016, 0.7380952380952381375, 0.7619047619047618625, 0.7857142857142856984, 0.8095238095238095344, 0.8333333333333333703, 0.8571428571428570953, 0.8809523809523809312, 0.9047619047619047672, 0.9285714285714286031, 0.9523809523809523281, 0.9761904761904761640, 1.000000000000000000 ),
 .UNSPECIFIED. ) 
 GEOMETRIC_REPRESENTATION_ITEM ( )  RATIONAL_B_SPLINE_SURFACE ( (
 ( 1.000000000000000000, 0.8660254037844387076, 1.000000000000000000, 0.8660254037844387076, 1.000000000000000000, 0.8660254037844387076, 1.000000000000000000, 0.8660254037844387076, 1.000000000000000000, 0.8660254037844387076, 1.000000000000000000, 0.8660254037844387076, 1.000000000000000000, 0.8660254037844387076, 1.000000000000000000, 0.8660254037844387076, 1.000000000000000000, 0.8660254037844387076, 1.000000000000000000, 0.8660254037844387076, 1.000000000000000000, 0.8660254037844387076, 1.000000000000000000, 0.8660254037844387076, 1.000000000000000000, 0.8660254037844387076, 1.000000000000000000, 0.8660254037844387076, 1.000000000000000000, 0.8660254037844387076, 1.000000000000000000, 0.8660254037844387076, 1.000000000000000000, 0.8660254037844387076, 1.000000000000000000, 0.8660254037844387076, 1.000000000000000000, 0.8660254037844387076, 1.000000000000000000, 0.8660254037844387076, 1.000000000000000000, 0.8660254037844387076, 1.000000000000000000, 0.8660254037844387076, 1.000000000000000000, 0.8660254037844387076, 1.000000000000000000, 0.8660254037844387076, 1.000000000000000000, 0.8660254037844387076, 1.000000000000000000, 0.8660254037844387076, 1.000000000000000000, 0.8660254037844387076, 1.000000000000000000, 0.8660254037844387076, 1.000000000000000000, 0.8660254037844387076, 1.000000000000000000, 0.8660254037844387076, 1.000000000000000000, 0.8660254037844387076, 1.000000000000000000, 0.8660254037844387076, 1.000000000000000000, 0.8660254037844387076, 1.000000000000000000, 0.8660254037844387076, 1.000000000000000000, 0.8660254037844387076, 1.000000000000000000, 0.8660254037844387076, 1.000000000000000000, 0.8660254037844387076, 1.000000000000000000, 0.8660254037844387076, 1.000000000000000000, 0.8660254037844387076, 1.000000000000000000, 0.8660254037844387076, 1.000000000000000000, 0.8660254037844387076, 1.000000000000000000, 0.8660254037844387076, 1.000000000000000000),
 ( 1.000000000000000000, 0.8660254037844387076, 1.000000000000000000, 0.8660254037844387076, 1.000000000000000000, 0.8660254037844387076, 1.000000000000000000, 0.8660254037844387076, 1.000000000000000000, 0.8660254037844387076, 1.000000000000000000, 0.8660254037844387076, 1.000000000000000000, 0.8660254037844387076, 1.000000000000000000, 0.8660254037844387076, 1.000000000000000000, 0.8660254037844387076, 1.000000000000000000, 0.8660254037844387076, 1.000000000000000000, 0.8660254037844387076, 1.000000000000000000, 0.8660254037844387076, 1.000000000000000000, 0.8660254037844387076, 1.000000000000000000, 0.8660254037844387076, 1.000000000000000000, 0.8660254037844387076, 1.000000000000000000, 0.8660254037844387076, 1.000000000000000000, 0.8660254037844387076, 1.000000000000000000, 0.8660254037844387076, 1.000000000000000000, 0.8660254037844387076, 1.000000000000000000, 0.8660254037844387076, 1.000000000000000000, 0.8660254037844387076, 1.000000000000000000, 0.8660254037844387076, 1.000000000000000000, 0.8660254037844387076, 1.000000000000000000, 0.8660254037844387076, 1.000000000000000000, 0.8660254037844387076, 1.000000000000000000, 0.8660254037844387076, 1.000000000000000000, 0.8660254037844387076, 1.000000000000000000, 0.8660254037844387076, 1.000000000000000000, 0.8660254037844387076, 1.000000000000000000, 0.8660254037844387076, 1.000000000000000000, 0.8660254037844387076, 1.000000000000000000, 0.8660254037844387076, 1.000000000000000000, 0.8660254037844387076, 1.000000000000000000, 0.8660254037844387076, 1.000000000000000000, 0.8660254037844387076, 1.000000000000000000, 0.8660254037844387076, 1.000000000000000000, 0.8660254037844387076, 1.000000000000000000, 0.8660254037844387076, 1.000000000000000000, 0.8660254037844387076, 1.000000000000000000, 0.8660254037844387076, 1.000000000000000000, 0.8660254037844387076, 1.000000000000000000, 0.8660254037844387076, 1.000000000000000000) ) ) 
 REPRESENTATION_ITEM ( '' )  SURFACE ( )  );
#24119 = DIRECTION ( 'NONE',  ( 0.000000000000000000, 0.000000000000000000, -1.000000000000000000 ) ) ;
#24120 = CARTESIAN_POINT ( 'NONE',  ( 77.08942877945061412, -3.654479441960591490, 13.45888422241439919 ) ) ;
#24121 = ORIENTED_EDGE ( 'NONE', *, *, #22565, .F. ) ;
#24122 = DIRECTION ( 'NONE',  ( 0.000000000000000000, -8.673617379884027583E-16, -1.000000000000000000 ) ) ;
#24123 = ORIENTED_EDGE ( 'NONE', *, *, #24831, .T. ) ;
#24124 = DIRECTION ( 'NONE',  ( -1.000000000000000000, 0.000000000000000000, 0.000000000000000000 ) ) ;
#24125 = DIRECTION ( 'NONE',  ( 0.000000000000000000, -0.000000000000000000, -1.000000000000000000 ) ) ;
#24126 = CARTESIAN_POINT ( 'NONE',  ( 21.09992658989239089, 25.46664230456640254, 47.04930799450051637 ) ) ;
#24127 = CARTESIAN_POINT ( 'NONE',  ( 0.000000000000000000, 0.000000000000000000, 0.000000000000000000 ) ) ;
#24128 = ORIENTED_EDGE ( 'NONE', *, *, #27599, .T. ) ;
#24129 = VERTEX_POINT ( 'NONE', #21528 ) ;
#24130 = CARTESIAN_POINT ( 'NONE',  ( -40.23967075304302909, 7.740322171013528596, 60.29072935073781991 ) ) ;
#24131 = AXIS2_PLACEMENT_3D ( 'NONE', #20583, #6129, #16129 ) ;
#24132 = CARTESIAN_POINT ( 'NONE',  ( 46.04844006429464542, 22.80400562401889530, 44.99211097489548905 ) ) ;
#24133 = AXIS2_PLACEMENT_3D ( 'NONE', #16176, #16022, #28657 ) ;
#24134 = FACE_BOUND ( 'NONE', #31549, .T. ) ;
#24135 = ORIENTED_EDGE ( 'NONE', *, *, #22509, .T. ) ;
#24136 = CIRCLE ( 'NONE', #8424, 0.1000000000000006301 ) ;
#24137 = CARTESIAN_POINT ( 'NONE',  ( 67.39212317433587884, -13.74047052604243646, 82.56529288175445913 ) ) ;
#24138 = EDGE_LOOP ( 'NONE', ( #8549, #32472, #12150, #9640 ) ) ;
#24139 = DIRECTION ( 'NONE',  ( 0.000000000000000000, 0.000000000000000000, 1.000000000000000000 ) ) ;
#24140 = VECTOR ( 'NONE', #23404, 999.9999999999998863 ) ;
#24141 = DIRECTION ( 'NONE',  ( -1.000000000000000000, 0.000000000000000000, 0.000000000000000000 ) ) ;
#24142 = TOROIDAL_SURFACE ( 'NONE', #10002, 55.72393233686778302, 0.09999999999999760469 ) ;
#24143 = CIRCLE ( 'NONE', #8430, 12.62506659569710443 ) ;
#24144 = CARTESIAN_POINT ( 'NONE',  ( -40.70217169293939463, 9.596168124565082280, 38.54930799450053058 ) ) ;
#24145 = CIRCLE ( 'NONE', #29406, 25.00000000000000000 ) ;
#24146 = ORIENTED_EDGE ( 'NONE', *, *, #13952, .F. ) ;
#24147 = DIRECTION ( 'NONE',  ( -0.000000000000000000, 0.000000000000000000, -1.000000000000000000 ) ) ;
#24148 = DIRECTION ( 'NONE',  ( 0.9097384655268497822, 0.4151817967359032191, 2.820562191637069803E-18 ) ) ;
#24149 = CYLINDRICAL_SURFACE ( 'NONE', #14171, 2.000000000000001776 ) ;
#24150 = CARTESIAN_POINT ( 'NONE',  ( 45.79384627280941089, 27.86618040159426357, 49.05938063676249072 ) ) ;
#24151 = EDGE_CURVE ( 'NONE', #28989, #26286, #31564, .T. ) ;
#24152 = ORIENTED_EDGE ( 'NONE', *, *, #9066, .F. ) ;
#24153 = EDGE_CURVE ( 'NONE', #29601, #8764, #6302, .T. ) ;
#24154 = EDGE_CURVE ( 'NONE', #6349, #31093, #9994, .T. ) ;
#24155 = AXIS2_PLACEMENT_3D ( 'NONE', #31490, #21786, #9652 ) ;
#24156 = DIRECTION ( 'NONE',  ( -0.2756373558170082672, 0.9612616959383162296, 0.000000000000000000 ) ) ;
#24157 = DIRECTION ( 'NONE',  ( -1.101824276508909887E-16, 1.000000000000000000, -0.000000000000000000 ) ) ;
#24158 = AXIS2_PLACEMENT_3D ( 'NONE', #2895, #15689, #3213 ) ;
#24159 = CARTESIAN_POINT ( 'NONE',  ( 53.00177451235461490, 2.793366809690220887, -4.849114461849969082 ) ) ;
#24160 = TOROIDAL_SURFACE ( 'NONE', #11596, 48.97546517713167447, 2.000000000000000000 ) ;
#24161 = CARTESIAN_POINT ( 'NONE',  ( 33.71785032049133690, 28.71664230456639899, 47.04930799450051637 ) ) ;
#24162 = LINE ( 'NONE', #21526, #14799 ) ;
#24163 = DIRECTION ( 'NONE',  ( 0.8746197071393925215, -0.4848096202463429982, -8.676864087101709653E-18 ) ) ;
#24164 = DIRECTION ( 'NONE',  ( -0.000000000000000000, -1.000000000000000000, -0.000000000000000000 ) ) ;
#24165 = CARTESIAN_POINT ( 'NONE',  ( 44.21498992391907024, 27.99488759933318605, 46.89958605635244027 ) ) ;
#24166 = ORIENTED_EDGE ( 'NONE', *, *, #26449, .T. ) ;
#24167 = CARTESIAN_POINT ( 'NONE',  ( 46.15191711366536254, 22.98879437201065912, 45.92598426414627255 ) ) ;
#24168 = AXIS2_PLACEMENT_3D ( 'NONE', #24980, #12354, #17915 ) ;
#24169 = CARTESIAN_POINT ( 'NONE',  ( -40.39264216188491474, 8.574558558407114006, 34.58262810048215385 ) ) ;
#24170 = DIRECTION ( 'NONE',  ( -2.779292025043186357E-18, 1.288349127009862211E-17, -1.000000000000000000 ) ) ;
#24171 = CARTESIAN_POINT ( 'NONE',  ( 33.46699938050304013, 30.46183152705961561, 47.04930799450051637 ) ) ;
#24172 = ORIENTED_EDGE ( 'NONE', *, *, #8193, .T. ) ;
#24173 = DIRECTION ( 'NONE',  ( 0.9097384655268497822, 0.4151817967359032191, 2.820562191637069417E-18 ) ) ;
#24174 = CARTESIAN_POINT ( 'NONE',  ( -40.18454328187963398, 7.548069831825863218, 53.64930799450051779 ) ) ;
#24175 = CARTESIAN_POINT ( 'NONE',  ( 21.09785597605720753, -5.098646251524523443, 47.04930799450052348 ) ) ;
#24176 = ORIENTED_EDGE ( 'NONE', *, *, #13181, .F. ) ;
#24177 = DIRECTION ( 'NONE',  ( 0.000000000000000000, 0.000000000000000000, 1.000000000000000000 ) ) ;
#24178 = CARTESIAN_POINT ( 'NONE',  ( 21.09785597605720042, 24.74924423484549507, 86.98512236694949706 ) ) ;
#24179 = LINE ( 'NONE', #8759, #22517 ) ;
#24180 = CARTESIAN_POINT ( 'NONE',  ( 53.16169625780806740, -5.983766253076982622, 106.7232700815558957 ) ) ;
#24181 = AXIS2_PLACEMENT_3D ( 'NONE', #3220, #15536, #18474 ) ;
#24182 = EDGE_LOOP ( 'NONE', ( #11384, #29996, #24907, #7366 ) ) ;
#24183 = LINE ( 'NONE', #19086, #5720 ) ;
#24184 = CIRCLE ( 'NONE', #27882, 12.27641737965284108 ) ;
#24185 = ORIENTED_EDGE ( 'NONE', *, *, #20525, .F. ) ;
#24186 = AXIS2_PLACEMENT_3D ( 'NONE', #29790, #17302, #4842 ) ;
#24187 = EDGE_CURVE ( 'NONE', #4406, #26923, #26309, .T. ) ;
#24188 =( REPRESENTATION_RELATIONSHIP ('NONE','NONE', #20382, #21423 ) REPRESENTATION_RELATIONSHIP_WITH_TRANSFORMATION ( #17713 )SHAPE_REPRESENTATION_RELATIONSHIP( ) );
#24189 = VERTEX_POINT ( 'NONE', #16603 ) ;
#24190 = PLANE ( 'NONE',  #31004 ) ;
#24191 = AXIS2_PLACEMENT_3D ( 'NONE', #4551, #2087, #14737 ) ;
#24192 = EDGE_CURVE ( 'NONE', #8696, #9808, #14185, .T. ) ;
#24193 = EDGE_CURVE ( 'NONE', #13402, #21924, #13136, .T. ) ;
#24194 = ADVANCED_FACE ( 'NONE', ( #13685 ), #16450, .F. ) ;
#24195 = CARTESIAN_POINT ( 'NONE',  ( 21.09785597605719687, 15.63322284159649556, 94.10733885242261465 ) ) ;
#24196 = CARTESIAN_POINT ( 'NONE',  ( -29.34961020680567501, 9.276496357494197653, 74.28030578752274948 ) ) ;
#24197 = CARTESIAN_POINT ( 'NONE',  ( -40.02540636251513462, 2.839176264122873050, 39.04930799450052348 ) ) ;
#24198 = ADVANCED_FACE ( 'NONE', ( #21695 ), #31723, .F. ) ;
#24199 = EDGE_CURVE ( 'NONE', #7112, #27336, #21356, .T. ) ;
#24200 = EDGE_LOOP ( 'NONE', ( #32195, #10850, #27260 ) ) ;
#24201 = DIRECTION ( 'NONE',  ( -0.9612616959383083470, -0.2756373558170356897, 0.000000000000000000 ) ) ;
#24202 = ORIENTED_EDGE ( 'NONE', *, *, #10127, .T. ) ;
#24203 = AXIS2_PLACEMENT_3D ( 'NONE', #15502, #5819, #28463 ) ;
#24204 = VECTOR ( 'NONE', #12101, 1000.000000000000114 ) ;
#24205 = DIRECTION ( 'NONE',  ( -0.000000000000000000, -1.000000000000000000, -0.000000000000000000 ) ) ;
#24206 = CIRCLE ( 'NONE', #9550, 1.899999999999999023 ) ;
#24207 = CARTESIAN_POINT ( 'NONE',  ( 21.09992658989239089, 24.84164230456639544, 47.04930799450051637 ) ) ;
#24208 = FACE_OUTER_BOUND ( 'NONE', #7532, .T. ) ;
#24209 = ORIENTED_EDGE ( 'NONE', *, *, #31392, .T. ) ;
#24210 = FACE_OUTER_BOUND ( 'NONE', #15525, .T. ) ;
#24211 = CYLINDRICAL_SURFACE ( 'NONE', #3229, 12.62506659569710266 ) ;
#24212 = FACE_OUTER_BOUND ( 'NONE', #23108, .T. ) ;
#24213 = ORIENTED_EDGE ( 'NONE', *, *, #2803, .F. ) ;
#24214 = CARTESIAN_POINT ( 'NONE',  ( 21.09785597605719332, 25.56454579224779877, 47.04930799450051637 ) ) ;
#24215 = DIRECTION ( 'NONE',  ( 0.000000000000000000, 0.000000000000000000, -1.000000000000000000 ) ) ;
#24216 = CARTESIAN_POINT ( 'NONE',  ( 21.09785597605720753, -13.88867167006704939, 105.7507399849467475 ) ) ;
#24217 = LINE ( 'NONE', #31453, #5959 ) ;
#24218 = SURFACE_STYLE_USAGE ( .BOTH. , #13894 ) ;
#24219 = ORIENTED_EDGE ( 'NONE', *, *, #27109, .T. ) ;
#24220 = DIRECTION ( 'NONE',  ( 0.000000000000000000, 0.000000000000000000, 1.000000000000000000 ) ) ;
#24221 = DIRECTION ( 'NONE',  ( 0.4544104193609903586, 0.000000000000000000, 0.8907924397839087627 ) ) ;
#24222 = ORIENTED_EDGE ( 'NONE', *, *, #9635, .T. ) ;
#24223 = CARTESIAN_POINT ( 'NONE',  ( -43.86787645162945637, -4.885237077964406538, 41.81402935846817570 ) ) ;
#24224 = CARTESIAN_POINT ( 'NONE',  ( -40.02540636251513462, 2.839176264122873050, 39.04930799450052348 ) ) ;
#24225 = TOROIDAL_SURFACE ( 'NONE', #27372, 58.88977237527051756, 0.5999999999999987566 ) ;
#24226 = ORIENTED_EDGE ( 'NONE', *, *, #16552, .F. ) ;
#24227 = ORIENTED_EDGE ( 'NONE', *, *, #9990, .T. ) ;
#24228 = EDGE_CURVE ( 'NONE', #16912, #31503, #18863, .T. ) ;
#24229 = ADVANCED_FACE ( 'NONE', ( #6124 ), #25701, .F. ) ;
#24230 = ORIENTED_EDGE ( 'NONE', *, *, #7356, .T. ) ;
#24231 = CIRCLE ( 'NONE', #9025, 22.00000000000000000 ) ;
#24232 = DIRECTION ( 'NONE',  ( -1.000000000000000000, 0.000000000000000000, 0.000000000000000000 ) ) ;
#24233 = EDGE_CURVE ( 'NONE', #19067, #30753, #16247, .T. ) ;
#24234 = ORIENTED_EDGE ( 'NONE', *, *, #3520, .F. ) ;
#24235 = DIRECTION ( 'NONE',  ( 0.000000000000000000, 0.000000000000000000, -1.000000000000000000 ) ) ;
#24236 = CARTESIAN_POINT ( 'NONE',  ( -40.41647043964083252, 8.356895951721261540, 54.54930799450051637 ) ) ;
#24237 = DIRECTION ( 'NONE',  ( -1.000000000000000000, 0.000000000000000000, 0.000000000000000000 ) ) ;
#24238 = CARTESIAN_POINT ( 'NONE',  ( -40.50727813154207269, 7.559769128450253284, 53.81525338917477796 ) ) ;
#24239 = CIRCLE ( 'NONE', #12193, 55.62842601856165459 ) ;
#24240 = CARTESIAN_POINT ( 'NONE',  ( 46.99218062947583974, 28.60286309983298381, 49.08406571254116102 ) ) ;
#24241 = ORIENTED_EDGE ( 'NONE', *, *, #12015, .F. ) ;
#24242 = CARTESIAN_POINT ( 'NONE',  ( 21.09992658989239089, 30.34184655352422411, 47.04930799450051637 ) ) ;
#24243 = VERTEX_POINT ( 'NONE', #31402 ) ;
#24244 = CARTESIAN_POINT ( 'NONE',  ( -9.880269303432738681, -5.935454207752202116, -10.95525492004900769 ) ) ;
#24245 = ORIENTED_EDGE ( 'NONE', *, *, #15400, .F. ) ;
#24246 = CARTESIAN_POINT ( 'NONE',  ( 48.71516269694878076, 29.58372224308939025, 45.72934403980688955 ) ) ;
#24247 = CARTESIAN_POINT ( 'NONE',  ( 21.09785597605719687, 30.56454579224779522, 30.04930799450051282 ) ) ;
#24248 = DIRECTION ( 'NONE',  ( -0.000000000000000000, -1.000000000000000000, -0.000000000000000000 ) ) ;
#24249 = DIRECTION ( 'NONE',  ( 0.2756373558169947779, -0.9612616959383200044, 0.000000000000000000 ) ) ;
#24250 = FACE_BOUND ( 'NONE', #9803, .T. ) ;
#24251 = CARTESIAN_POINT ( 'NONE',  ( 48.73570333863616355, 27.82287913140503832, 44.52463952959527660 ) ) ;
#24252 = CIRCLE ( 'NONE', #15364, 0.1249999999999983763 ) ;
#24253 = CARTESIAN_POINT ( 'NONE',  ( 47.28721660713063812, 22.91413368675619111, 48.84239091338285732 ) ) ;
#24254 = DIRECTION ( 'NONE',  ( 0.7141240004913296247, -0.3958453973319808195, 0.5773502691896363892 ) ) ;
#24255 = EDGE_CURVE ( 'NONE', #4827, #12851, #9467, .T. ) ;
#24256 = VERTEX_POINT ( 'NONE', #30082 ) ;
#24257 = CARTESIAN_POINT ( 'NONE',  ( 21.09992658989239089, 27.34143805560860940, 47.04930799450051637 ) ) ;
#24258 = DIRECTION ( 'NONE',  ( 0.000000000000000000, -6.672013369141553384E-16, 1.000000000000000000 ) ) ;
#24259 = CARTESIAN_POINT ( 'NONE',  ( 21.09785597605719332, 7.237299147902269247, 47.04930799450051637 ) ) ;
#24260 = EDGE_CURVE ( 'NONE', #382, #15550, #32048, .T. ) ;
#24261 = DIRECTION ( 'NONE',  ( -1.000000000000000000, 0.000000000000000000, 0.000000000000000000 ) ) ;
#24262 = CARTESIAN_POINT ( 'NONE',  ( -38.57628410747783221, 11.23353061944650655, 22.24400271019782593 ) ) ;
#24263 = ORIENTED_EDGE ( 'NONE', *, *, #6366, .F. ) ;
#24264 = DIRECTION ( 'NONE',  ( -1.431146867680865853E-17, -2.558717127065790464E-17, -1.000000000000000000 ) ) ;
#24265 = EDGE_LOOP ( 'NONE', ( #28160, #1106, #24241, #20110, #31041, #7405, #19186, #30526, #8615, #5598, #25287, #7190, #22742, #30877, #15356, #2315, #1373, #31748 ) ) ;
#24266 = DIRECTION ( 'NONE',  ( -1.101824276508909887E-16, 1.000000000000000000, -0.000000000000000000 ) ) ;
#24267 = FACE_OUTER_BOUND ( 'NONE', #26390, .T. ) ;
#24268 = EDGE_CURVE ( 'NONE', #29214, #2165, #26211, .T. ) ;
#24269 = ADVANCED_FACE ( 'NONE', ( #14493, #14816 ), #7094, .T. ) ;
#24270 = ADVANCED_FACE ( 'NONE', ( #15137 ), #25, .F. ) ;
#24271 = ORIENTED_EDGE ( 'NONE', *, *, #18576, .F. ) ;
#24272 = CIRCLE ( 'NONE', #6983, 12.48414152717711900 ) ;
#24273 = CIRCLE ( 'NONE', #28480, 2.000000000000001776 ) ;
#24274 = AXIS2_PLACEMENT_3D ( 'NONE', #10918, #5663, #31103 ) ;
#24275 = AXIS2_PLACEMENT_3D ( 'NONE', #14258, #24750, #31657 ) ;
#24276 = ORIENTED_EDGE ( 'NONE', *, *, #12036, .F. ) ;
#24277 = CARTESIAN_POINT ( 'NONE',  ( 33.72499318558949710, 24.09143805560860940, 47.04930799450051637 ) ) ;
#24278 = EDGE_CURVE ( 'NONE', #28333, #257, #19414, .T. ) ;
#24279 = DIRECTION ( 'NONE',  ( -1.000000000000000000, -1.101824276508910010E-16, 0.000000000000000000 ) ) ;
#24280 = CARTESIAN_POINT ( 'NONE',  ( 21.09992658989238734, 38.56284415653841791, 47.04930799450051637 ) ) ;
#24281 = ORIENTED_EDGE ( 'NONE', *, *, #15853, .T. ) ;
#24282 = PLANE ( 'NONE',  #12548 ) ;
#24283 = CARTESIAN_POINT ( 'NONE',  ( 21.09785597605720753, 14.86454579224779948, 47.04930799450052348 ) ) ;
#24284 = CARTESIAN_POINT ( 'NONE',  ( 72.92745752893763722, 6.334306897662558278, 17.30572780667399968 ) ) ;
#24285 = EDGE_LOOP ( 'NONE', ( #28728, #6367 ) ) ;
#24286 = CARTESIAN_POINT ( 'NONE',  ( 45.50174972710295407, 22.86454579224779593, 48.32172736629423326 ) ) ;
#24287 = VERTEX_POINT ( 'NONE', #24656 ) ;
#24288 = SPHERICAL_SURFACE ( 'NONE', #19666, 36.01080762834750715 ) ;
#24289 = DIRECTION ( 'NONE',  ( -2.779292025043186357E-18, 1.288349127009862211E-17, -1.000000000000000000 ) ) ;
#24290 = CIRCLE ( 'NONE', #188, 1.500000000000001332 ) ;
#24291 = CARTESIAN_POINT ( 'NONE',  ( 33.72499318558949000, 38.56284415653841791, 47.04930799450051637 ) ) ;
#24292 = ADVANCED_FACE ( 'NONE', ( #12522 ), #17096, .F. ) ;
#24293 = ORIENTED_EDGE ( 'NONE', *, *, #29533, .T. ) ;
#24294 = EDGE_LOOP ( 'NONE', ( #4538, #8001, #30509, #3478 ) ) ;
#24295 = DIRECTION ( 'NONE',  ( -1.000000000000000000, 0.000000000000000000, 0.000000000000000000 ) ) ;
#24296 = CARTESIAN_POINT ( 'NONE',  ( 46.92175814837349179, 22.74928388133296764, 44.57455356976052485 ) ) ;
#24297 = EDGE_CURVE ( 'NONE', #12758, #3218, #6840, .T. ) ;
#24298 = CIRCLE ( 'NONE', #9636, 0.1000000000000006301 ) ;
#24299 = FACE_OUTER_BOUND ( 'NONE', #21973, .T. ) ;
#24300 = ORIENTED_EDGE ( 'NONE', *, *, #24255, .F. ) ;
#24301 = CIRCLE ( 'NONE', #1241, 12.62506659569710266 ) ;
#24302 = CARTESIAN_POINT ( 'NONE',  ( -12.57422076041892645, -1.761407059904331218, -7.664706412628855325 ) ) ;
#24303 = DIRECTION ( 'NONE',  ( -1.000000000000000000, 0.000000000000000000, 0.000000000000000000 ) ) ;
#24304 = AXIS2_PLACEMENT_3D ( 'NONE', #2430, #12938, #29844 ) ;
#24305 = ORIENTED_EDGE ( 'NONE', *, *, #17217, .F. ) ;
#24306 = CARTESIAN_POINT ( 'NONE',  ( 8.823509210239528500, 26.34164230456639899, 47.04930799450051637 ) ) ;
#24307 = CARTESIAN_POINT ( 'NONE',  ( 44.91142894931555674, 25.89787913140504472, 45.63089057098605394 ) ) ;
#24308 = EDGE_CURVE ( 'NONE', #22635, #22214, #29379, .T. ) ;
#24309 = DIRECTION ( 'NONE',  ( 0.3428121700606640565, 0.6184495258776567805, -0.7071067811865474617 ) ) ;
#24310 = EDGE_CURVE ( 'NONE', #5411, #4161, #25145, .T. ) ;
#24311 = VERTEX_POINT ( 'NONE', #14653 ) ;
#24312 = DIRECTION ( 'NONE',  ( -1.101824276508909887E-16, 1.000000000000000000, -0.000000000000000000 ) ) ;
#24313 = DIRECTION ( 'NONE',  ( 0.000000000000000000, 0.000000000000000000, 1.000000000000000000 ) ) ;
#24314 = DIRECTION ( 'NONE',  ( 0.4848096202463636484, 0.8746197071393810862, 0.000000000000000000 ) ) ;
#24315 = CARTESIAN_POINT ( 'NONE',  ( 47.20547626766766314, 27.57451373492759572, 44.97710074790751378 ) ) ;
#24316 = ORIENTED_EDGE ( 'NONE', *, *, #26978, .F. ) ;
#24317 = DIRECTION ( 'NONE',  ( 0.000000000000000000, 0.000000000000000000, 1.000000000000000000 ) ) ;
#24318 = CARTESIAN_POINT ( 'NONE',  ( -40.35915383839597581, 8.550197532140535017, 39.44930799450052206 ) ) ;
#24319 = FACE_OUTER_BOUND ( 'NONE', #11242, .T. ) ;
#24320 = FACE_OUTER_BOUND ( 'NONE', #13034, .T. ) ;
#24321 = CARTESIAN_POINT ( 'NONE',  ( 21.09992658989238734, 31.84143805560860940, 47.04930799450051637 ) ) ;
#24322 = CARTESIAN_POINT ( 'NONE',  ( -31.23570478744295542, -13.74047052604243646, 72.85129969572992081 ) ) ;
#24323 = LINE ( 'NONE', #26466, #17308 ) ;
#24324 = EDGE_LOOP ( 'NONE', ( #6204, #8063, #18177, #17646 ) ) ;
#24325 = DIRECTION ( 'NONE',  ( -1.101824276508909887E-16, 1.000000000000000000, -0.000000000000000000 ) ) ;
#24326 = FACE_OUTER_BOUND ( 'NONE', #16320, .T. ) ;
#24327 = DIRECTION ( 'NONE',  ( -2.779292025043186357E-18, 1.288349127009862211E-17, -1.000000000000000000 ) ) ;
#24328 = CYLINDRICAL_SURFACE ( 'NONE', #30468, 0.9031915329475500576 ) ;
#24329 = VECTOR ( 'NONE', #20884, 1000.000000000000000 ) ;
#24330 = VERTEX_POINT ( 'NONE', #12189 ) ;
#24331 = CARTESIAN_POINT ( 'NONE',  ( -40.41647043964083252, 8.356895951721261540, 59.44930799450051495 ) ) ;
#24332 = CARTESIAN_POINT ( 'NONE',  ( -42.21246928125516718, 14.65068104870687726, 37.04930799450052348 ) ) ;
#24333 = DIRECTION ( 'NONE',  ( -0.000000000000000000, -1.000000000000000000, -0.000000000000000000 ) ) ;
#24334 = ORIENTED_EDGE ( 'NONE', *, *, #14233, .T. ) ;
#24335 = EDGE_LOOP ( 'NONE', ( #18402, #12488 ) ) ;
#24337 = TOROIDAL_SURFACE ( 'NONE', #10200, 12.61792373059899219, 0.1249999999999961003 ) ;
#24336 = CARTESIAN_POINT ( 'NONE',  ( -40.11729073372970333, 6.802967823440400963, 39.44930799450052206 ) ) ;
#24338 = CARTESIAN_POINT ( 'NONE',  ( 48.23388202445966755, 15.77906836436399374, 49.27628909396055690 ) ) ;
#24339 = AXIS2_PLACEMENT_3D ( 'NONE', #4306, #9067, #14323 ) ;
#24340 = CARTESIAN_POINT ( 'NONE',  ( 21.09785597605719332, -16.63545420775219696, -32.16074251183835031 ) ) ;
#24341 = ADVANCED_FACE ( 'NONE', ( #2660 ), #4470, .F. ) ;
#24342 = CARTESIAN_POINT ( 'NONE',  ( 47.79865503179234310, 9.702389020015065313, 106.7232700815558957 ) ) ;
#24343 = TOROIDAL_SURFACE ( 'NONE', #10205, 1.899999999999999467, 0.1000000000000000056 ) ;
#24344 = ADVANCED_FACE ( 'NONE', ( #5123 ), #32213, .F. ) ;
#24345 = ADVANCED_FACE ( 'NONE', ( #38 ), #7263, .T. ) ;
#24346 = ORIENTED_EDGE ( 'NONE', *, *, #24638, .T. ) ;
#24347 = DIRECTION ( 'NONE',  ( 0.000000000000000000, -0.000000000000000000, -1.000000000000000000 ) ) ;
#24348 = EDGE_LOOP ( 'NONE', ( #5689, #9766, #32406, #2277 ) ) ;
#24349 = EDGE_LOOP ( 'NONE', ( #1180, #831, #25371, #9520 ) ) ;
#24350 = CARTESIAN_POINT ( 'NONE',  ( 52.16615856333482526, -5.937394852768787423, 107.4212530892143889 ) ) ;
#24351 = ORIENTED_EDGE ( 'NONE', *, *, #27990, .F. ) ;
#24352 = AXIS2_PLACEMENT_3D ( 'NONE', #28249, #990, #25936 ) ;
#24354 = CARTESIAN_POINT ( 'NONE',  ( -42.30123736278718383, 13.66041317296246937, 59.53596428539564300 ) ) ;
#24353 = B_SPLINE_CURVE_WITH_KNOTS ( 'NONE', 3,
 ( #16850, #14242, #16676, #14078, #26701, #1261, #29327, #24238, #19303, #6364 ),
 .UNSPECIFIED., .F., .F.,
 ( 4, 3, 3, 4 ),
 ( 0.000000000000000000, 3.371050856462795163E-05, 6.737649377718237724E-05, 7.827667330985808435E-05 ),
 .UNSPECIFIED. ) ;
#24355 = DIRECTION ( 'NONE',  ( -1.101824276508909887E-16, 1.000000000000000000, -0.000000000000000000 ) ) ;
#24356 = CONICAL_SURFACE ( 'NONE', #23314, 54.55130244989821620, 1.291543646475813212 ) ;
#24357 = DIRECTION ( 'NONE',  ( -1.000000000000000000, -1.101824276508909887E-16, 0.000000000000000000 ) ) ;
#24358 = VECTOR ( 'NONE', #21771, 1000.000000000000000 ) ;
#24359 = AXIS2_PLACEMENT_3D ( 'NONE', #2318, #10036, #29570 ) ;
#24360 = ORIENTED_EDGE ( 'NONE', *, *, #29461, .T. ) ;
#24361 = PLANE ( 'NONE',  #13930 ) ;
#24362 = ORIENTED_EDGE ( 'NONE', *, *, #9597, .T. ) ;
#24363 = CIRCLE ( 'NONE', #32240, 84.30000000000001137 ) ;
#24364 = DIRECTION ( 'NONE',  ( 0.000000000000000000, 0.000000000000000000, 1.000000000000000000 ) ) ;
#24365 = DIRECTION ( 'NONE',  ( 0.8746197071393895239, -0.4848096202463486604, -1.277302113040671208E-17 ) ) ;
#24366 = CARTESIAN_POINT ( 'NONE',  ( -40.65766396543777716, 6.815881913223422295, 39.50959409847852299 ) ) ;
#24367 = EDGE_LOOP ( 'NONE', ( #845, #2713 ) ) ;
#24368 = DIRECTION ( 'NONE',  ( 0.000000000000000000, 0.000000000000000000, -1.000000000000000000 ) ) ;
#24369 = DIRECTION ( 'NONE',  ( -1.000000000000000000, 0.000000000000000000, 0.000000000000000000 ) ) ;
#24370 = DIRECTION ( 'NONE',  ( -0.000000000000000000, -1.000000000000000000, -0.000000000000000000 ) ) ;
#24371 = DIRECTION ( 'NONE',  ( 0.2756373558169947779, -0.9612616959383203374, -1.385316060672546240E-15 ) ) ;
#24372 = CARTESIAN_POINT ( 'NONE',  ( 8.474859994195286461, 29.34184655352418858, 47.04930799450051637 ) ) ;
#24373 = DIRECTION ( 'NONE',  ( 1.000000000000000000, 0.000000000000000000, 0.000000000000000000 ) ) ;
#24374 =( NAMED_UNIT ( * ) SI_UNIT ( $, .STERADIAN. ) SOLID_ANGLE_UNIT ( ) );
#24375 = ORIENTED_EDGE ( 'NONE', *, *, #24855, .F. ) ;
#24376 = CARTESIAN_POINT ( 'NONE',  ( -40.12099660621151997, 7.356848571226008993, 35.24284630439623811 ) ) ;
#24377 = CARTESIAN_POINT ( 'NONE',  ( 21.09785597605719332, -6.659195188345857552, 47.04930799450051637 ) ) ;
#24378 = ORIENTED_EDGE ( 'NONE', *, *, #4882, .F. ) ;
#24379 = FACE_OUTER_BOUND ( 'NONE', #22807, .T. ) ;
#24380 = ADVANCED_FACE ( 'NONE', ( #2004 ), #19721, .F. ) ;
#24381 = ORIENTED_EDGE ( 'NONE', *, *, #7538, .F. ) ;
#24382 = CIRCLE ( 'NONE', #31724, 2.000000000000001776 ) ;
#24383 = EDGE_CURVE ( 'NONE', #21242, #17105, #13667, .T. ) ;
#24384 = ORIENTED_EDGE ( 'NONE', *, *, #23970, .F. ) ;
#24385 = ADVANCED_FACE ( 'NONE', ( #12023 ), #20444, .T. ) ;
#24386 = AXIS2_PLACEMENT_3D ( 'NONE', #21780, #21620, #24085 ) ;
#24387 = ADVANCED_FACE ( 'NONE', ( #22016 ), #27266, .T. ) ;
#24388 = AXIS2_PLACEMENT_3D ( 'NONE', #12070, #6491, #4021 ) ;
#24389 = AXIS2_PLACEMENT_3D ( 'NONE', #29588, #29750, #13887 ) ;
#24390 = VECTOR ( 'NONE', #28127, 1000.000000000000000 ) ;
#24391 = ORIENTED_EDGE ( 'NONE', *, *, #24268, .T. ) ;
#24392 = EDGE_CURVE ( 'NONE', #30056, #5110, #10710, .T. ) ;
#24393 = CARTESIAN_POINT ( 'NONE',  ( -40.11286833322908052, 2.887657226147509970, 55.04930799450051637 ) ) ;
#24394 = ORIENTED_EDGE ( 'NONE', *, *, #12784, .T. ) ;
#24395 = ORIENTED_EDGE ( 'NONE', *, *, #11522, .T. ) ;
#24396 = CYLINDRICAL_SURFACE ( 'NONE', #22639, 78.50000000000000000 ) ;
#24397 = CARTESIAN_POINT ( 'NONE',  ( -40.69193635511749108, 9.347952559758583746, 39.44930799450052206 ) ) ;
#24398 = CARTESIAN_POINT ( 'NONE',  ( 21.09785597605719332, 25.56454579224779167, 47.04930799450051637 ) ) ;
#24399 = DIRECTION ( 'NONE',  ( 0.000000000000000000, 0.000000000000000000, 1.000000000000000000 ) ) ;
#24400 = CARTESIAN_POINT ( 'NONE',  ( 47.20353132263855400, 27.55286309983298310, 45.01455027646040463 ) ) ;
#24401 = ADVANCED_FACE ( 'NONE', ( #5608 ), #8941, .T. ) ;
#24402 = ORIENTED_EDGE ( 'NONE', *, *, #18960, .F. ) ;
#24403 = CARTESIAN_POINT ( 'NONE',  ( -38.59984781516420327, -5.935454207752198563, 77.87546120947918382 ) ) ;
#24404 = VERTEX_POINT ( 'NONE', #20366 ) ;
#24406 = CARTESIAN_POINT ( 'NONE',  ( 21.09785597605719332, 40.56454579224780588, 59.54930799450053769 ) ) ;
#24405 = VECTOR ( 'NONE', #16128, 1000.000000000000000 ) ;
#24407 = CIRCLE ( 'NONE', #15490, 31.00000000000000000 ) ;
#24408 = ORIENTED_EDGE ( 'NONE', *, *, #16659, .F. ) ;
#24409 = CARTESIAN_POINT ( 'NONE',  ( 81.54161849434414933, -5.935454207752202116, 77.87546120947918382 ) ) ;
#24410 = FACE_OUTER_BOUND ( 'NONE', #9093, .T. ) ;
#24411 = CARTESIAN_POINT ( 'NONE',  ( 48.35473289974373756, 22.80400562401889530, 45.11188864597615833 ) ) ;
#24412 = CARTESIAN_POINT ( 'NONE',  ( -39.64148344771002286, 7.657122216028890982, 32.14930799450051779 ) ) ;
#24413 = DIRECTION ( 'NONE',  ( -1.000000000000000000, 0.000000000000000000, 0.000000000000000000 ) ) ;
#24414 = CARTESIAN_POINT ( 'NONE',  ( 48.46535932150934656, 27.58954579807170759, 49.73005965046827015 ) ) ;
#24415 = CARTESIAN_POINT ( 'NONE',  ( 47.07819351491129822, 23.11533908250407165, 47.42790437944410087 ) ) ;
#24416 = LINE ( 'NONE', #19158, #18005 ) ;
#24417 = ORIENTED_EDGE ( 'NONE', *, *, #15802, .F. ) ;
#24418 = FACE_OUTER_BOUND ( 'NONE', #30790, .T. ) ;
#24419 = FACE_BOUND ( 'NONE', #5083, .T. ) ;
#24420 = DIRECTION ( 'NONE',  ( -0.2756373558169974980, 0.9612616959383193382, 1.315048337272770589E-17 ) ) ;
#24421 = AXIS2_PLACEMENT_3D ( 'NONE', #8543, #18533, #18855 ) ;
#24422 = CARTESIAN_POINT ( 'NONE',  ( 48.00894325680572194, 23.03451764446789696, 46.25432281694521919 ) ) ;
#24423 = CARTESIAN_POINT ( 'NONE',  ( -29.27337757263006424, 8.768497289655476479, 19.08884019352816352 ) ) ;
#24424 = ORIENTED_EDGE ( 'NONE', *, *, #27305, .F. ) ;
#24425 = ORIENTED_EDGE ( 'NONE', *, *, #15677, .T. ) ;
#24426 = FACE_OUTER_BOUND ( 'NONE', #17327, .T. ) ;
#24427 = DIRECTION ( 'NONE',  ( -1.101824276508909887E-16, 1.000000000000000000, -0.000000000000000000 ) ) ;
#24428 = ADVANCED_FACE ( 'NONE', ( #30238 ), #681, .F. ) ;
#24429 = ORIENTED_EDGE ( 'NONE', *, *, #23114, .T. ) ;
#24430 = STYLED_ITEM ( 'NONE', ( #29556 ), #30825 ) ;
#24431 = ORIENTED_EDGE ( 'NONE', *, *, #5815, .T. ) ;
#24432 = EDGE_CURVE ( 'NONE', #26305, #15887, #5820, .T. ) ;
#24433 = DIRECTION ( 'NONE',  ( -0.8746197071393925215, 0.4848096202463429982, 8.676864087101709653E-18 ) ) ;
#24434 = CARTESIAN_POINT ( 'NONE',  ( 52.00224528769592780, -5.936959954202218448, -13.39898132534822395 ) ) ;
#24435 = DIRECTION ( 'NONE',  ( 0.000000000000000000, -0.000000000000000000, -1.000000000000000000 ) ) ;
#24436 = ADVANCED_FACE ( 'NONE', ( #13167 ), #7391, .T. ) ;
#24437 = AXIS2_PLACEMENT_3D ( 'NONE', #26172, #748, #28328 ) ;
#24438 = EDGE_LOOP ( 'NONE', ( #16506, #17214, #13744, #3878, #10698 ) ) ;
#24439 = CARTESIAN_POINT ( 'NONE',  ( -40.23672901771082877, 7.760455916344220384, 34.54930799450052348 ) ) ;
#24440 = LINE ( 'NONE', #17210, #17041 ) ;
#24441 = CARTESIAN_POINT ( 'NONE',  ( -40.05987053574653345, 7.506472619680472746, 38.70582007960419446 ) ) ;
#24442 = EDGE_CURVE ( 'NONE', #31760, #17055, #24145, .T. ) ;
#24443 = ORIENTED_EDGE ( 'NONE', *, *, #11928, .F. ) ;
#24444 = VERTEX_POINT ( 'NONE', #27932 ) ;
#24445 =( NAMED_UNIT ( * ) SI_UNIT ( $, .STERADIAN. ) SOLID_ANGLE_UNIT ( ) );
#24446 = EDGE_CURVE ( 'NONE', #21006, #18493, #30988, .T. ) ;
#24447 = EDGE_LOOP ( 'NONE', ( #29954, #22539, #19105, #11472 ) ) ;
#24448 = PLANE ( 'NONE',  #30757 ) ;
#24449 = CARTESIAN_POINT ( 'NONE',  ( 21.09785597605719332, 44.06454579224779877, 47.04930799450051637 ) ) ;
#24450 = DIRECTION ( 'NONE',  ( 0.000000000000000000, -1.000000000000000000, 0.000000000000000000 ) ) ;
#24451 = CARTESIAN_POINT ( 'NONE',  ( -39.81510167530662159, 8.701012637326792643, 39.46050754198200394 ) ) ;
#24452 = DIRECTION ( 'NONE',  ( 0.000000000000000000, 0.000000000000000000, 1.000000000000000000 ) ) ;
#24453 = ORIENTED_EDGE ( 'NONE', *, *, #25972, .F. ) ;
#24454 = VERTEX_POINT ( 'NONE', #8237 ) ;
#24455 = FACE_OUTER_BOUND ( 'NONE', #19735, .T. ) ;
#24456 = VECTOR ( 'NONE', #8686, 1000.000000000000000 ) ;
#24457 = EDGE_CURVE ( 'NONE', #15237, #17902, #14747, .T. ) ;
#24458 = CARTESIAN_POINT ( 'NONE',  ( 46.04844006429464542, 22.86454579224779948, 44.99211097489548905 ) ) ;
#24459 = CARTESIAN_POINT ( 'NONE',  ( 21.09785597605720042, -16.63545420775220407, 47.04930799450051637 ) ) ;
#24460 = ORIENTED_EDGE ( 'NONE', *, *, #9416, .F. ) ;
#24461 = CARTESIAN_POINT ( 'NONE',  ( -6.840663840071563584, 8.583949016299408541, -4.360699202176528289 ) ) ;
#24462 = DIRECTION ( 'NONE',  ( -0.8746197071393925215, 0.4848096202463429982, 8.676864087101708112E-18 ) ) ;
#24463 = VERTEX_POINT ( 'NONE', #15778 ) ;
#24464 = CARTESIAN_POINT ( 'NONE',  ( 21.09992658989238734, 31.46664230456641675, 47.04930799450051637 ) ) ;
#24465 = CYLINDRICAL_SURFACE ( 'NONE', #450, 12.62506659569710266 ) ;
#24466 = EDGE_CURVE ( 'NONE', #24759, #2133, #5453, .T. ) ;
#24467 = AXIS2_PLACEMENT_3D ( 'NONE', #12648, #22143, #17059 ) ;
#24468 = DIRECTION ( 'NONE',  ( -1.000000000000000000, 0.000000000000000000, 0.000000000000000000 ) ) ;
#24469 = ORIENTED_EDGE ( 'NONE', *, *, #20268, .T. ) ;
#24470 = EDGE_CURVE ( 'NONE', #19118, #20658, #28873, .T. ) ;
#24471 = PLANE ( 'NONE',  #13862 ) ;
#24472 = CIRCLE ( 'NONE', #20805, 67.18681090792858868 ) ;
#24473 = CARTESIAN_POINT ( 'NONE',  ( 21.09992658989239089, 26.22145308207318593, 47.04930799450051637 ) ) ;
#24474 = CARTESIAN_POINT ( 'NONE',  ( 45.28286642839709231, 25.68619643316632306, 47.97516931882780966 ) ) ;
#24475 = ADVANCED_FACE ( 'NONE', ( #23488 ), #23329, .F. ) ;
#24476 = EDGE_LOOP ( 'NONE', ( #12272, #2179, #24729, #17948, #12439, #26472 ) ) ;
#24477 = DIRECTION ( 'NONE',  ( -7.588956326749211550E-18, 4.206627182996912454E-18, -1.000000000000000000 ) ) ;
#24478 = DIRECTION ( 'NONE',  ( -0.4848096202462977566, -0.8746197071394176126, 0.000000000000000000 ) ) ;
#24479 = CARTESIAN_POINT ( 'NONE',  ( 54.58813758245922543, -3.977894809549914257, -8.278115739697286202 ) ) ;
#24480 = ADVANCED_FACE ( 'NONE', ( #5292 ), #8439, .T. ) ;
#24481 = DIRECTION ( 'NONE',  ( -0.000000000000000000, 1.000000000000000000, -0.000000000000000000 ) ) ;
#24482 = EDGE_CURVE ( 'NONE', #2557, #10177, #15769, .T. ) ;
#24483 = CARTESIAN_POINT ( 'NONE',  ( 21.09992658989239089, 30.09184655352422411, 47.04930799450051637 ) ) ;
#24484 = CARTESIAN_POINT ( 'NONE',  ( -40.02540636251514172, 2.839176264122877047, 57.04930799450051637 ) ) ;
#24485 = FACE_OUTER_BOUND ( 'NONE', #20883, .T. ) ;
#24486 = DIRECTION ( 'NONE',  ( 0.000000000000000000, 0.000000000000000000, -1.000000000000000000 ) ) ;
#24487 = B_SPLINE_SURFACE_WITH_KNOTS ( 'NONE', 3, 1, ( 
 ( #5135, #27124 ),
 ( #19896, #22690 ),
 ( #9740, #7443 ),
 ( #4642, #12703 ),
 ( #19730, #14663 ),
 ( #24494, #17437 ) ),
 .UNSPECIFIED., .F., .F., .F.,
 ( 4, 1, 1, 4 ),
 ( 2, 2 ),
 ( 0.1800733115436725096, 0.3950736110976382220, 0.6810807126490734387, 1.000000000000000000 ),
 ( 0.000000000000000000, 1.000000000000000000 ),
 .UNSPECIFIED. ) ;
#24488 = CARTESIAN_POINT ( 'NONE',  ( 21.09992658989238734, 38.56284415653841791, 47.04930799450051637 ) ) ;
#24489 = ORIENTED_EDGE ( 'NONE', *, *, #11824, .F. ) ;
#24490 = CYLINDRICAL_SURFACE ( 'NONE', #5030, 0.7928932188134565351 ) ;
#24491 = CARTESIAN_POINT ( 'NONE',  ( 49.70056603649367588, 24.90621246473837047, 47.18448000306445067 ) ) ;
#24492 = CARTESIAN_POINT ( 'NONE',  ( -29.53813221254135968, 7.610385968504705723, 18.25503064196351843 ) ) ;
#24493 = AXIS2_PLACEMENT_3D ( 'NONE', #31360, #18540, #28573 ) ;
#24494 = CARTESIAN_POINT ( 'NONE',  ( 80.85108986838919520, 9.702389020015065313, 73.75010705023588287 ) ) ;
#24495 = ORIENTED_EDGE ( 'NONE', *, *, #10165, .F. ) ;
#24496 = DIRECTION ( 'NONE',  ( -1.000000000000000000, 0.000000000000000000, 0.000000000000000000 ) ) ;
#24497 = DIRECTION ( 'NONE',  ( 0.000000000000000000, 0.000000000000000000, -1.000000000000000000 ) ) ;
#24498 = DIRECTION ( 'NONE',  ( -1.000000000000000000, 0.000000000000000000, 0.000000000000000000 ) ) ;
#24499 = ORIENTED_EDGE ( 'NONE', *, *, #31062, .T. ) ;
#24500 = ORIENTED_EDGE ( 'NONE', *, *, #19704, .T. ) ;
#24501 = FACE_OUTER_BOUND ( 'NONE', #27553, .T. ) ;
#24502 = CARTESIAN_POINT ( 'NONE',  ( 44.70507715278255745, 29.14951373492759146, 46.92503878583764987 ) ) ;
#24503 = AXIS2_PLACEMENT_3D ( 'NONE', #22029, #29759, #31736 ) ;
#24504 = VECTOR ( 'NONE', #3754, 1000.000000000000227 ) ;
#24505 = CARTESIAN_POINT ( 'NONE',  ( 56.35714053840848692, -3.295808585244882849, 97.45038561958638468 ) ) ;
#24506 = ORIENTED_EDGE ( 'NONE', *, *, #32176, .F. ) ;
#24507 = CARTESIAN_POINT ( 'NONE',  ( 72.15675507252800003, 11.55977609614115664, 23.89582598614757103 ) ) ;
#24508 = VECTOR ( 'NONE', #397, 1000.000000000000000 ) ;
#24509 = VERTEX_POINT ( 'NONE', #18072 ) ;
#24510 = AXIS2_PLACEMENT_3D ( 'NONE', #8939, #21081, #8769 ) ;
#24511 = ORIENTED_EDGE ( 'NONE', *, *, #126, .F. ) ;
#24512 = ADVANCED_FACE ( 'NONE', ( #7749 ), #14718, .T. ) ;
#24513 = DIRECTION ( 'NONE',  ( -0.000000000000000000, -1.000000000000000000, -0.000000000000000000 ) ) ;
#24514 = EDGE_LOOP ( 'NONE', ( #24521, #9642, #22941, #1537 ) ) ;
#24515 = DIRECTION ( 'NONE',  ( -1.000000000000000000, -1.101824276508909764E-16, 0.000000000000000000 ) ) ;
#24516 = CARTESIAN_POINT ( 'NONE',  ( -30.22711675696656286, 4.712813290757158491, 77.84736881414806930 ) ) ;
#24517 = CARTESIAN_POINT ( 'NONE',  ( 21.09785597605719687, 40.56454579224780588, 17.04930799450051637 ) ) ;
#24518 = AXIS2_PLACEMENT_3D ( 'NONE', #6586, #14791, #4774 ) ;
#24519 = AXIS2_PLACEMENT_3D ( 'NONE', #8465, #15852, #18462 ) ;
#24520 = ADVANCED_FACE ( 'NONE', ( #17748 ), #8081, .F. ) ;
#24521 = ORIENTED_EDGE ( 'NONE', *, *, #31648, .T. ) ;
#24522 = CYLINDRICAL_SURFACE ( 'NONE', #25962, 19.00000000000000000 ) ;
#24523 = ORIENTED_EDGE ( 'NONE', *, *, #14987, .F. ) ;
#24524 = AXIS2_PLACEMENT_3D ( 'NONE', #19070, #6130, #15981 ) ;
#24525 = CARTESIAN_POINT ( 'NONE',  ( -40.68997348041997952, 6.796928795907699161, 60.44930799450051495 ) ) ;
#24526 = AXIS2_PLACEMENT_3D ( 'NONE', #14985, #12701, #22689 ) ;
#24527 = CARTESIAN_POINT ( 'NONE',  ( 21.09992658989238734, 38.56284415653841791, 47.04930799450051637 ) ) ;
#24528 = CARTESIAN_POINT ( 'NONE',  ( -43.72819403793993587, 1.315833819094414769, 39.54930799450052348 ) ) ;
#24529 = EDGE_LOOP ( 'NONE', ( #1689, #7582, #6321, #3281 ) ) ;
#24530 = CARTESIAN_POINT ( 'NONE',  ( -42.66751614955960292, 15.14923148629343608, 35.54930799450051637 ) ) ;
#24531 = FACE_OUTER_BOUND ( 'NONE', #11723, .T. ) ;
#24532 = LINE ( 'NONE', #2051, #21546 ) ;
#24533 = DIRECTION ( 'NONE',  ( 0.000000000000000000, 0.000000000000000000, 1.000000000000000000 ) ) ;
#24534 = FACE_OUTER_BOUND ( 'NONE', #20042, .T. ) ;
#24535 = TOROIDAL_SURFACE ( 'NONE', #19296, 13.50178401536290806, 0.5000000000000002220 ) ;
#24536 = CARTESIAN_POINT ( 'NONE',  ( 33.50134396954526039, 25.59164230456639899, 47.04930799450051637 ) ) ;
#24537 = CARTESIAN_POINT ( 'NONE',  ( 21.09785597605720753, -5.098646251524523443, 47.04930799450052348 ) ) ;
#24538 = VERTEX_POINT ( 'NONE', #26550 ) ;
#24539 = CARTESIAN_POINT ( 'NONE',  ( 21.09785597605720753, -5.098646251524523443, 47.04930799450052348 ) ) ;
#24540 = DIRECTION ( 'NONE',  ( -0.000000000000000000, -1.000000000000000000, -0.000000000000000000 ) ) ;
#24541 = ORIENTED_EDGE ( 'NONE', *, *, #17860, .T. ) ;
#24542 = CARTESIAN_POINT ( 'NONE',  ( -45.72330504332160217, -5.935454207752198563, 54.04930799450053058 ) ) ;
#24543 = CARTESIAN_POINT ( 'NONE',  ( 21.09785597605720397, -15.93545420775219945, 119.5493079945004808 ) ) ;
#24544 = ORIENTED_EDGE ( 'NONE', *, *, #626, .F. ) ;
#24545 = EDGE_LOOP ( 'NONE', ( #14108, #6433, #7212, #15500 ) ) ;
#24546 = AXIS2_PLACEMENT_3D ( 'NONE', #12547, #20081, #19914 ) ;
#24547 = CIRCLE ( 'NONE', #11448, 0.1000000000000018235 ) ;
#24548 = CIRCLE ( 'NONE', #9348, 43.00000000000000000 ) ;
#24549 = ORIENTED_EDGE ( 'NONE', *, *, #19402, .F. ) ;
#24550 = AXIS2_PLACEMENT_3D ( 'NONE', #18872, #28263, #28584 ) ;
#24551 = AXIS2_PLACEMENT_3D ( 'NONE', #3955, #18552, #13977 ) ;
#24552 = CARTESIAN_POINT ( 'NONE',  ( 21.09785597605719332, 14.86454579224779771, 47.04930799450051637 ) ) ;
#24553 = EDGE_CURVE ( 'NONE', #12894, #32314, #19953, .T. ) ;
#24554 = ORIENTED_EDGE ( 'NONE', *, *, #19749, .T. ) ;
#24555 = ORIENTED_EDGE ( 'NONE', *, *, #20971, .F. ) ;
#24556 = FACE_OUTER_BOUND ( 'NONE', #20908, .T. ) ;
#24557 = EDGE_CURVE ( 'NONE', #7034, #26728, #18988, .T. ) ;
#24558 = ADVANCED_FACE ( 'NONE', ( #1767 ), #19484, .T. ) ;
#24559 = CARTESIAN_POINT ( 'NONE',  ( 21.09785597605719332, -19.93545420775220123, 131.3493079945005491 ) ) ;
#24560 = ADVANCED_FACE ( 'NONE', ( #24410 ), #4760, .F. ) ;
#24561 = CARTESIAN_POINT ( 'NONE',  ( -40.16174044770769314, 7.468546898574136783, 53.54930799450051637 ) ) ;
#24562 = FACE_OUTER_BOUND ( 'NONE', #27191, .T. ) ;
#24563 = EDGE_CURVE ( 'NONE', #2124, #21917, #6872, .T. ) ;
#24564 = CARTESIAN_POINT ( 'NONE',  ( 21.09785597605720042, 15.56454579224779877, 96.02477317163219084 ) ) ;
#24565 = VERTEX_POINT ( 'NONE', #11024 ) ;
#24566 = CARTESIAN_POINT ( 'NONE',  ( 21.09785597605719332, 11.92558985988973497, 47.04930799450051637 ) ) ;
#24567 = ORIENTED_EDGE ( 'NONE', *, *, #20338, .F. ) ;
#24568 = CARTESIAN_POINT ( 'NONE',  ( -8.545635354592475252, 6.496515553941723198, -3.810470283972227978 ) ) ;
#24569 = PRESENTATION_LAYER_ASSIGNMENT (  '', '', ( #19864 ) ) ;
#24570 = ORIENTED_EDGE ( 'NONE', *, *, #20800, .F. ) ;
#24571 = CARTESIAN_POINT ( 'NONE',  ( -40.70508238852950456, 9.491303552449114278, 34.64930799450052490 ) ) ;
#24572 = CARTESIAN_POINT ( 'NONE',  ( 8.474859994195286461, 27.09143805560860940, 47.04930799450051637 ) ) ;
#24573 = AXIS2_PLACEMENT_3D ( 'NONE', #22209, #10081, #29771 ) ;
#24574 = CARTESIAN_POINT ( 'NONE',  ( 21.09785597605719332, 25.76454579224776964, 47.04930799450051637 ) ) ;
#24575 = CARTESIAN_POINT ( 'NONE',  ( 21.09785597605719332, 25.56454579224779167, 78.34930799450054906 ) ) ;
#24576 = CARTESIAN_POINT ( 'NONE',  ( 21.09992658989239089, 25.71664230456640254, 47.04930799450051637 ) ) ;
#24577 = AXIS2_PLACEMENT_3D ( 'NONE', #20988, #6382, #8525 ) ;
#24578 = CARTESIAN_POINT ( 'NONE',  ( 45.46000861347822308, 26.07287913140504543, 49.57397645940629616 ) ) ;
#24579 = CARTESIAN_POINT ( 'NONE',  ( 46.99747725352182925, 22.88065857334294861, 48.98207832244369087 ) ) ;
#24580 = CARTESIAN_POINT ( 'NONE',  ( -40.90015969217747482, 8.955334253785162346, 57.95249952744806166 ) ) ;
#24581 = ORIENTED_EDGE ( 'NONE', *, *, #17570, .T. ) ;
#24582 = DIRECTION ( 'NONE',  ( -1.101824276508909887E-16, 1.000000000000000000, -0.000000000000000000 ) ) ;
#24583 = DIRECTION ( 'NONE',  ( 0.4848096202463425541, 0.8746197071393929656, -2.220446049250313081E-16 ) ) ;
#24584 = DIRECTION ( 'NONE',  ( 0.4544104193609903586, 0.000000000000000000, 0.8907924397839087627 ) ) ;
#24585 = AXIS2_PLACEMENT_3D ( 'NONE', #8053, #18046, #27907 ) ;
#24586 = DIRECTION ( 'NONE',  ( 0.2756373558169942228, -0.9612616959383203374, 0.000000000000000000 ) ) ;
#24587 = DIRECTION ( 'NONE',  ( -1.224646799147353207E-16, -1.349345573449484691E-32, 1.000000000000000000 ) ) ;
#24588 = EDGE_LOOP ( 'NONE', ( #17242, #32360, #2456, #6509 ) ) ;
#24589 = VERTEX_POINT ( 'NONE', #21012 ) ;
#24590 = CARTESIAN_POINT ( 'NONE',  ( 21.09992658989239089, 24.47145308207319303, 47.04930799450051637 ) ) ;
#24591 = ORIENTED_EDGE ( 'NONE', *, *, #27993, .T. ) ;
#24592 = ADVANCED_FACE ( 'NONE', ( #6862 ), #26877, .T. ) ;
#24593 = CIRCLE ( 'NONE', #25653, 1.000000000000000000 ) ;
#24594 = CIRCLE ( 'NONE', #16197, 12.36707279061065101 ) ;
#24595 =( BOUNDED_SURFACE ( )  B_SPLINE_SURFACE ( 3, 2, ( 
 ( #25805, #3148, #20555, #7939, #856, #25331, #30745, #25488, #23347, #2989, #17934, #10724, #23016, #22857, #8253, #30586, #18239, #12868, #28120, #3316, #10393, #15477, #5625, #20391, #23184, #28273, #30422, #5473, #535, #5795, #13023, #15626, #20872, #10566, #13346, #15799, #25646, #13193, #10881, #20719, #22307, #15089, #27403, #15252, #10172, #20005, #7387, #20320, #17381, #5407, #19839, #30193, #15410, #27229, #14929, #10009, #25422, #12802, #2930, #25101, #2776, #24941, #10330, #7704, #17699, #9680, #29705, #2455, #12306, #22138, #17546, #27725, #5243, #22792, #19676, #30353, #17212, #7549, #27891, #32167, #14772, #22629, #7211, #152, #12473 ),
 ( #4756, #25263, #309, #24774, #32332, #7871, #2290, #9840, #17873, #29870, #4918, #22459, #32493, #30036, #27563, #5078, #2612, #12641, #20168, #16049, #3084, #25578, #20494, #18181, #796, #3415, #28534, #16203, #11141, #10496, #30521, #13292, #8038, #28050, #5893, #23440, #6050, #28683, #20813, #13122, #18026, #6198, #10822, #18662, #5565, #12961, #21124, #31158, #26220, #23284, #15565, #20655, #8192, #30836, #8672, #31000, #28211, #15899, #8347, #18346, #28376, #22945, #23119, #25903, #8512, #637, #13445, #10668, #949, #10976, #20972, #30680, #18506, #26054, #469, #5726, #15731, #3570, #25746, #3255, #13596, #23601, #1116, #7010, #18979 ),
 ( #6528, #9478, #21609, #26702, #31958, #26870, #13762, #24075, #17005, #21284, #4226, #3736, #29011, #13921, #16851, #9145, #1263, #16678, #3897, #29170, #8985, #29329, #24240, #1591, #21442, #1914, #31476, #19475, #1428, #11775, #29506, #8817, #16524, #11614, #23757, #4383, #11294, #6684, #14402, #26544, #24400, #21769, #31796, #31317, #18814, #4053, #26388, #28853, #31642, #9307, #19304, #11934, #6365, #21930, #16364, #19143, #23917, #11444, #14079, #14243, #1759, #6852, #11851, #18893, #28929, #6438, #14481, #14316, #16756, #1992, #31387, #29411, #24474, #12011, #19384, #16440, #18723, #6273, #26297, #31870, #1501, #22005, #31555, #13832, #26780 ),
 ( #23987, #21846, #8732, #1344, #11517, #28758, #26615, #31713, #4461, #9385, #16277, #29083, #3806, #23828, #9224, #11361, #21517, #26458, #6922, #14152, #21347, #21684, #8896, #1670, #13995, #1834, #29240, #6601, #3973, #16921, #9058, #19052, #16595, #4297, #4129, #24150, #11692, #19215, #6758, #26943, #24315, #24969, #12676, #24810, #20205, #7580, #17579, #19545, #7086, #2326, #22173, #12835, #27436, #27595, #5109, #185, #29576, #7737, #27102, #17416, #5280, #32036, #24644, #24, #9554, #10043, #15124, #14967, #25135, #4787, #4618, #7420, #2649, #14640, #22666, #10204, #17086, #30227, #22494, #9874, #12180, #25299, #2164, #17735, #29738 ) ),
 .UNSPECIFIED., .F., .F., .F. ) 
 B_SPLINE_SURFACE_WITH_KNOTS ( ( 4, 4 ),
 ( 3, 2, 2, 2, 2, 2, 2, 2, 2, 2, 2, 2, 2, 2, 2, 2, 2, 2, 2, 2, 2, 2, 2, 2, 2, 2, 2, 2, 2, 2, 2, 2, 2, 2, 2, 2, 2, 2, 2, 2, 2, 2, 3 ),
 ( 0.000000000000000000, 1.000000000000000000 ),
 ( 0.000000000000000000, 0.02380952380952380820, 0.04761904761904761640, 0.07142857142857142461, 0.09523809523809523281, 0.1190476190476190410, 0.1428571428571428492, 0.1666666666666666574, 0.1904761904761904656, 0.2142857142857142738, 0.2380952380952380820, 0.2619047619047619180, 0.2857142857142856984, 0.3095238095238095344, 0.3333333333333333148, 0.3571428571428571508, 0.3809523809523809312, 0.4047619047619047672, 0.4285714285714285476, 0.4523809523809523836, 0.4761904761904761640, 0.5000000000000000000, 0.5238095238095238360, 0.5476190476190476719, 0.5714285714285713969, 0.5952380952380952328, 0.6190476190476190688, 0.6428571428571429047, 0.6666666666666666297, 0.6904761904761904656, 0.7142857142857143016, 0.7380952380952381375, 0.7619047619047618625, 0.7857142857142856984, 0.8095238095238095344, 0.8333333333333333703, 0.8571428571428570953, 0.8809523809523809312, 0.9047619047619047672, 0.9285714285714286031, 0.9523809523809523281, 0.9761904761904761640, 1.000000000000000000 ),
 .UNSPECIFIED. ) 
 GEOMETRIC_REPRESENTATION_ITEM ( )  RATIONAL_B_SPLINE_SURFACE ( (
 ( 1.000000000000000000, 0.8660254037844387076, 1.000000000000000000, 0.8660254037844387076, 1.000000000000000000, 0.8660254037844387076, 1.000000000000000000, 0.8660254037844387076, 1.000000000000000000, 0.8660254037844387076, 1.000000000000000000, 0.8660254037844387076, 1.000000000000000000, 0.8660254037844387076, 1.000000000000000000, 0.8660254037844387076, 1.000000000000000000, 0.8660254037844387076, 1.000000000000000000, 0.8660254037844387076, 1.000000000000000000, 0.8660254037844387076, 1.000000000000000000, 0.8660254037844387076, 1.000000000000000000, 0.8660254037844387076, 1.000000000000000000, 0.8660254037844387076, 1.000000000000000000, 0.8660254037844387076, 1.000000000000000000, 0.8660254037844387076, 1.000000000000000000, 0.8660254037844387076, 1.000000000000000000, 0.8660254037844387076, 1.000000000000000000, 0.8660254037844387076, 1.000000000000000000, 0.8660254037844387076, 1.000000000000000000, 0.8660254037844387076, 1.000000000000000000, 0.8660254037844387076, 1.000000000000000000, 0.8660254037844387076, 1.000000000000000000, 0.8660254037844387076, 1.000000000000000000, 0.8660254037844387076, 1.000000000000000000, 0.8660254037844387076, 1.000000000000000000, 0.8660254037844387076, 1.000000000000000000, 0.8660254037844387076, 1.000000000000000000, 0.8660254037844387076, 1.000000000000000000, 0.8660254037844387076, 1.000000000000000000, 0.8660254037844387076, 1.000000000000000000, 0.8660254037844387076, 1.000000000000000000, 0.8660254037844387076, 1.000000000000000000, 0.8660254037844387076, 1.000000000000000000, 0.8660254037844387076, 1.000000000000000000, 0.8660254037844387076, 1.000000000000000000, 0.8660254037844387076, 1.000000000000000000, 0.8660254037844387076, 1.000000000000000000, 0.8660254037844387076, 1.000000000000000000, 0.8660254037844387076, 1.000000000000000000, 0.8660254037844387076, 1.000000000000000000, 0.8660254037844387076, 1.000000000000000000),
 ( 0.6666666666666665186, 0.5773502691896257311, 0.6666666666666665186, 0.5773502691896257311, 0.6666666666666665186, 0.5773502691896257311, 0.6666666666666665186, 0.5773502691896257311, 0.6666666666666665186, 0.5773502691896257311, 0.6666666666666665186, 0.5773502691896257311, 0.6666666666666665186, 0.5773502691896257311, 0.6666666666666665186, 0.5773502691896257311, 0.6666666666666665186, 0.5773502691896257311, 0.6666666666666665186, 0.5773502691896257311, 0.6666666666666665186, 0.5773502691896257311, 0.6666666666666665186, 0.5773502691896257311, 0.6666666666666665186, 0.5773502691896257311, 0.6666666666666665186, 0.5773502691896257311, 0.6666666666666665186, 0.5773502691896257311, 0.6666666666666665186, 0.5773502691896257311, 0.6666666666666665186, 0.5773502691896257311, 0.6666666666666665186, 0.5773502691896257311, 0.6666666666666665186, 0.5773502691896257311, 0.6666666666666665186, 0.5773502691896257311, 0.6666666666666665186, 0.5773502691896257311, 0.6666666666666665186, 0.5773502691896257311, 0.6666666666666665186, 0.5773502691896257311, 0.6666666666666665186, 0.5773502691896257311, 0.6666666666666665186, 0.5773502691896257311, 0.6666666666666665186, 0.5773502691896257311, 0.6666666666666665186, 0.5773502691896257311, 0.6666666666666665186, 0.5773502691896257311, 0.6666666666666665186, 0.5773502691896257311, 0.6666666666666665186, 0.5773502691896257311, 0.6666666666666665186, 0.5773502691896257311, 0.6666666666666665186, 0.5773502691896257311, 0.6666666666666665186, 0.5773502691896257311, 0.6666666666666665186, 0.5773502691896257311, 0.6666666666666665186, 0.5773502691896257311, 0.6666666666666665186, 0.5773502691896257311, 0.6666666666666665186, 0.5773502691896257311, 0.6666666666666665186, 0.5773502691896257311, 0.6666666666666665186, 0.5773502691896257311, 0.6666666666666665186, 0.5773502691896257311, 0.6666666666666665186, 0.5773502691896257311, 0.6666666666666665186, 0.5773502691896257311, 0.6666666666666665186),
 ( 0.6666666666666665186, 0.5773502691896257311, 0.6666666666666665186, 0.5773502691896257311, 0.6666666666666665186, 0.5773502691896257311, 0.6666666666666665186, 0.5773502691896257311, 0.6666666666666665186, 0.5773502691896257311, 0.6666666666666665186, 0.5773502691896257311, 0.6666666666666665186, 0.5773502691896257311, 0.6666666666666665186, 0.5773502691896257311, 0.6666666666666665186, 0.5773502691896257311, 0.6666666666666665186, 0.5773502691896257311, 0.6666666666666665186, 0.5773502691896257311, 0.6666666666666665186, 0.5773502691896257311, 0.6666666666666665186, 0.5773502691896257311, 0.6666666666666665186, 0.5773502691896257311, 0.6666666666666665186, 0.5773502691896257311, 0.6666666666666665186, 0.5773502691896257311, 0.6666666666666665186, 0.5773502691896257311, 0.6666666666666665186, 0.5773502691896257311, 0.6666666666666665186, 0.5773502691896257311, 0.6666666666666665186, 0.5773502691896257311, 0.6666666666666665186, 0.5773502691896257311, 0.6666666666666665186, 0.5773502691896257311, 0.6666666666666665186, 0.5773502691896257311, 0.6666666666666665186, 0.5773502691896257311, 0.6666666666666665186, 0.5773502691896257311, 0.6666666666666665186, 0.5773502691896257311, 0.6666666666666665186, 0.5773502691896257311, 0.6666666666666665186, 0.5773502691896257311, 0.6666666666666665186, 0.5773502691896257311, 0.6666666666666665186, 0.5773502691896257311, 0.6666666666666665186, 0.5773502691896257311, 0.6666666666666665186, 0.5773502691896257311, 0.6666666666666665186, 0.5773502691896257311, 0.6666666666666665186, 0.5773502691896257311, 0.6666666666666665186, 0.5773502691896257311, 0.6666666666666665186, 0.5773502691896257311, 0.6666666666666665186, 0.5773502691896257311, 0.6666666666666665186, 0.5773502691896257311, 0.6666666666666665186, 0.5773502691896257311, 0.6666666666666665186, 0.5773502691896257311, 0.6666666666666665186, 0.5773502691896257311, 0.6666666666666665186, 0.5773502691896257311, 0.6666666666666665186),
 ( 1.000000000000000000, 0.8660254037844387076, 1.000000000000000000, 0.8660254037844387076, 1.000000000000000000, 0.8660254037844387076, 1.000000000000000000, 0.8660254037844387076, 1.000000000000000000, 0.8660254037844387076, 1.000000000000000000, 0.8660254037844387076, 1.000000000000000000, 0.8660254037844387076, 1.000000000000000000, 0.8660254037844387076, 1.000000000000000000, 0.8660254037844387076, 1.000000000000000000, 0.8660254037844387076, 1.000000000000000000, 0.8660254037844387076, 1.000000000000000000, 0.8660254037844387076, 1.000000000000000000, 0.8660254037844387076, 1.000000000000000000, 0.8660254037844387076, 1.000000000000000000, 0.8660254037844387076, 1.000000000000000000, 0.8660254037844387076, 1.000000000000000000, 0.8660254037844387076, 1.000000000000000000, 0.8660254037844387076, 1.000000000000000000, 0.8660254037844387076, 1.000000000000000000, 0.8660254037844387076, 1.000000000000000000, 0.8660254037844387076, 1.000000000000000000, 0.8660254037844387076, 1.000000000000000000, 0.8660254037844387076, 1.000000000000000000, 0.8660254037844387076, 1.000000000000000000, 0.8660254037844387076, 1.000000000000000000, 0.8660254037844387076, 1.000000000000000000, 0.8660254037844387076, 1.000000000000000000, 0.8660254037844387076, 1.000000000000000000, 0.8660254037844387076, 1.000000000000000000, 0.8660254037844387076, 1.000000000000000000, 0.8660254037844387076, 1.000000000000000000, 0.8660254037844387076, 1.000000000000000000, 0.8660254037844387076, 1.000000000000000000, 0.8660254037844387076, 1.000000000000000000, 0.8660254037844387076, 1.000000000000000000, 0.8660254037844387076, 1.000000000000000000, 0.8660254037844387076, 1.000000000000000000, 0.8660254037844387076, 1.000000000000000000, 0.8660254037844387076, 1.000000000000000000, 0.8660254037844387076, 1.000000000000000000, 0.8660254037844387076, 1.000000000000000000, 0.8660254037844387076, 1.000000000000000000) ) ) 
 REPRESENTATION_ITEM ( '' )  SURFACE ( )  );
#24596 = ORIENTED_EDGE ( 'NONE', *, *, #2072, .T. ) ;
#24597 = FACE_OUTER_BOUND ( 'NONE', #17050, .T. ) ;
#24598 = CARTESIAN_POINT ( 'NONE',  ( 51.92400919103563695, -5.935454207752202116, -12.70392589783158499 ) ) ;
#24599 = CARTESIAN_POINT ( 'NONE',  ( 21.09785597605717911, -12.82881809906321813, 103.0103621606812681 ) ) ;
#24600 = CIRCLE ( 'NONE', #11003, 56.65825807113184709 ) ;
#24601 = CIRCLE ( 'NONE', #9429, 0.1250000000000001110 ) ;
#24602 = EDGE_LOOP ( 'NONE', ( #4353, #12616, #19277, #22723 ) ) ;
#24603 = EDGE_CURVE ( 'NONE', #3439, #2858, #18888, .T. ) ;
#24604 = DIRECTION ( 'NONE',  ( -1.101824276508909887E-16, 1.000000000000000000, -0.000000000000000000 ) ) ;
#24605 = ADVANCED_FACE ( 'NONE', ( #9487 ), #12096, .T. ) ;
#24606 = CIRCLE ( 'NONE', #5224, 43.00000000000000000 ) ;
#24607 = LINE ( 'NONE', #2126, #14436 ) ;
#24608 = ADVANCED_FACE ( 'NONE', ( #26710 ), #19151, .F. ) ;
#24609 = AXIS2_PLACEMENT_3D ( 'NONE', #21542, #28784, #1053 ) ;
#24610 = ORIENTED_EDGE ( 'NONE', *, *, #3519, .T. ) ;
#24611 = ORIENTED_EDGE ( 'NONE', *, *, #8848, .T. ) ;
#24612 = DIRECTION ( 'NONE',  ( -1.101824276508909887E-16, 1.000000000000000000, -0.000000000000000000 ) ) ;
#24613 = ORIENTED_EDGE ( 'NONE', *, *, #5423, .F. ) ;
#24614 = CARTESIAN_POINT ( 'NONE',  ( 21.09785597605720753, 13.86454579224779948, 47.04930799450052348 ) ) ;
#24615 = DIRECTION ( 'NONE',  ( -7.588956326749211550E-18, 4.206627182996911684E-18, -1.000000000000000000 ) ) ;
#24616 = CYLINDRICAL_SURFACE ( 'NONE', #19503, 12.62506659569710443 ) ;
#24617 = CARTESIAN_POINT ( 'NONE',  ( 21.09992658989239089, 26.84164230456639899, 47.04930799450051637 ) ) ;
#24618 = CARTESIAN_POINT ( 'NONE',  ( 48.18662509608405031, 28.59624452788247950, 49.18364984542562013 ) ) ;
#24619 = DIRECTION ( 'NONE',  ( 0.000000000000000000, 0.000000000000000000, 1.000000000000000000 ) ) ;
#24620 = ORIENTED_EDGE ( 'NONE', *, *, #14901, .T. ) ;
#24621 = VERTEX_POINT ( 'NONE', #24572 ) ;
#24622 = CARTESIAN_POINT ( 'NONE',  ( 100.3079064823960493, -16.63545420775219696, 47.04930799450134771 ) ) ;
#24623 = AXIS2_PLACEMENT_3D ( 'NONE', #17301, #12231, #9769 ) ;
#24624 = FACE_OUTER_BOUND ( 'NONE', #24182, .T. ) ;
#24625 = CARTESIAN_POINT ( 'NONE',  ( 21.09785597605719332, -16.63545420775219696, 128.7593585008393973 ) ) ;
#24626 = ORIENTED_EDGE ( 'NONE', *, *, #13391, .T. ) ;
#24627 = CARTESIAN_POINT ( 'NONE',  ( -10.54383519688239090, 3.260977705924062775, -5.641619965526164293 ) ) ;
#24628 = CARTESIAN_POINT ( 'NONE',  ( 50.27680291267451906, -13.74047052604243468, 97.57784857907853393 ) ) ;
#24629 = ORIENTED_EDGE ( 'NONE', *, *, #4705, .F. ) ;
#24630 = CARTESIAN_POINT ( 'NONE',  ( 8.474859994195286461, 25.09143805560860940, 47.04930799450051637 ) ) ;
#24631 = CARTESIAN_POINT ( 'NONE',  ( 21.09785597605720753, 17.36467600858027183, 47.04930799450052348 ) ) ;
#24632 = AXIS2_PLACEMENT_3D ( 'NONE', #27039, #27533, #9975 ) ;
#24633 = CIRCLE ( 'NONE', #12608, 55.62393233686778160 ) ;
#24634 = CARTESIAN_POINT ( 'NONE',  ( 42.59785597605720397, 14.86454579224779948, 47.04930799450052348 ) ) ;
#24635 = VECTOR ( 'NONE', #17427, 1000.000000000000000 ) ;
#24636 = VECTOR ( 'NONE', #25390, 1000.000000000000000 ) ;
#24637 = VECTOR ( 'NONE', #20072, 1000.000000000000227 ) ;
#24638 = EDGE_CURVE ( 'NONE', #25249, #3392, #13497, .T. ) ;
#24639 = EDGE_CURVE ( 'NONE', #17931, #10875, #31496, .T. ) ;
#24640 = ORIENTED_EDGE ( 'NONE', *, *, #4828, .T. ) ;
#24641 = ORIENTED_EDGE ( 'NONE', *, *, #9950, .T. ) ;
#24642 = CARTESIAN_POINT ( 'NONE',  ( 21.09785597605719332, 45.28940914544685370, 69.74790822305027405 ) ) ;
#24643 = CARTESIAN_POINT ( 'NONE',  ( 21.09992658989238734, 32.46183152705962272, 47.04930799450051637 ) ) ;
#24644 = CARTESIAN_POINT ( 'NONE',  ( 45.35708200440645044, 26.29118040159426428, 45.92000246470679770 ) ) ;
#24645 = AXIS2_PLACEMENT_3D ( 'NONE', #27114, #17589, #4631 ) ;
#24646 = ORIENTED_EDGE ( 'NONE', *, *, #2924, .F. ) ;
#24647 = CARTESIAN_POINT ( 'NONE',  ( 33.50134396954521776, 29.34164230456639899, 47.04930799450051637 ) ) ;
#24648 = DIRECTION ( 'NONE',  ( -1.000000000000000000, 0.000000000000000000, 0.000000000000000000 ) ) ;
#24649 = ADVANCED_FACE ( 'NONE', ( #21778 ), #1601, .T. ) ;
#24650 = CIRCLE ( 'NONE', #19915, 12.36707279061065101 ) ;
#24651 = CIRCLE ( 'NONE', #20460, 0.1250000000000001110 ) ;
#24652 = DIRECTION ( 'NONE',  ( -1.101824276508909887E-16, 1.000000000000000000, -0.000000000000000000 ) ) ;
#24653 = DIRECTION ( 'NONE',  ( 0.000000000000000000, -1.000000000000000000, 0.000000000000000000 ) ) ;
#24654 = CARTESIAN_POINT ( 'NONE',  ( -11.40214402394279603, 13.86454579224779948, 47.04930799450052348 ) ) ;
#24655 = FACE_OUTER_BOUND ( 'NONE', #30491, .T. ) ;
#24656 = CARTESIAN_POINT ( 'NONE',  ( -42.21195563036362586, 4.051200314738734320, 55.04930799450051637 ) ) ;
#24657 = AXIS2_PLACEMENT_3D ( 'NONE', #22468, #6111, #2621 ) ;
#24658 = LINE ( 'NONE', #8784, #23844 ) ;
#24659 = CARTESIAN_POINT ( 'NONE',  ( -41.01929587258828036, 9.401204285752060130, 34.64930799450051779 ) ) ;
#24660 = AXIS2_PLACEMENT_3D ( 'NONE', #16977, #32100, #4358 ) ;
#24661 = ORIENTED_EDGE ( 'NONE', *, *, #25244, .F. ) ;
#24662 = AXIS2_PLACEMENT_3D ( 'NONE', #27299, #1862, #9414 ) ;
#24663 = DIRECTION ( 'NONE',  ( -0.8746197071393926326, 0.4848096202463430537, 8.676864087101709653E-18 ) ) ;
#24664 = AXIS2_PLACEMENT_3D ( 'NONE', #23894, #31291, #4032 ) ;
#24665 = CARTESIAN_POINT ( 'NONE',  ( 49.92650180258424086, 24.88153309617948139, 45.60636096795945349 ) ) ;
#24666 = CARTESIAN_POINT ( 'NONE',  ( -30.07837276871502752, 5.259395908821971055, 16.59273893179034332 ) ) ;
#24667 = ORIENTED_EDGE ( 'NONE', *, *, #3851, .F. ) ;
#24668 = FACE_OUTER_BOUND ( 'NONE', #2912, .T. ) ;
#24669 = CARTESIAN_POINT ( 'NONE',  ( 21.09785597605719687, 48.06454579224779877, 66.09820277283748169 ) ) ;
#24670 = LINE ( 'NONE', #12860, #6279 ) ;
#24671 = EDGE_CURVE ( 'NONE', #2915, #8103, #32031, .T. ) ;
#24672 = VERTEX_POINT ( 'NONE', #9152 ) ;
#24673 = ORIENTED_EDGE ( 'NONE', *, *, #11571, .T. ) ;
#24674 = CARTESIAN_POINT ( 'NONE',  ( -40.11902961310586591, 6.880801488287907830, 39.52370399052030336 ) ) ;
#24675 = CARTESIAN_POINT ( 'NONE',  ( 21.09785597605718976, 1.799431449832689101, 47.04930799450051637 ) ) ;
#24676 = AXIS2_PLACEMENT_3D ( 'NONE', #18391, #13487, #10544 ) ;
#24677 = CARTESIAN_POINT ( 'NONE',  ( -9.472371843582571671, 5.388785998227650254, -12.62465409255485582 ) ) ;
#24678 = EDGE_CURVE ( 'NONE', #21924, #22032, #4245, .T. ) ;
#24679 = DIRECTION ( 'NONE',  ( -1.224646799147353207E-16, -1.349345573449484691E-32, 1.000000000000000000 ) ) ;
#24680 = CARTESIAN_POINT ( 'NONE',  ( 45.39362547348767407, 29.25948157811722083, 45.34546605000252839 ) ) ;
#24681 = VERTEX_POINT ( 'NONE', #24247 ) ;
#24682 = ADVANCED_FACE ( 'NONE', ( #27690 ), #118, .T. ) ;
#24683 = EDGE_CURVE ( 'NONE', #32232, #30206, #12645, .T. ) ;
#24684 = CIRCLE ( 'NONE', #9469, 0.1250000000000001110 ) ;
#24685 = ORIENTED_EDGE ( 'NONE', *, *, #5833, .T. ) ;
#24686 = ADVANCED_FACE ( 'NONE', ( #30166 ), #24909, .T. ) ;
#24687 = VECTOR ( 'NONE', #15907, 1000.000000000000000 ) ;
#24688 = AXIS2_PLACEMENT_3D ( 'NONE', #4624, #29743, #12184 ) ;
#24689 = DIRECTION ( 'NONE',  ( 0.9612616959383198934, 0.2756373558169956106, 0.000000000000000000 ) ) ;
#24690 = AXIS2_PLACEMENT_3D ( 'NONE', #19606, #29637, #4681 ) ;
#24691 = VERTEX_POINT ( 'NONE', #22599 ) ;
#24692 = DIRECTION ( 'NONE',  ( -1.000000000000000000, 0.000000000000000000, 0.000000000000000000 ) ) ;
#24693 = CARTESIAN_POINT ( 'NONE',  ( 21.09992658989238734, 38.56284415653841791, 47.04930799450051637 ) ) ;
#24694 = EDGE_CURVE ( 'NONE', #24565, #15433, #6318, .T. ) ;
#24695 = CONICAL_SURFACE ( 'NONE', #9515, 1.799999999999998490, 0.7853981633974489451 ) ;
#24696 = ORIENTED_EDGE ( 'NONE', *, *, #24193, .T. ) ;
#24697 = CARTESIAN_POINT ( 'NONE',  ( -40.76127908587941562, 8.436192945956459965, 34.55055826194723068 ) ) ;
#24698 = ORIENTED_EDGE ( 'NONE', *, *, #21763, .T. ) ;
#24699 = LINE ( 'NONE', #2700, #22589 ) ;
#24700 = CARTESIAN_POINT ( 'NONE',  ( 21.09785597605720042, -13.59284023713420630, 47.04930799450051637 ) ) ;
#24701 = ORIENTED_EDGE ( 'NONE', *, *, #32357, .F. ) ;
#24702 = DIRECTION ( 'NONE',  ( 0.000000000000000000, 0.000000000000000000, -1.000000000000000000 ) ) ;
#24703 = CARTESIAN_POINT ( 'NONE',  ( 21.09785597605721108, -16.73545420775220194, 125.4493079945005150 ) ) ;
#24704 = FACE_OUTER_BOUND ( 'NONE', #26299, .T. ) ;
#24705 = DIRECTION ( 'NONE',  ( -1.101824276508909887E-16, 1.000000000000000000, -0.000000000000000000 ) ) ;
#24706 = DIRECTION ( 'NONE',  ( 0.000000000000000000, -1.000000000000000000, 0.000000000000000000 ) ) ;
#24707 = ORIENTED_EDGE ( 'NONE', *, *, #23391, .T. ) ;
#24708 = AXIS2_PLACEMENT_3D ( 'NONE', #11420, #1408, #11591 ) ;
#24709 = DIRECTION ( 'NONE',  ( -0.4848096202462977566, -0.8746197071394176126, 0.000000000000000000 ) ) ;
#24710 = LINE ( 'NONE', #17802, #20109 ) ;
#24711 = ADVANCED_FACE ( 'NONE', ( #27368 ), #19432, .T. ) ;
#24712 = ORIENTED_EDGE ( 'NONE', *, *, #14359, .F. ) ;
#24713 = AXIS2_PLACEMENT_3D ( 'NONE', #5643, #10745, #27974 ) ;
#24714 = DIRECTION ( 'NONE',  ( 1.000000000000000000, -0.000000000000000000, -0.000000000000000000 ) ) ;
#24715 = AXIS2_PLACEMENT_3D ( 'NONE', #12926, #8478, #22915 ) ;
#24716 = AXIS2_PLACEMENT_3D ( 'NONE', #17673, #22921, #7839 ) ;
#24717 = ADVANCED_FACE ( 'NONE', ( #5210 ), #15256, .T. ) ;
#24718 = DIRECTION ( 'NONE',  ( -1.101824276508909887E-16, 1.000000000000000000, -0.000000000000000000 ) ) ;
#24719 = ORIENTED_EDGE ( 'NONE', *, *, #18801, .T. ) ;
#24720 = ORIENTED_EDGE ( 'NONE', *, *, #6236, .T. ) ;
#24721 = CIRCLE ( 'NONE', #17372, 0.1250000000000001110 ) ;
#24722 = EDGE_CURVE ( 'NONE', #7173, #15510, #25235, .T. ) ;
#24723 = ORIENTED_EDGE ( 'NONE', *, *, #22572, .T. ) ;
#24724 = EDGE_CURVE ( 'NONE', #3682, #7574, #32300, .T. ) ;
#24725 = AXIS2_PLACEMENT_3D ( 'NONE', #11069, #13050, #30608 ) ;
#24726 = TOROIDAL_SURFACE ( 'NONE', #22135, 0.8999999999999995781, 0.1000000000000000056 ) ;
#24727 = CARTESIAN_POINT ( 'NONE',  ( 21.09992658989239089, 23.59164230456639544, 47.04930799450051637 ) ) ;
#24728 = ORIENTED_EDGE ( 'NONE', *, *, #21782, .F. ) ;
#24729 = ORIENTED_EDGE ( 'NONE', *, *, #11761, .T. ) ;
#24730 = DIRECTION ( 'NONE',  ( 1.000000000000000000, 0.000000000000000000, 0.000000000000000000 ) ) ;
#24731 = DIRECTION ( 'NONE',  ( -1.224646799147353207E-16, -1.349345573449484691E-32, 1.000000000000000000 ) ) ;
#24732 = CARTESIAN_POINT ( 'NONE',  ( 21.09992658989238734, 38.56284415653841791, 47.04930799450051637 ) ) ;
#24733 = CARTESIAN_POINT ( 'NONE',  ( 45.96182992765471909, 15.77906836436399374, 44.82232689504101586 ) ) ;
#24734 = CARTESIAN_POINT ( 'NONE',  ( 21.09992658989239089, 30.21183152705961561, 47.04930799450051637 ) ) ;
#24735 = ORIENTED_EDGE ( 'NONE', *, *, #31083, .F. ) ;
#24736 = CARTESIAN_POINT ( 'NONE',  ( 33.46699938050304013, 32.46183152705962272, 47.04930799450051637 ) ) ;
#24737 = ORIENTED_EDGE ( 'NONE', *, *, #7821, .F. ) ;
#24738 = CARTESIAN_POINT ( 'NONE',  ( -30.57062045089658753, 7.039311848382081571, 17.81148138227357336 ) ) ;
#24739 = CARTESIAN_POINT ( 'NONE',  ( 47.09785597605719687, 24.76454579224779806, 47.04930799450078638 ) ) ;
#24740 = AXIS2_PLACEMENT_3D ( 'NONE', #6819, #9776, #16818 ) ;
#24741 = ORIENTED_EDGE ( 'NONE', *, *, #7160, .F. ) ;
#24742 = DIRECTION ( 'NONE',  ( -1.101824276508909887E-16, 1.000000000000000000, -0.000000000000000000 ) ) ;
#24743 = DIRECTION ( 'NONE',  ( -1.224646799147353207E-16, -1.349345573449484691E-32, 1.000000000000000000 ) ) ;
#24744 = CARTESIAN_POINT ( 'NONE',  ( -42.30123736278718383, 13.66041317296246937, 54.56265170360538264 ) ) ;
#24745 = CARTESIAN_POINT ( 'NONE',  ( 47.35361591473682097, 23.10527845304106265, 47.55068078453451363 ) ) ;
#24746 = CARTESIAN_POINT ( 'NONE',  ( 46.17891025898683921, 22.93807716476589675, 48.46582155994513386 ) ) ;
#24747 = TOROIDAL_SURFACE ( 'NONE', #18962, 46.75000000000000000, 0.7905694150421007649 ) ;
#24748 = CARTESIAN_POINT ( 'NONE',  ( 48.40186567930498285, 27.42957786121582231, 45.03923535223908203 ) ) ;
#24749 = CARTESIAN_POINT ( 'NONE',  ( -40.06503689199327312, 6.934220188909110405, 34.98002959068131901 ) ) ;
#24750 = DIRECTION ( 'NONE',  ( 1.234978253042719660E-16, -1.000000000000000000, -1.109335647967047851E-31 ) ) ;
#24751 = ORIENTED_EDGE ( 'NONE', *, *, #23233, .F. ) ;
#24752 = CARTESIAN_POINT ( 'NONE',  ( -38.52112853513683888, -5.935454207752202116, 16.07118271501078510 ) ) ;
#24753 = ORIENTED_EDGE ( 'NONE', *, *, #24983, .T. ) ;
#24754 = AXIS2_PLACEMENT_3D ( 'NONE', #27071, #4583, #26584 ) ;
#24755 = CYLINDRICAL_SURFACE ( 'NONE', #29490, 12.36707279061065101 ) ;
#24756 = CARTESIAN_POINT ( 'NONE',  ( -29.27337757263006424, -5.432165593243111879, 14.50875660354866703 ) ) ;
#24757 = VERTEX_POINT ( 'NONE', #9810 ) ;
#24758 = CIRCLE ( 'NONE', #31576, 25.50000000000000355 ) ;
#24759 = VERTEX_POINT ( 'NONE', #19804 ) ;
#24760 = CARTESIAN_POINT ( 'NONE',  ( 21.09785597605719332, 25.56454579224779877, 18.54930799450050927 ) ) ;
#24761 = EDGE_CURVE ( 'NONE', #16834, #11074, #23638, .T. ) ;
#24762 = ORIENTED_EDGE ( 'NONE', *, *, #25356, .F. ) ;
#24763 = PRODUCT_DEFINITION_SHAPE ( 'NONE', 'NONE',  #8511 ) ;
#24764 = ORIENTED_EDGE ( 'NONE', *, *, #12356, .F. ) ;
#24765 = AXIS2_PLACEMENT_3D ( 'NONE', #25303, #30388, #2167 ) ;
#24766 = DIRECTION ( 'NONE',  ( -0.4848096202463430537, -0.8746197071393926326, -9.920727850371701658E-18 ) ) ;
#24767 = CARTESIAN_POINT ( 'NONE',  ( 52.07152283844947505, -5.935708903123431135, -13.42846411458451428 ) ) ;
#24768 = CIRCLE ( 'NONE', #662, 0.1250000000000001110 ) ;
#24769 = ORIENTED_EDGE ( 'NONE', *, *, #14847, .T. ) ;
#24770 = DIRECTION ( 'NONE',  ( -1.000000000000000000, 0.000000000000000000, 0.000000000000000000 ) ) ;
#24771 = AXIS2_PLACEMENT_3D ( 'NONE', #20267, #27662, #7807 ) ;
#24772 = CARTESIAN_POINT ( 'NONE',  ( 8.732853799281738105, 24.46183152705960140, 47.04930799450051637 ) ) ;
#24773 = DIRECTION ( 'NONE',  ( -1.000000000000000000, 0.000000000000000000, 0.000000000000000000 ) ) ;
#24774 = CARTESIAN_POINT ( 'NONE',  ( 46.02876340639226527, 29.66789516297708929, 44.95353858666495483 ) ) ;
#24775 = ORIENTED_EDGE ( 'NONE', *, *, #860, .T. ) ;
#24776 = ORIENTED_EDGE ( 'NONE', *, *, #15663, .T. ) ;
#24777 = LINE ( 'NONE', #19024, #4836 ) ;
#24778 = ORIENTED_EDGE ( 'NONE', *, *, #29715, .T. ) ;
#24779 = CARTESIAN_POINT ( 'NONE',  ( -40.46704588662232283, 7.410332433786886774, 35.29983070667008604 ) ) ;
#24780 = CARTESIAN_POINT ( 'NONE',  ( 33.46699938050304013, 27.96183152705961206, 47.04930799450051637 ) ) ;
#24781 = DIRECTION ( 'NONE',  ( -1.101824276508909887E-16, 1.000000000000000000, -0.000000000000000000 ) ) ;
#24782 = CARTESIAN_POINT ( 'NONE',  ( 45.24946171279598417, 29.12124452788248163, 47.99220971130007030 ) ) ;
#24783 = APPLICATION_PROTOCOL_DEFINITION ( 'draft international standard', 'automotive_design', 1998, #93 ) ;
#24784 = EDGE_LOOP ( 'NONE', ( #43, #22319, #21550, #10558 ) ) ;
#24785 = EDGE_LOOP ( 'NONE', ( #11779, #10316, #28378, #22614 ) ) ;
#24786 = DIRECTION ( 'NONE',  ( -1.101824276508909887E-16, 1.000000000000000000, -0.000000000000000000 ) ) ;
#24787 = CARTESIAN_POINT ( 'NONE',  ( -41.24971778908466291, 11.62557032131817358, 57.04930799450051637 ) ) ;
#24788 = DIRECTION ( 'NONE',  ( -1.000000000000000000, 0.000000000000000000, 0.000000000000000000 ) ) ;
#24789 = CIRCLE ( 'NONE', #21640, 0.1250000000000018319 ) ;
#24790 = ORIENTED_EDGE ( 'NONE', *, *, #13208, .F. ) ;
#24791 = CARTESIAN_POINT ( 'NONE',  ( 45.35708200440645044, 29.09118040159425789, 45.92000246470680480 ) ) ;
#24792 = CARTESIAN_POINT ( 'NONE',  ( 21.09785597605719332, 25.56454579224779877, 70.54930799450050927 ) ) ;
#24793 = TOROIDAL_SURFACE ( 'NONE', #29532, 22.69860022854976123, 0.2999999999999999889 ) ;
#24794 = ORIENTED_EDGE ( 'NONE', *, *, #23968, .F. ) ;
#24795 = DIRECTION ( 'NONE',  ( -1.101824276508909887E-16, 1.000000000000000000, -0.000000000000000000 ) ) ;
#24796 = CARTESIAN_POINT ( 'NONE',  ( 44.77625694075214824, 26.01454579807171186, 48.23360063142255427 ) ) ;
#24797 = CARTESIAN_POINT ( 'NONE',  ( -40.59758774925371938, 7.567737757495682338, 35.90717268343339441 ) ) ;
#24798 = EDGE_CURVE ( 'NONE', #32074, #16648, #2132, .T. ) ;
#24799 = EDGE_CURVE ( 'NONE', #10889, #7845, #10037, .T. ) ;
#24800 = EDGE_CURVE ( 'NONE', #229, #25363, #16296, .T. ) ;
#24801 = AXIS2_PLACEMENT_3D ( 'NONE', #9419, #32069, #21545 ) ;
#24802 =( BOUNDED_CURVE ( )  B_SPLINE_CURVE ( 2, ( #10187, #2791, #25281, #22809, #32347, #323, #17560, #9856, #7887 ),
 .UNSPECIFIED., .F., .F. ) 
 B_SPLINE_CURVE_WITH_KNOTS ( ( 3, 2, 2, 2, 3 ),
 ( 0.1071428583041297289, 0.1190476190476190410, 0.1428571428571428492, 0.1666666666666666574, 0.1785714297327012090 ),
 .UNSPECIFIED. ) 
 CURVE ( )  GEOMETRIC_REPRESENTATION_ITEM ( )  RATIONAL_B_SPLINE_CURVE ( ( 0.9330127018922200755, 0.9330127084266225390, 1.000000000000000000, 0.8660254037844388186, 1.000000000000000000, 0.8660254037844388186, 1.000000000000000000, 0.9330126953578159466, 0.9330127018922200755 ) ) 
 REPRESENTATION_ITEM ( '' )  );
#24803 = AXIS2_PLACEMENT_3D ( 'NONE', #21787, #31810, #19491 ) ;
#24804 = ADVANCED_FACE ( 'NONE', ( #14848 ), #11730, .T. ) ;
#24805 = EDGE_CURVE ( 'NONE', #27840, #2021, #24850, .T. ) ;
#24806 = ORIENTED_EDGE ( 'NONE', *, *, #23612, .F. ) ;
#24807 = ORIENTED_EDGE ( 'NONE', *, *, #19552, .F. ) ;
#24808 = CARTESIAN_POINT ( 'NONE',  ( -40.40505316653322865, 8.317079188576503412, 54.54930799450051637 ) ) ;
#24809 = DIRECTION ( 'NONE',  ( 0.000000000000000000, 0.000000000000000000, 1.000000000000000000 ) ) ;
#24810 = CARTESIAN_POINT ( 'NONE',  ( 49.49063479933183629, 27.39951373492759856, 47.17357720316391578 ) ) ;
#24811 = ORIENTED_EDGE ( 'NONE', *, *, #1405, .F. ) ;
#24812 = AXIS2_PLACEMENT_3D ( 'NONE', #22602, #12119, #12281 ) ;
#24813 = LINE ( 'NONE', #29910, #15970 ) ;
#24815 = DIRECTION ( 'NONE',  ( 0.000000000000000000, 0.000000000000000000, -1.000000000000000000 ) ) ;
#24814 = AXIS2_PLACEMENT_3D ( 'NONE', #15372, #15529, #5685 ) ;
#24816 = FACE_OUTER_BOUND ( 'NONE', #27950, .T. ) ;
#24817 = FACE_OUTER_BOUND ( 'NONE', #22087, .T. ) ;
#24818 = CARTESIAN_POINT ( 'NONE',  ( 21.09992658989239089, 30.21664230456641675, 47.04930799450051637 ) ) ;
#24820 = AXIS2_PLACEMENT_3D ( 'NONE', #3019, #30934, #13532 ) ;
#24819 = FACE_OUTER_BOUND ( 'NONE', #22125, .T. ) ;
#24821 = FACE_OUTER_BOUND ( 'NONE', #11750, .T. ) ;
#24822 = CARTESIAN_POINT ( 'NONE',  ( 21.09785597605719332, 11.92558985988973497, 47.04930799450051637 ) ) ;
#24823 = AXIS2_PLACEMENT_3D ( 'NONE', #3966, #11510, #9052 ) ;
#24824 = DIRECTION ( 'NONE',  ( 0.9612616959383194493, 0.2756373558169974980, 8.795445018804946186E-19 ) ) ;
#24825 = LINE ( 'NONE', #22019, #5349 ) ;
#24826 = FILL_AREA_STYLE_COLOUR ( '', #31752 ) ;
#24827 = ORIENTED_EDGE ( 'NONE', *, *, #27347, .F. ) ;
#24828 = VERTEX_POINT ( 'NONE', #4829 ) ;
#24829 = ADVANCED_FACE ( 'NONE', ( #9592 ), #30295, .F. ) ;
#24830 = CARTESIAN_POINT ( 'NONE',  ( 33.46699938050304013, 28.46183152705961206, 47.04930799450051637 ) ) ;
#24831 = EDGE_CURVE ( 'NONE', #3679, #18639, #10327, .T. ) ;
#24832 = CARTESIAN_POINT ( 'NONE',  ( 44.49514591562071075, 25.25621246473836834, 46.91413598593712209 ) ) ;
#24833 = CARTESIAN_POINT ( 'NONE',  ( 21.09785597605719332, 15.43591091851532759, 33.06511779397247608 ) ) ;
#24834 = DIRECTION ( 'NONE',  ( 0.4544104193609900810, 5.611869858668441979E-17, 0.8907924397839090958 ) ) ;
#24835 = EDGE_LOOP ( 'NONE', ( #15750, #21039, #24079, #21402 ) ) ;
#24836 = DIRECTION ( 'NONE',  ( 0.000000000000000000, 0.000000000000000000, -1.000000000000000000 ) ) ;
#24837 = CARTESIAN_POINT ( 'NONE',  ( 21.09785597605719332, 39.33406896771847983, 47.04930799450051637 ) ) ;
#24838 = CARTESIAN_POINT ( 'NONE',  ( 21.09992658989238734, 31.09164230456639544, 47.04930799450051637 ) ) ;
#24839 = ORIENTED_EDGE ( 'NONE', *, *, #13798, .T. ) ;
#24840 = ORIENTED_EDGE ( 'NONE', *, *, #15444, .F. ) ;
#24841 = FACE_OUTER_BOUND ( 'NONE', #22291, .T. ) ;
#24842 = DIRECTION ( 'NONE',  ( -0.000000000000000000, -1.000000000000000000, -0.000000000000000000 ) ) ;
#24843 = CARTESIAN_POINT ( 'NONE',  ( 21.09992658989239089, 28.72145308207318237, 47.04930799450051637 ) ) ;
#24844 = CARTESIAN_POINT ( 'NONE',  ( 21.09785597605720753, 14.86454579224779948, 47.04930799450052348 ) ) ;
#24845 = VECTOR ( 'NONE', #17942, 1000.000000000000000 ) ;
#24846 = CARTESIAN_POINT ( 'NONE',  ( 45.78890401032107604, 29.38203082867340044, 48.92530043617153979 ) ) ;
#24847 = EDGE_LOOP ( 'NONE', ( #7245, #8971, #19340, #27455 ) ) ;
#24848 = ADVANCED_FACE ( 'NONE', ( #14517 ), #10565, .T. ) ;
#24849 = VERTEX_POINT ( 'NONE', #29124 ) ;
#24850 = LINE ( 'NONE', #21560, #21533 ) ;
#24851 = ORIENTED_EDGE ( 'NONE', *, *, #11527, .F. ) ;
#24852 = EDGE_CURVE ( 'NONE', #14823, #29876, #6640, .T. ) ;
#24853 = DIRECTION ( 'NONE',  ( -0.000000000000000000, -1.000000000000000000, -0.000000000000000000 ) ) ;
#24854 = DIRECTION ( 'NONE',  ( -1.000000000000000000, 0.000000000000000000, 0.000000000000000000 ) ) ;
#24855 = EDGE_CURVE ( 'NONE', #29052, #24243, #70, .T. ) ;
#24856 = ORIENTED_EDGE ( 'NONE', *, *, #12546, .F. ) ;
#24857 = CARTESIAN_POINT ( 'NONE',  ( 34.09963999142011204, 17.16467605102632632, 47.04930799450052348 ) ) ;
#24858 = ORIENTED_EDGE ( 'NONE', *, *, #9950, .F. ) ;
#24859 = CARTESIAN_POINT ( 'NONE',  ( 21.09992658989239089, 29.59164230456639899, 47.04930799450051637 ) ) ;
#24860 = AXIS2_PLACEMENT_3D ( 'NONE', #25501, #25973, #20728 ) ;
#24861 = FACE_OUTER_BOUND ( 'NONE', #19659, .T. ) ;
#24862 = AXIS2_PLACEMENT_3D ( 'NONE', #24483, #23556, #28495 ) ;
#24863 = CARTESIAN_POINT ( 'NONE',  ( 71.55936645880184699, 9.702389020015065313, 73.75010705023584023 ) ) ;
#24864 = ORIENTED_EDGE ( 'NONE', *, *, #11243, .T. ) ;
#24865 = EDGE_CURVE ( 'NONE', #21395, #21286, #16800, .T. ) ;
#24866 = CARTESIAN_POINT ( 'NONE',  ( 72.25012468985910630, 5.370505999354230120, 77.42531960576580730 ) ) ;
#24867 = DIRECTION ( 'NONE',  ( -1.101824276508909887E-16, 1.000000000000000000, -0.000000000000000000 ) ) ;
#24868 = CARTESIAN_POINT ( 'NONE',  ( 33.72499318558949710, 25.59184655352419213, 47.04930799450051637 ) ) ;
#24869 = VECTOR ( 'NONE', #11368, 1000.000000000000000 ) ;
#24870 = ADVANCED_FACE ( 'NONE', ( #12053 ), #22610, .T. ) ;
#24871 = FACE_OUTER_BOUND ( 'NONE', #8693, .T. ) ;
#24872 = DIRECTION ( 'NONE',  ( -0.000000000000000000, -1.000000000000000000, 0.000000000000000000 ) ) ;
#24873 = CONICAL_SURFACE ( 'NONE', #19624, 13.20000000000000995, 0.7853981633974612686 ) ;
#24874 = DIRECTION ( 'NONE',  ( 0.000000000000000000, 0.000000000000000000, -1.000000000000000000 ) ) ;
#24875 = ORIENTED_EDGE ( 'NONE', *, *, #26937, .F. ) ;
#24876 = DIRECTION ( 'NONE',  ( -1.000000000000000000, 0.000000000000000000, 0.000000000000000000 ) ) ;
#24877 = CARTESIAN_POINT ( 'NONE',  ( 21.09992658989239089, 26.34164230456639899, 47.04930799450051637 ) ) ;
#24878 = ORIENTED_EDGE ( 'NONE', *, *, #10696, .T. ) ;
#24879 = CYLINDRICAL_SURFACE ( 'NONE', #28751, 12.36707279061065101 ) ;
#24880 = B_SPLINE_CURVE_WITH_KNOTS ( 'NONE', 3,
 ( #827, #23634, #3766, #3115, #10851, #26258 ),
 .UNSPECIFIED., .F., .F.,
 ( 4, 2, 4 ),
 ( 0.000000000000000000, 0.5000000000000000000, 1.000000000000000000 ),
 .UNSPECIFIED. ) ;
#24881 = DIRECTION ( 'NONE',  ( 1.000000000000000000, 0.000000000000000000, 0.000000000000000000 ) ) ;
#24882 = ORIENTED_EDGE ( 'NONE', *, *, #30062, .T. ) ;
#24883 = VERTEX_POINT ( 'NONE', #14360 ) ;
#24884 = ADVANCED_FACE ( 'NONE', ( #4167 ), #18910, .T. ) ;
#24885 = ORIENTED_EDGE ( 'NONE', *, *, #3394, .T. ) ;
#24886 = CIRCLE ( 'NONE', #8654, 12.36707279061065101 ) ;
#24887 = TOROIDAL_SURFACE ( 'NONE', #31190, 12.61792373059860495, 0.1250000000000008604 ) ;
#24888 = AXIS2_PLACEMENT_3D ( 'NONE', #19306, #7339, #31798 ) ;
#24889 = CIRCLE ( 'NONE', #24359, 12.68414152717711119 ) ;
#24890 = TOROIDAL_SURFACE ( 'NONE', #6548, 12.40141737965282509, 0.1249999999999980849 ) ;
#24891 = ADVANCED_FACE ( 'NONE', ( #31911 ), #24190, .F. ) ;
#24892 = DIRECTION ( 'NONE',  ( 0.000000000000000000, 0.000000000000000000, 1.000000000000000000 ) ) ;
#24893 = EDGE_CURVE ( 'NONE', #14245, #27708, #9755, .T. ) ;
#24894 = ORIENTED_EDGE ( 'NONE', *, *, #387, .T. ) ;
#24895 = ORIENTED_EDGE ( 'NONE', *, *, #7815, .T. ) ;
#24896 = LINE ( 'NONE', #19628, #24204 ) ;
#24897 = CARTESIAN_POINT ( 'NONE',  ( -44.25434836777630210, -5.709091131881068648, 53.11493085759866517 ) ) ;
#24898 = LINE ( 'NONE', #24561, #3956 ) ;
#24899 = DIRECTION ( 'NONE',  ( -0.000000000000000000, -1.000000000000000000, 0.000000000000000000 ) ) ;
#24900 = CARTESIAN_POINT ( 'NONE',  ( 8.698509210239585343, 32.09164230456639899, 47.04930799450051637 ) ) ;
#24901 = ORIENTED_EDGE ( 'NONE', *, *, #27161, .T. ) ;
#24902 = DIRECTION ( 'NONE',  ( -1.101824276508909887E-16, 1.000000000000000000, -0.000000000000000000 ) ) ;
#24903 = ORIENTED_EDGE ( 'NONE', *, *, #4341, .F. ) ;
#24904 = CARTESIAN_POINT ( 'NONE',  ( -33.35089495028901041, -1.269481974065232555, 13.46653852984619348 ) ) ;
#24905 = CARTESIAN_POINT ( 'NONE',  ( -5.948280841129993668, 9.423225080673429233, -3.404543741840068805 ) ) ;
#24906 = ADVANCED_FACE ( 'NONE', ( #7291 ), #11863, .T. ) ;
#24907 = ORIENTED_EDGE ( 'NONE', *, *, #8459, .F. ) ;
#24908 = DIRECTION ( 'NONE',  ( -1.101824276508909887E-16, 1.000000000000000000, -0.000000000000000000 ) ) ;
#24909 = CYLINDRICAL_SURFACE ( 'NONE', #1099, 55.00000000000000000 ) ;
#24910 = DIRECTION ( 'NONE',  ( -0.4848096202463427762, -0.8746197071393926326, 0.000000000000000000 ) ) ;
#24911 = DIRECTION ( 'NONE',  ( 0.9612616959383213366, 0.2756373558169906701, -3.016780184296941179E-15 ) ) ;
#24912 = DIRECTION ( 'NONE',  ( -1.000000000000000000, 0.000000000000000000, 0.000000000000000000 ) ) ;
#24913 = EDGE_CURVE ( 'NONE', #12822, #23541, #17095, .T. ) ;
#24914 = CARTESIAN_POINT ( 'NONE',  ( 46.00908685603034343, 28.94624452788248092, 44.91496614357595263 ) ) ;
#24915 = CIRCLE ( 'NONE', #15485, 0.1250000000000001110 ) ;
#24916 = CARTESIAN_POINT ( 'NONE',  ( -40.46271621608484281, 3.081581074246047880, 37.04930799450052348 ) ) ;
#24917 = DIRECTION ( 'NONE',  ( -0.4848096202463673121, -0.8746197071393789768, 0.000000000000000000 ) ) ;
#24918 = CONICAL_SURFACE ( 'NONE', #1845, 13.81487396812510937, 1.187672012580059944 ) ;
#24919 = ORIENTED_EDGE ( 'NONE', *, *, #17853, .F. ) ;
#24920 = CYLINDRICAL_SURFACE ( 'NONE', #6653, 2.500000000000002220 ) ;
#24921 = CARTESIAN_POINT ( 'NONE',  ( -39.02270572350619915, 5.305725667695960546, 52.04930799450051637 ) ) ;
#24922 = AXIS2_PLACEMENT_3D ( 'NONE', #30448, #2859, #17795 ) ;
#24923 = VERTEX_POINT ( 'NONE', #22183 ) ;
#24924 = CIRCLE ( 'NONE', #19654, 0.1000000000000006301 ) ;
#24925 = CIRCLE ( 'NONE', #21760, 1.300000000000002487 ) ;
#24926 = FACE_BOUND ( 'NONE', #31865, .T. ) ;
#24927 = VERTEX_POINT ( 'NONE', #9069 ) ;
#24928 = ORIENTED_EDGE ( 'NONE', *, *, #31145, .F. ) ;
#24929 = ORIENTED_EDGE ( 'NONE', *, *, #6264, .F. ) ;
#24930 = TOROIDAL_SURFACE ( 'NONE', #20727, 12.68414152717710763, 0.1999999999999992339 ) ;
#24931 = EDGE_LOOP ( 'NONE', ( #25688, #1866, #10761, #9208, #18083 ) ) ;
#24932 = ADVANCED_FACE ( 'NONE', ( #1678, #24655 ), #17259, .T. ) ;
#24933 = DIRECTION ( 'NONE',  ( -1.101824276508909887E-16, 1.000000000000000000, -0.000000000000000000 ) ) ;
#24934 = CARTESIAN_POINT ( 'NONE',  ( 51.92400919103563695, -5.935454207752202116, -3.337848843846767721 ) ) ;
#24935 = CIRCLE ( 'NONE', #10804, 1.524998423334080533 ) ;
#24936 = CIRCLE ( 'NONE', #3886, 2.500000000000002220 ) ;
#24937 = ORIENTED_EDGE ( 'NONE', *, *, #23825, .T. ) ;
#24938 = DIRECTION ( 'NONE',  ( -0.000000000000000000, -1.000000000000000000, 0.000000000000000000 ) ) ;
#24939 = DIRECTION ( 'NONE',  ( -1.000000000000000000, 0.000000000000000000, 0.000000000000000000 ) ) ;
#24940 = DIRECTION ( 'NONE',  ( 0.000000000000000000, 1.000000000000000000, -0.000000000000000000 ) ) ;
#24941 = CARTESIAN_POINT ( 'NONE',  ( 44.70507715278255745, 26.26291119454915801, 46.92503878583765697 ) ) ;
#24942 = ORIENTED_EDGE ( 'NONE', *, *, #1951, .F. ) ;
#24943 = ORIENTED_EDGE ( 'NONE', *, *, #28574, .T. ) ;
#24944 = DIRECTION ( 'NONE',  ( -0.000000000000000000, -1.000000000000000000, 0.000000000000000000 ) ) ;
#24945 = ADVANCED_FACE ( 'NONE', ( #32212 ), #29952, .T. ) ;
#24946 = ORIENTED_EDGE ( 'NONE', *, *, #4117, .F. ) ;
#24947 = CIRCLE ( 'NONE', #1877, 13.00000000000000533 ) ;
#24948 = DIRECTION ( 'NONE',  ( 0.000000000000000000, -1.000000000000000000, 0.000000000000000000 ) ) ;
#24949 = DIRECTION ( 'NONE',  ( -1.101824276508909887E-16, 1.000000000000000000, -0.000000000000000000 ) ) ;
#24950 = CARTESIAN_POINT ( 'NONE',  ( -40.68984688381691228, 6.797157182225290306, 34.72546689663558084 ) ) ;
#24951 = CARTESIAN_POINT ( 'NONE',  ( 21.09785597605720042, -14.03534765547855656, -12.76032168114853782 ) ) ;
#24952 = CARTESIAN_POINT ( 'NONE',  ( -41.74033427429298371, 15.41509661078533355, 38.44930799450052206 ) ) ;
#24953 =( NAMED_UNIT ( * ) SI_UNIT ( $, .STERADIAN. ) SOLID_ANGLE_UNIT ( ) );
#24954 = ORIENTED_EDGE ( 'NONE', *, *, #23572, .F. ) ;
#24955 = EDGE_LOOP ( 'NONE', ( #44, #21530, #15883, #3669 ) ) ;
#24956 = FACE_OUTER_BOUND ( 'NONE', #27483, .T. ) ;
#24957 = DIRECTION ( 'NONE',  ( 0.9612616959383128989, 0.2756373558170196469, 0.000000000000000000 ) ) ;
#24958 = VERTEX_POINT ( 'NONE', #12022 ) ;
#24959 = CARTESIAN_POINT ( 'NONE',  ( 46.99023568444673771, 27.22451373492759785, 49.12151524109405898 ) ) ;
#24960 = ORIENTED_EDGE ( 'NONE', *, *, #12778, .F. ) ;
#24961 = CARTESIAN_POINT ( 'NONE',  ( 21.09785597605719332, 12.78350261226561280, -8.675054649682497399 ) ) ;
#24962 = COLOUR_RGB ( '',0.7921568627450980005, 0.8196078431372548767, 0.9333333333333333481 ) ;
#24963 = DIRECTION ( 'NONE',  ( -0.000000000000000000, -1.000000000000000000, 0.000000000000000000 ) ) ;
#24964 = AXIS2_PLACEMENT_3D ( 'NONE', #4833, #9919, #29779 ) ;
#24965 = ORIENTED_EDGE ( 'NONE', *, *, #14388, .T. ) ;
#24966 = EDGE_LOOP ( 'NONE', ( #27852, #21825, #8924, #26535 ) ) ;
#24967 = DIRECTION ( 'NONE',  ( 0.000000000000000000, 0.000000000000000000, 1.000000000000000000 ) ) ;
#24968 = CARTESIAN_POINT ( 'NONE',  ( 21.09785597605719332, -15.93545420775219945, 47.04930799450051637 ) ) ;
#24969 = CARTESIAN_POINT ( 'NONE',  ( 48.40186567930498285, 27.51618040159426570, 45.03923535223908203 ) ) ;
#24970 = ORIENTED_EDGE ( 'NONE', *, *, #28673, .T. ) ;
#24971 = DIRECTION ( 'NONE',  ( -1.000000000000000000, 0.000000000000000000, 0.000000000000000000 ) ) ;
#24972 = DIRECTION ( 'NONE',  ( 0.000000000000000000, 0.000000000000000000, -1.000000000000000000 ) ) ;
#24973 = CIRCLE ( 'NONE', #17644, 0.4999999999999988343 ) ;
#24974 = CARTESIAN_POINT ( 'NONE',  ( -40.50048552624281939, 7.561504794674588581, 53.84930799450049932 ) ) ;
#24975 = EDGE_CURVE ( 'NONE', #16293, #25493, #13192, .T. ) ;
#24976 = DIRECTION ( 'NONE',  ( 0.000000000000000000, -0.000000000000000000, -1.000000000000000000 ) ) ;
#24977 = CARTESIAN_POINT ( 'NONE',  ( 21.09785597605719687, 30.56454579224779522, 78.54930799450052348 ) ) ;
#24978 = DIRECTION ( 'NONE',  ( -1.000000000000000000, 0.000000000000000000, 0.000000000000000000 ) ) ;
#24979 = EDGE_CURVE ( 'NONE', #23177, #18054, #15330, .T. ) ;
#24980 = CARTESIAN_POINT ( 'NONE',  ( 21.09785597605720753, 14.98269195386757602, 47.04930799450052348 ) ) ;
#24982 = ADVANCED_FACE ( 'NONE', ( #24485 ), #26791, .T. ) ;
#24981 = CARTESIAN_POINT ( 'NONE',  ( 21.09992658989238734, 38.56284415653841791, 47.04930799450051637 ) ) ;
#24983 = EDGE_CURVE ( 'NONE', #13414, #18622, #4139, .T. ) ;
#24984 = EDGE_CURVE ( 'NONE', #12804, #10005, #1120, .T. ) ;
#24985 = DIRECTION ( 'NONE',  ( -1.000000000000000000, 0.000000000000000000, 0.000000000000000000 ) ) ;
#24986 = SURFACE_STYLE_USAGE ( .BOTH. , #2005 ) ;
#24987 = ADVANCED_FACE ( 'NONE', ( #9883 ), #20365, .F. ) ;
#24988 = ORIENTED_EDGE ( 'NONE', *, *, #11198, .F. ) ;
#24989 = ORIENTED_EDGE ( 'NONE', *, *, #9337, .F. ) ;
#24990 = CARTESIAN_POINT ( 'NONE',  ( 33.37634396954526750, 24.84164230456639544, 47.04930799450051637 ) ) ;
#24991 = ADVANCED_FACE ( 'NONE', ( #8080 ), #28101, .T. ) ;
#24992 = CARTESIAN_POINT ( 'NONE',  ( 47.03171727263369206, 25.15018075992191982, 44.52927784484388241 ) ) ;
#24993 = CARTESIAN_POINT ( 'NONE',  ( -35.11018699695847545, -4.854904164370157815, 14.08771498410514234 ) ) ;
#24994 = TOROIDAL_SURFACE ( 'NONE', #22902, 12.40141737965288193, 0.1250000000000005829 ) ;
#24995 = FACE_OUTER_BOUND ( 'NONE', #28730, .T. ) ;
#24996 = VERTEX_POINT ( 'NONE', #18071 ) ;
#24997 = DIRECTION ( 'NONE',  ( 0.000000000000000000, -0.000000000000000000, -1.000000000000000000 ) ) ;
#24998 = CARTESIAN_POINT ( 'NONE',  ( 33.72499318558949710, 31.84143805560860940, 47.04930799450051637 ) ) ;
#24999 = DIRECTION ( 'NONE',  ( 0.8746197071393927436, -0.4848096202463423876, -1.277302113040827440E-17 ) ) ;
#25000 = ORIENTED_EDGE ( 'NONE', *, *, #15281, .T. ) ;
#25001 = ORIENTED_EDGE ( 'NONE', *, *, #782, .F. ) ;
#25002 = CARTESIAN_POINT ( 'NONE',  ( -40.11264481937004689, 6.813248423021984301, 39.46181098083825844 ) ) ;
#25003 = DIRECTION ( 'NONE',  ( 0.000000000000000000, 0.000000000000000000, 1.000000000000000000 ) ) ;
#25004 = CARTESIAN_POINT ( 'NONE',  ( -58.11219453028166981, 25.56454579224780232, 49.54930799450023926 ) ) ;
#25005 = DIRECTION ( 'NONE',  ( -0.6797146636928631525, -0.1949050434465325332, -0.7071067811865497932 ) ) ;
#25006 = CARTESIAN_POINT ( 'NONE',  ( 44.90600895698101169, 29.28496411753620876, 46.11062626847921564 ) ) ;
#25007 = EDGE_LOOP ( 'NONE', ( #22570, #16941, #11340, #19351 ) ) ;
#25008 = EDGE_CURVE ( 'NONE', #21286, #29013, #21028, .T. ) ;
#25009 = ORIENTED_EDGE ( 'NONE', *, *, #3799, .T. ) ;
#25010 = DIRECTION ( 'NONE',  ( 1.000000000000000000, 0.000000000000000000, 0.000000000000000000 ) ) ;
#25011 = EDGE_CURVE ( 'NONE', #30056, #2086, #14230, .T. ) ;
#25012 = TOROIDAL_SURFACE ( 'NONE', #10873, 12.61792373059899219, 0.1249999999999961003 ) ;
#25013 = ORIENTED_EDGE ( 'NONE', *, *, #32119, .T. ) ;
#25014 = DIRECTION ( 'NONE',  ( 5.937205496305277864E-17, -0.8746197071393925215, 0.4848096202463429982 ) ) ;
#25015 = EDGE_LOOP ( 'NONE', ( #6529, #3633, #15672, #14880 ) ) ;
#25016 = LINE ( 'NONE', #7787, #14962 ) ;
#25017 = ORIENTED_EDGE ( 'NONE', *, *, #29126, .F. ) ;
#25018 = CYLINDRICAL_SURFACE ( 'NONE', #19377, 12.62506659569710443 ) ;
#25019 = DIRECTION ( 'NONE',  ( -1.101824276508909887E-16, 1.000000000000000000, -0.000000000000000000 ) ) ;
#25020 = EDGE_CURVE ( 'NONE', #4178, #32468, #11191, .T. ) ;
#25021 = DIRECTION ( 'NONE',  ( -1.000000000000000000, 0.000000000000000000, 0.000000000000000000 ) ) ;
#25022 = ADVANCED_FACE ( 'NONE', ( #13004 ), #30237, .F. ) ;
#25023 = DIRECTION ( 'NONE',  ( -1.101824276508909887E-16, 1.000000000000000000, -0.000000000000000000 ) ) ;
#25024 = ORIENTED_EDGE ( 'NONE', *, *, #1393, .F. ) ;
#25025 = DIRECTION ( 'NONE',  ( -1.000000000000000000, 0.000000000000000000, 0.000000000000000000 ) ) ;
#25027 = LINE ( 'NONE', #14862, #3755 ) ;
#25026 = VECTOR ( 'NONE', #28114, 1000.000000000000000 ) ;
#25028 = CARTESIAN_POINT ( 'NONE',  ( 49.00637973737335074, 15.77906836436399374, 50.79063624159320511 ) ) ;
#25029 = LINE ( 'NONE', #28303, #24508 ) ;
#25030 = CARTESIAN_POINT ( 'NONE',  ( -38.36853489569023168, 7.065850718397949315, 32.04930799450052348 ) ) ;
#25031 = VERTEX_POINT ( 'NONE', #5607 ) ;
#25032 = DIRECTION ( 'NONE',  ( 0.000000000000000000, 0.000000000000000000, 1.000000000000000000 ) ) ;
#25033 = DIRECTION ( 'NONE',  ( 0.000000000000000000, -0.8746197071393925215, -0.4848096202463429982 ) ) ;
#25034 = AXIS2_PLACEMENT_3D ( 'NONE', #19071, #13376, #1361 ) ;
#25035 = ORIENTED_EDGE ( 'NONE', *, *, #4334, .F. ) ;
#25036 = B_SPLINE_CURVE_WITH_KNOTS ( 'NONE', 3,
 ( #8445, #25676, #28624, #5827, #566, #5655, #3018, #3181, #30771, #18124, #21061, #3671, #18595, #26154, #30933, #15661 ),
 .UNSPECIFIED., .F., .F.,
 ( 4, 2, 2, 2, 2, 2, 2, 4 ),
 ( 0.000000000000000000, 0.0003391165876995429857, 0.0004238957346244386255, 0.0005086748815493342653, 0.0005298696682805630271, 0.0005510644550117917888, 0.0005934540284742352177, 0.0006782331753991313996 ),
 .UNSPECIFIED. ) ;
#25037 = CYLINDRICAL_SURFACE ( 'NONE', #14069, 12.62506659569710266 ) ;
#25038 = DIRECTION ( 'NONE',  ( -1.101824276508909887E-16, 1.000000000000000000, -0.000000000000000000 ) ) ;
#25039 = EDGE_LOOP ( 'NONE', ( #27097, #8241, #7962, #18532 ) ) ;
#25040 = PRODUCT_DEFINITION_SHAPE ( 'NONE', 'NONE',  #8905 ) ;
#25041 = LINE ( 'NONE', #2722, #1008 ) ;
#25042 = ORIENTED_EDGE ( 'NONE', *, *, #15716, .F. ) ;
#25043 = ADVANCED_FACE ( 'NONE', ( #24821 ), #30081, .T. ) ;
#25044 = ORIENTED_EDGE ( 'NONE', *, *, #27158, .T. ) ;
#25045 = EDGE_CURVE ( 'NONE', #29763, #8194, #32055, .T. ) ;
#25046 = VECTOR ( 'NONE', #10780, 1000.000000000000000 ) ;
#25047 = EDGE_CURVE ( 'NONE', #23695, #1790, #23123, .T. ) ;
#25048 = AXIS2_PLACEMENT_3D ( 'NONE', #21923, #16518, #24232 ) ;
#25049 = AXIS2_PLACEMENT_3D ( 'NONE', #10224, #20223, #30247 ) ;
#25050 = DIRECTION ( 'NONE',  ( -1.000000000000000000, -1.101824276508909887E-16, 0.000000000000000000 ) ) ;
#25051 = EDGE_LOOP ( 'NONE', ( #22302, #16832, #4531, #22697 ) ) ;
#25052 = AXIS2_PLACEMENT_3D ( 'NONE', #10777, #8620, #28329 ) ;
#25053 = EDGE_LOOP ( 'NONE', ( #4089, #16310, #12163, #30873 ) ) ;
#25054 = CARTESIAN_POINT ( 'NONE',  ( 73.76522107166850617, 0.6013300790671820550, 14.08091825663031926 ) ) ;
#25055 = CARTESIAN_POINT ( 'NONE',  ( -40.60722745863126448, 9.415333058485023443, 34.69072935073783270 ) ) ;
#25056 = DIRECTION ( 'NONE',  ( 0.000000000000000000, 0.000000000000000000, 1.000000000000000000 ) ) ;
#25057 = CARTESIAN_POINT ( 'NONE',  ( -2.402144023942794249, 14.86454579224779948, 47.04930799450052348 ) ) ;
#25058 = DIRECTION ( 'NONE',  ( -1.000000000000000000, 0.000000000000000000, 0.000000000000000000 ) ) ;
#25059 = EDGE_CURVE ( 'NONE', #30824, #21924, #3725, .T. ) ;
#25060 = ORIENTED_EDGE ( 'NONE', *, *, #24033, .F. ) ;
#25061 = DIRECTION ( 'NONE',  ( -1.101824276508909887E-16, 1.000000000000000000, -0.000000000000000000 ) ) ;
#25062 = ORIENTED_EDGE ( 'NONE', *, *, #6028, .F. ) ;
#25063 = CARTESIAN_POINT ( 'NONE',  ( -37.03867781279360827, -5.627071229729164514, 14.99370382524486089 ) ) ;
#25064 = CARTESIAN_POINT ( 'NONE',  ( 21.09992658989238734, 30.84164230456639544, 47.04930799450051637 ) ) ;
#25065 = EDGE_LOOP ( 'NONE', ( #14911, #23705, #29866, #14137 ) ) ;
#25066 = CYLINDRICAL_SURFACE ( 'NONE', #22623, 12.36707279061065101 ) ;
#25067 = DIRECTION ( 'NONE',  ( -0.000000000000000000, 1.000000000000000000, -0.000000000000000000 ) ) ;
#25068 = CARTESIAN_POINT ( 'NONE',  ( -42.26253548098706858, 13.64258395852576911, 54.54930799450051637 ) ) ;
#25069 = CARTESIAN_POINT ( 'NONE',  ( -40.02540636251514172, 2.839176264122877047, 59.04930799450051637 ) ) ;
#25070 = CARTESIAN_POINT ( 'NONE',  ( 21.09785597605720753, 13.86454579224779948, 47.04930799450052348 ) ) ;
#25071 = CARTESIAN_POINT ( 'NONE',  ( 48.18662509608405031, 28.59624452788247950, 49.18364984542562013 ) ) ;
#25072 = FACE_BOUND ( 'NONE', #743, .T. ) ;
#25073 = DIRECTION ( 'NONE',  ( -1.000000000000000000, 0.000000000000000000, 0.000000000000000000 ) ) ;
#25074 = ORIENTED_EDGE ( 'NONE', *, *, #20161, .F. ) ;
#25075 = DIRECTION ( 'NONE',  ( 0.000000000000000000, 1.000000000000000000, -0.000000000000000000 ) ) ;
#25076 = LINE ( 'NONE', #29847, #21894 ) ;
#25077 = AXIS2_PLACEMENT_3D ( 'NONE', #21191, #23353, #16114 ) ;
#25078 = ORIENTED_EDGE ( 'NONE', *, *, #17154, .T. ) ;
#25079 = CIRCLE ( 'NONE', #6702, 55.62842601856165459 ) ;
#25080 = DIRECTION ( 'NONE',  ( -0.9612616959383200044, -0.2756373558169954996, 1.660411357259285896E-16 ) ) ;
#25081 = CIRCLE ( 'NONE', #11957, 55.00000000000000000 ) ;
#25082 = VERTEX_POINT ( 'NONE', #14976 ) ;
#25083 = AXIS2_PLACEMENT_3D ( 'NONE', #9783, #17486, #19774 ) ;
#25084 = ADVANCED_FACE ( 'NONE', ( #20050 ), #27604, .F. ) ;
#25085 = EDGE_LOOP ( 'NONE', ( #29709, #26262 ) ) ;
#25086 = DIRECTION ( 'NONE',  ( -1.101824276508909887E-16, 1.000000000000000000, -0.000000000000000000 ) ) ;
#25087 = ADVANCED_FACE ( 'NONE', ( #25144 ), #2659, .T. ) ;
#25088 = CIRCLE ( 'NONE', #970, 4.200000000000000178 ) ;
#25089 = ORIENTED_EDGE ( 'NONE', *, *, #23207, .F. ) ;
#25090 = EDGE_CURVE ( 'NONE', #456, #5630, #9390, .T. ) ;
#25091 = EDGE_CURVE ( 'NONE', #3409, #2830, #3927, .T. ) ;
#25092 = EDGE_CURVE ( 'NONE', #23906, #1567, #12671, .T. ) ;
#25093 = ORIENTED_EDGE ( 'NONE', *, *, #15358, .T. ) ;
#25094 = DIRECTION ( 'NONE',  ( -1.000000000000000000, -1.101824276508910010E-16, 0.000000000000000000 ) ) ;
#25095 = TOROIDAL_SURFACE ( 'NONE', #5157, 12.40141737965279667, 0.1249999999999991951 ) ;
#25096 = ORIENTED_EDGE ( 'NONE', *, *, #19523, .T. ) ;
#25097 = AXIS2_PLACEMENT_3D ( 'NONE', #25634, #13178, #10716 ) ;
#25098 = CYLINDRICAL_SURFACE ( 'NONE', #6763, 2.000000000000001776 ) ;
#25099 = DIRECTION ( 'NONE',  ( 0.000000000000000000, -1.000000000000000000, 0.000000000000000000 ) ) ;
#25100 = CARTESIAN_POINT ( 'NONE',  ( 45.96182992765471909, 26.60087065737812040, 44.82232689504102296 ) ) ;
#25101 = CARTESIAN_POINT ( 'NONE',  ( 45.79384627280941089, 26.37957786121582160, 49.05938063676249072 ) ) ;
#25102 = VERTEX_POINT ( 'NONE', #8678 ) ;
#25103 = ORIENTED_EDGE ( 'NONE', *, *, #29521, .F. ) ;
#25104 = DIRECTION ( 'NONE',  ( -1.101824276508909887E-16, 1.000000000000000000, -0.000000000000000000 ) ) ;
#25105 = EDGE_LOOP ( 'NONE', ( #30223, #4201, #9549, #26459 ) ) ;
#25106 = AXIS2_PLACEMENT_3D ( 'NONE', #24459, #21829, #1817 ) ;
#25107 = DIRECTION ( 'NONE',  ( -1.000000000000000000, 0.000000000000000000, 0.000000000000000000 ) ) ;
#25108 = DIRECTION ( 'NONE',  ( 0.000000000000000000, 0.000000000000000000, -1.000000000000000000 ) ) ;
#25109 = DIRECTION ( 'NONE',  ( -0.09590798424311161585, 0.9774730502038649904, -0.1880108898004995421 ) ) ;
#25110 = CARTESIAN_POINT ( 'NONE',  ( 52.83083363940430388, -5.773219817368569373, -11.52912231966167056 ) ) ;
#25111 = CARTESIAN_POINT ( 'NONE',  ( -42.38687957179149635, 4.148162238787999279, 37.04930799450052348 ) ) ;
#25112 = SHAPE_DEFINITION_REPRESENTATION ( #29486, #20382 ) ;
#25113 = EDGE_LOOP ( 'NONE', ( #8545, #1458, #25690 ) ) ;
#25114 = ORIENTED_EDGE ( 'NONE', *, *, #11352, .F. ) ;
#25115 = CARTESIAN_POINT ( 'NONE',  ( -42.26497471389478733, 14.66834543456875117, 59.01654570186344984 ) ) ;
#25116 = DIRECTION ( 'NONE',  ( -1.000000000000000000, -1.101824276508909764E-16, 0.000000000000000000 ) ) ;
#25117 = DIRECTION ( 'NONE',  ( -1.101824276508909887E-16, 1.000000000000000000, -0.000000000000000000 ) ) ;
#25118 = VERTEX_POINT ( 'NONE', #29016 ) ;
#25119 = CARTESIAN_POINT ( 'NONE',  ( 44.70507715278255034, 28.44951373492759217, 46.92503878583765697 ) ) ;
#25120 = ADVANCED_FACE ( 'NONE', ( #9151 ), #24695, .T. ) ;
#25121 = ORIENTED_EDGE ( 'NONE', *, *, #31216, .T. ) ;
#25122 = FACE_OUTER_BOUND ( 'NONE', #7906, .T. ) ;
#25123 = DIRECTION ( 'NONE',  ( -1.101824276508909887E-16, 1.000000000000000000, -0.000000000000000000 ) ) ;
#25124 = AXIS2_PLACEMENT_3D ( 'NONE', #27560, #2608, #148 ) ;
#25125 = AXIS2_PLACEMENT_3D ( 'NONE', #23385, #30943, #10437 ) ;
#25126 = ADVANCED_FACE ( 'NONE', ( #29176 ), #23666, .T. ) ;
#25127 = CARTESIAN_POINT ( 'NONE',  ( 21.09992658989238734, 32.59164230456639899, 47.04930799450051637 ) ) ;
#25128 = EDGE_CURVE ( 'NONE', #10313, #23399, #31802, .T. ) ;
#25129 = AXIS2_PLACEMENT_3D ( 'NONE', #20989, #31017, #24096 ) ;
#25130 = EDGE_LOOP ( 'NONE', ( #25667, #3402, #20070, #29626, #12095, #12839, #6287, #9869, #24166, #17468, #10854, #29135, #1246, #11603 ) ) ;
#25131 = AXIS2_PLACEMENT_3D ( 'NONE', #22327, #22165, #6911 ) ;
#25132 = ORIENTED_EDGE ( 'NONE', *, *, #9448, .F. ) ;
#25133 = DIRECTION ( 'NONE',  ( -1.000000000000000000, 0.000000000000000000, 0.000000000000000000 ) ) ;
#25134 = CARTESIAN_POINT ( 'NONE',  ( 33.71785032049137953, 24.71664230456639899, 47.04930799450051637 ) ) ;
#25135 = CARTESIAN_POINT ( 'NONE',  ( 48.83862994770794330, 25.94118040159426641, 48.17861352429476796 ) ) ;
#25136 = VERTEX_POINT ( 'NONE', #14085 ) ;
#25137 = DIRECTION ( 'NONE',  ( -1.000000000000000000, 0.000000000000000000, 0.000000000000000000 ) ) ;
#25138 = FACE_OUTER_BOUND ( 'NONE', #9485, .T. ) ;
#25139 = DIRECTION ( 'NONE',  ( 0.9612616959383128989, 0.2756373558170196469, 0.000000000000000000 ) ) ;
#25140 = AXIS2_PLACEMENT_3D ( 'NONE', #27829, #3024, #10604 ) ;
#25141 = FACE_OUTER_BOUND ( 'NONE', #8487, .T. ) ;
#25142 = DIRECTION ( 'NONE',  ( -1.000000000000000000, 0.000000000000000000, 0.000000000000000000 ) ) ;
#25143 = CARTESIAN_POINT ( 'NONE',  ( -40.50726673551752555, 7.559560314205212350, 60.26436683999078525 ) ) ;
#25144 = FACE_OUTER_BOUND ( 'NONE', #15692, .T. ) ;
#25145 = LINE ( 'NONE', #29748, #10512 ) ;
#25146 = LINE ( 'NONE', #25628, #24635 ) ;
#25147 = LINE ( 'NONE', #10867, #4748 ) ;
#25148 = EDGE_LOOP ( 'NONE', ( #18573, #3061, #26056, #29332 ) ) ;
#25149 = ORIENTED_EDGE ( 'NONE', *, *, #9258, .T. ) ;
#25150 = DIRECTION ( 'NONE',  ( 0.8746197071393926326, -0.4848096202463430537, -8.676864087101709653E-18 ) ) ;
#25151 = DIRECTION ( 'NONE',  ( -1.000000000000000000, 0.000000000000000000, 0.000000000000000000 ) ) ;
#25152 = DIRECTION ( 'NONE',  ( -1.101824276508909887E-16, 1.000000000000000000, -0.000000000000000000 ) ) ;
#25153 = AXIS2_PLACEMENT_3D ( 'NONE', #20228, #7605, #4646 ) ;
#25154 = VECTOR ( 'NONE', #19415, 1000.000000000000000 ) ;
#25155 = CARTESIAN_POINT ( 'NONE',  ( 53.69468933856271775, -5.264348929021193335, 103.7321922401826981 ) ) ;
#25156 = VERTEX_POINT ( 'NONE', #8991 ) ;
#25157 = CARTESIAN_POINT ( 'NONE',  ( 21.09785597605719332, 14.86454579224779948, 47.04930799450051637 ) ) ;
#25158 = AXIS2_PLACEMENT_3D ( 'NONE', #30506, #18015, #5555 ) ;
#25159 = FACE_OUTER_BOUND ( 'NONE', #5401, .T. ) ;
#25160 = CARTESIAN_POINT ( 'NONE',  ( 47.79865503179234310, 9.702389020015065313, -3.412202488244239884 ) ) ;
#25161 = EDGE_LOOP ( 'NONE', ( #22950, #14562, #20552, #25584 ) ) ;
#25162 = EDGE_LOOP ( 'NONE', ( #15840, #16889, #23865, #26641 ) ) ;
#25163 = CARTESIAN_POINT ( 'NONE',  ( 21.09785597605719332, -6.704410789454799513, 47.04930799450051637 ) ) ;
#25164 = CARTESIAN_POINT ( 'NONE',  ( 44.70507715278255745, 25.64951373492759856, 46.92503878583764987 ) ) ;
#25165 = CIRCLE ( 'NONE', #16750, 2.499999999999997335 ) ;
#25166 = DIRECTION ( 'NONE',  ( -0.9761574614375595482, -0.2110602665713100512, -0.05069688703093144094 ) ) ;
#25167 = CARTESIAN_POINT ( 'NONE',  ( 7.782982007932094604, 15.23835801850285776, 47.04930799450052348 ) ) ;
#25168 = CARTESIAN_POINT ( 'NONE',  ( 21.09992658989239089, 29.84164230456639899, 47.04930799450051637 ) ) ;
#25169 = CIRCLE ( 'NONE', #2074, 59.80962967564905597 ) ;
#25170 = EDGE_CURVE ( 'NONE', #9845, #21115, #27319, .T. ) ;
#25171 = ORIENTED_EDGE ( 'NONE', *, *, #81, .T. ) ;
#25172 = ADVANCED_FACE ( 'NONE', ( #6690 ), #27887, .F. ) ;
#25173 = DIRECTION ( 'NONE',  ( -0.000000000000000000, -1.000000000000000000, 9.698999007525574140E-17 ) ) ;
#25174 = VECTOR ( 'NONE', #18989, 1000.000000000000000 ) ;
#25175 = VECTOR ( 'NONE', #25166, 1000.000000000000114 ) ;
#25176 = EDGE_LOOP ( 'NONE', ( #16519, #23921, #9321, #29117 ) ) ;
#25177 = CIRCLE ( 'NONE', #13626, 12.62506659569710443 ) ;
#25178 = DIRECTION ( 'NONE',  ( -1.000000000000000000, -1.101824276508909887E-16, 0.000000000000000000 ) ) ;
#25179 = FACE_OUTER_BOUND ( 'NONE', #4439, .T. ) ;
#25180 = AXIS2_PLACEMENT_3D ( 'NONE', #16115, #21516, #19214 ) ;
#25181 = CIRCLE ( 'NONE', #13665, 12.62506659569710266 ) ;
#25182 = ORIENTED_EDGE ( 'NONE', *, *, #17573, .F. ) ;
#25183 = DIRECTION ( 'NONE',  ( -0.2029548553014555723, 0.9702957262759968060, -0.1316644609608115524 ) ) ;
#25184 = ORIENTED_EDGE ( 'NONE', *, *, #6521, .T. ) ;
#25185 = DIRECTION ( 'NONE',  ( -1.000000000000000000, 0.000000000000000000, 0.000000000000000000 ) ) ;
#25186 = CARTESIAN_POINT ( 'NONE',  ( -40.18454328187963398, 7.548069831825862330, 53.80788663826320573 ) ) ;
#25187 =( BOUNDED_CURVE ( )  B_SPLINE_CURVE ( 3, ( #24744, #21938, #25068, #22107 ),
 .UNSPECIFIED., .F., .F. ) 
 B_SPLINE_CURVE_WITH_KNOTS ( ( 4, 4 ),
 ( 4.189866217988888586, 4.712388980384689674 ),
 .UNSPECIFIED. ) 
 CURVE ( )  GEOMETRIC_REPRESENTATION_ITEM ( )  RATIONAL_B_SPLINE_CURVE ( ( 1.000000000000000000, 0.9773766218953335860, 0.9773766218953335860, 1.000000000000000000 ) ) 
 REPRESENTATION_ITEM ( '' )  );
#25188 = CARTESIAN_POINT ( 'NONE',  ( -36.98761417531858342, -5.935454207752198563, 77.87546120947918382 ) ) ;
#25189 = FACE_OUTER_BOUND ( 'NONE', #16060, .T. ) ;
#25190 = EDGE_LOOP ( 'NONE', ( #10781, #8397, #16344 ) ) ;
#25191 = CARTESIAN_POINT ( 'NONE',  ( 78.96239148643020656, -5.919445383190008236, 78.27029210513457258 ) ) ;
#25192 = DIRECTION ( 'NONE',  ( 0.000000000000000000, 0.000000000000000000, -1.000000000000000000 ) ) ;
#25193 = AXIS2_PLACEMENT_3D ( 'NONE', #18737, #1679, #11702 ) ;
#25194 = CARTESIAN_POINT ( 'NONE',  ( 33.46699938050304013, 31.46183152705961561, 47.04930799450051637 ) ) ;
#25195 = CARTESIAN_POINT ( 'NONE',  ( 21.09992658989239089, 23.96664230456639899, 47.04930799450051637 ) ) ;
#25196 = CARTESIAN_POINT ( 'NONE',  ( 33.72499318558949710, 29.09184655352418858, 47.04930799450051637 ) ) ;
#25197 = VERTEX_POINT ( 'NONE', #680 ) ;
#25198 = DIRECTION ( 'NONE',  ( 2.779292025043186357E-18, -1.288349127009862211E-17, 1.000000000000000000 ) ) ;
#25199 = DIRECTION ( 'NONE',  ( -1.101824276508909887E-16, 1.000000000000000000, -0.000000000000000000 ) ) ;
#25200 = ORIENTED_EDGE ( 'NONE', *, *, #1951, .T. ) ;
#25201 = CARTESIAN_POINT ( 'NONE',  ( 47.09785597605719687, 24.86454579224779593, 47.04930799450078638 ) ) ;
#25202 = EDGE_CURVE ( 'NONE', #11589, #13067, #29404, .T. ) ;
#25203 = CIRCLE ( 'NONE', #13673, 0.1250000000000001110 ) ;
#25204 = DIRECTION ( 'NONE',  ( -1.000000000000000000, 0.000000000000000000, 0.000000000000000000 ) ) ;
#25205 = ORIENTED_EDGE ( 'NONE', *, *, #12914, .F. ) ;
#25206 = DIRECTION ( 'NONE',  ( -0.000000000000000000, -1.000000000000000000, 0.000000000000000000 ) ) ;
#25207 = TOROIDAL_SURFACE ( 'NONE', #11055, 41.50000000000000000, 1.499999999999997780 ) ;
#25208 = EDGE_LOOP ( 'NONE', ( #2097, #18411, #18508, #7371 ) ) ;
#25209 = AXIS2_PLACEMENT_3D ( 'NONE', #3047, #13084, #23078 ) ;
#25210 = CIRCLE ( 'NONE', #30437, 0.1250000000000001110 ) ;
#25211 = VERTEX_POINT ( 'NONE', #3742 ) ;
#25212 = EDGE_CURVE ( 'NONE', #29229, #2570, #23682, .T. ) ;
#25213 = EDGE_CURVE ( 'NONE', #24404, #17879, #24721, .T. ) ;
#25214 = EDGE_CURVE ( 'NONE', #21751, #6567, #19999, .T. ) ;
#25215 = EDGE_CURVE ( 'NONE', #31644, #25156, #22103, .T. ) ;
#25216 = AXIS2_PLACEMENT_3D ( 'NONE', #6691, #16686, #4235 ) ;
#25217 = DIRECTION ( 'NONE',  ( 8.659560562355045024E-17, -0.7071067811865383579, 0.7071067811865566766 ) ) ;
#25218 = CARTESIAN_POINT ( 'NONE',  ( 46.96819297411687444, 26.06988759933319244, 49.54594323136014822 ) ) ;
#25219 = ORIENTED_EDGE ( 'NONE', *, *, #23635, .T. ) ;
#25220 = VERTEX_POINT ( 'NONE', #1434 ) ;
#25221 = CARTESIAN_POINT ( 'NONE',  ( 21.09785597605719332, 11.92558985988973497, 47.04930799450051637 ) ) ;
#25222 = CARTESIAN_POINT ( 'NONE',  ( 21.09992658989238734, 31.59164230456639544, 47.04930799450051637 ) ) ;
#25223 = CARTESIAN_POINT ( 'NONE',  ( -32.36020198612200716, 0.9737162801293415271, 79.86951263711033278 ) ) ;
#25224 = DIRECTION ( 'NONE',  ( 0.000000000000000000, -0.000000000000000000, -1.000000000000000000 ) ) ;
#25225 = AXIS2_PLACEMENT_3D ( 'NONE', #25826, #15973, #5976 ) ;
#25226 = ORIENTED_EDGE ( 'NONE', *, *, #186, .F. ) ;
#25227 = CLOSED_SHELL ( 'NONE', ( #6822, #26341, #3750, #29272, #22253, #6114, #26378, #26374, #12832, #9187, #411, #26794, #23392, #20402, #13819, #15353, #14641, #7907, #21600, #6671, #8048, #3704, #19141, #21031, #25571, #6230, #29442, #9631, #21631, #30279, #24198, #27307, #28812, #16485, #12670, #27522, #26835, #21148, #8015, #16151, #19360, #31026, #15300, #18176, #11859, #23166, #30767, #29313, #12954, #2202, #4437, #26271, #21042, #8645, #16989, #5268, #11235, #19857, #9835, #21847, #10319, #32440, #27807, #18286, #9217, #19428, #21880, #27258, #24269, #26338, #24932, #2375, #8597, #32076, #8342, #18079, #25800, #28538, #30632, #27581, #4257, #986, #10827, #8946, #16433, #16356, #2562, #26860, #2114, #32259, #789, #3767, #3246, #24345, #17080, #30143, #22257, #19209, #8892, #3929, #22158, #21629, #2842, #25087, #26707, #1472, #16338, #29692, #1021, #22858, #27617, #26655, #22156, #21074, #3002, #24592, #11170, #19518, #27219, #25280, #3375, #18835, #22819, #21849, #2331, #28714, #14392, #7071, #18250, #26008, #7635, #26980, #4114, #11476, #6638, #21387, #8461, #27199, #15755, #21843, #14951, #12496, #752, #30803, #24558, #4532, #28713, #1513, #19445, #20871, #20249, #3747, #25851, #19138, #19775, #24608, #3151, #17746, #18806, #8261, #29903, #2891, #14840, #10984, #29389, #5262, #28669, #24475, #26445, #10836, #13823, #16736, #5878, #31069, #9668, #8810, #22303, #7231, #22279, #25893, #28210, #301, #813, #25084, #4494, #28033, #23071, #21555, #9886, #17496, #31823, #26606, #4835, #18964, #1443, #30588, #14071, #26897, #21559, #17442, #2777, #21464, #2161, #10585, #27350, #31792, #16001, #20679, #20032, #24891, #22246, #1982, #11009, #3165, #7908, #30396, #8176, #27717, #22794, #16339, #5868, #10254, #11667, #5541, #30814, #23967, #23783, #17594, #12872, #2030, #7653, #5231, #20303, #784, #15903, #21510, #17374, #13664, #22784, #31718, #28902, #15757, #4403, #7620, #18373, #4052, #11311, #20300, #6517, #28489, #14485, #32027, #30261, #14498, #8818, #24682, #28509, #6751, #24804, #4526, #14578, #18066, #29987, #16399, #16414, #18656, #23267, #6371, #27614, #21839, #11965, #31863, #16374, #585, #6936 ) ) ;
#25228 = CARTESIAN_POINT ( 'NONE',  ( -9.504800311772120480, 5.005525289648605991, 98.30203229136020582 ) ) ;
#25229 = ORIENTED_EDGE ( 'NONE', *, *, #24105, .F. ) ;
#25230 = LINE ( 'NONE', #5205, #29075 ) ;
#25231 = CARTESIAN_POINT ( 'NONE',  ( 79.37786958444415575, -5.721341737285090545, 15.14745076809877133 ) ) ;
#25232 = AXIS2_PLACEMENT_3D ( 'NONE', #9244, #3829, #16458 ) ;
#25233 = ORIENTED_EDGE ( 'NONE', *, *, #5833, .F. ) ;
#25234 = CARTESIAN_POINT ( 'NONE',  ( 21.09785597605720042, -13.64309448858209528, 47.04930799450051637 ) ) ;
#25235 = LINE ( 'NONE', #5052, #17878 ) ;
#25236 = FACE_OUTER_BOUND ( 'NONE', #5005, .T. ) ;
#25237 = DIRECTION ( 'NONE',  ( -1.101824276508909887E-16, 1.000000000000000000, -0.000000000000000000 ) ) ;
#25238 = DIRECTION ( 'NONE',  ( -1.000000000000000000, 0.000000000000000000, 0.000000000000000000 ) ) ;
#25239 = CARTESIAN_POINT ( 'NONE',  ( 47.20547626766766314, 26.78791119454915659, 44.97710074790751378 ) ) ;
#25240 = DIRECTION ( 'NONE',  ( 0.000000000000000000, 0.000000000000000000, 1.000000000000000000 ) ) ;
#25241 = CARTESIAN_POINT ( 'NONE',  ( 21.09785597605719332, -15.93545420775219945, -37.45069200549951915 ) ) ;
#25242 = VERTEX_POINT ( 'NONE', #11450 ) ;
#25244 = EDGE_CURVE ( 'NONE', #28626, #31841, #26302, .T. ) ;
#25243 = DIRECTION ( 'NONE',  ( 0.8746197071393926326, -0.4848096202463430537, -8.676864087101709653E-18 ) ) ;
#25245 = ORIENTED_EDGE ( 'NONE', *, *, #8385, .T. ) ;
#25246 = VECTOR ( 'NONE', #7748, 1000.000000000000000 ) ;
#25247 = EDGE_CURVE ( 'NONE', #2027, #27575, #10065, .T. ) ;
#25248 = DIRECTION ( 'NONE',  ( -1.000000000000000000, 0.000000000000000000, 0.000000000000000000 ) ) ;
#25249 = VERTEX_POINT ( 'NONE', #2577 ) ;
#25250 = VERTEX_POINT ( 'NONE', #19639 ) ;
#25251 = DIRECTION ( 'NONE',  ( -0.6184495258776567805, 0.3428121700606641120, 0.7071067811865474617 ) ) ;
#25252=STYLED_ITEM('',(#32529),#1854);
#25253 = ORIENTED_EDGE ( 'NONE', *, *, #21112, .F. ) ;
#25254 = CIRCLE ( 'NONE', #19994, 12.36707279061065101 ) ;
#25255 = EDGE_CURVE ( 'NONE', #1311, #21016, #10578, .T. ) ;
#25256 = EDGE_LOOP ( 'NONE', ( #3951, #30894, #23864, #8762, #15244, #29268, #15038, #24226 ) ) ;
#25257 = CARTESIAN_POINT ( 'NONE',  ( 46.04327488119035650, 22.93807716476589675, 48.37782978030396208 ) ) ;
#25258 = ORIENTED_EDGE ( 'NONE', *, *, #31685, .T. ) ;
#25259 = CARTESIAN_POINT ( 'NONE',  ( -4.902144023942810236, 24.86454579224779948, 44.54930799450078638 ) ) ;
#25260 = CARTESIAN_POINT ( 'NONE',  ( 47.78944874062793247, 29.51560991843770765, 45.00889955171861345 ) ) ;
#25261 = FACE_OUTER_BOUND ( 'NONE', #31683, .T. ) ;
#25262 = ADVANCED_FACE ( 'NONE', ( #4886 ), #32374, .F. ) ;
#25263 = CARTESIAN_POINT ( 'NONE',  ( 44.74832014356462651, 29.78456182964375643, 46.92728461490987257 ) ) ;
#25264 = ORIENTED_EDGE ( 'NONE', *, *, #16842, .F. ) ;
#25265 = ORIENTED_EDGE ( 'NONE', *, *, #1338, .F. ) ;
#25266 = CARTESIAN_POINT ( 'NONE',  ( 21.09785597605719332, 25.56454579224779877, 59.04930799450051637 ) ) ;
#25267 = VERTEX_POINT ( 'NONE', #10138 ) ;
#25268 = ADVANCED_FACE ( 'NONE', ( #22268 ), #25066, .F. ) ;
#25269 = DIRECTION ( 'NONE',  ( -1.344306794811909313E-16, 1.000000000000000000, 1.759793992609926301E-18 ) ) ;
#25270 = CONICAL_SURFACE ( 'NONE', #14191, 12.52247886585643499, 0.6248499269447925775 ) ;
#25271 = CARTESIAN_POINT ( 'NONE',  ( 54.44545748192361145, -4.258649047046827896, 103.5750977336757188 ) ) ;
#25272 = CARTESIAN_POINT ( 'NONE',  ( -40.68642432603679282, 6.803331639905807471, 34.75772891228915285 ) ) ;
#25273 = AXIS2_PLACEMENT_3D ( 'NONE', #21539, #26321, #11228 ) ;
#25274 = CARTESIAN_POINT ( 'NONE',  ( 52.94504501510867556, -5.721341737285968065, -11.26059709029990330 ) ) ;
#25275 = CARTESIAN_POINT ( 'NONE',  ( -40.47970302497625994, 7.463434137431151250, 60.44930799450051495 ) ) ;
#25276 = APPLICATION_PROTOCOL_DEFINITION ( 'draft international standard', 'automotive_design', 1998, #20836 ) ;
#25277 = ORIENTED_EDGE ( 'NONE', *, *, #14034, .T. ) ;
#25278 = VERTEX_POINT ( 'NONE', #22105 ) ;
#25279 = DIRECTION ( 'NONE',  ( -1.000000000000000000, 0.000000000000000000, 0.000000000000000000 ) ) ;
#25280 = ADVANCED_FACE ( 'NONE', ( #19971 ), #30001, .T. ) ;
#25281 = CARTESIAN_POINT ( 'NONE',  ( 46.96819297411687444, 28.99253733014355561, 49.54594323136014822 ) ) ;
#25282 = EDGE_CURVE ( 'NONE', #12063, #13560, #18932, .T. ) ;
#25283 = EDGE_CURVE ( 'NONE', #8390, #3586, #4805, .T. ) ;
#25284 = FACE_OUTER_BOUND ( 'NONE', #6704, .T. ) ;
#25285 = EDGE_LOOP ( 'NONE', ( #21101, #28969, #29355, #8195 ) ) ;
#25286 = CARTESIAN_POINT ( 'NONE',  ( 45.79384627280941089, 27.86618040159426357, 49.05938063676250493 ) ) ;
#25287 = ORIENTED_EDGE ( 'NONE', *, *, #30507, .F. ) ;
#25288 = CARTESIAN_POINT ( 'NONE',  ( 44.79156314060809763, 19.96454579224779380, 46.92953032342012420 ) ) ;
#25289 = CARTESIAN_POINT ( 'NONE',  ( 21.09992658989238734, 38.56284415653841791, 47.04930799450051637 ) ) ;
#25290 = AXIS2_PLACEMENT_3D ( 'NONE', #562, #20098, #2705 ) ;
#25291 = AXIS2_PLACEMENT_3D ( 'NONE', #6731, #24125, #6900 ) ;
#25292 = EDGE_CURVE ( 'NONE', #23085, #28525, #12698, .T. ) ;
#25293 = AXIS2_PLACEMENT_3D ( 'NONE', #7054, #16566, #32003 ) ;
#25294 = ORIENTED_EDGE ( 'NONE', *, *, #15239, .F. ) ;
#25295 = AXIS2_PLACEMENT_3D ( 'NONE', #12859, #27784, #364 ) ;
#25296 = VERTEX_POINT ( 'NONE', #117 ) ;
#25297 = SPHERICAL_SURFACE ( 'NONE', #3888, 0.1000000000000000056 ) ;
#25298 = LINE ( 'NONE', #18210, #29730 ) ;
#25299 = CARTESIAN_POINT ( 'NONE',  ( 48.18662509608405031, 25.18284706826093355, 49.18364984542562013 ) ) ;
#25300 = ORIENTED_EDGE ( 'NONE', *, *, #6772, .T. ) ;
#25301 = CARTESIAN_POINT ( 'NONE',  ( -29.27613032885505007, -4.281517947942904634, 80.46297774100551692 ) ) ;
#25302 = CARTESIAN_POINT ( 'NONE',  ( 81.58034905098003264, -5.935653941159266367, 16.06701660332827331 ) ) ;
#25303 = CARTESIAN_POINT ( 'NONE',  ( 21.09785597605719332, 15.24673779880127356, 60.53344952167864790 ) ) ;
#25304 = EDGE_CURVE ( 'NONE', #14245, #23467, #31025, .T. ) ;
#25305 = DIRECTION ( 'NONE',  ( 1.234978253042719660E-16, -1.000000000000000000, -1.109335647967047851E-31 ) ) ;
#25306 = ADVANCED_FACE ( 'NONE', ( #16858 ), #15812, .F. ) ;
#25307 = CARTESIAN_POINT ( 'NONE',  ( -41.94956971822180947, 3.905757428664828890, 47.04930799450051637 ) ) ;
#25308 = DIRECTION ( 'NONE',  ( -1.101824276508909887E-16, 1.000000000000000000, -0.000000000000000000 ) ) ;
#25309 = DIRECTION ( 'NONE',  ( -1.101824276508909887E-16, 1.000000000000000000, -0.000000000000000000 ) ) ;
#25310 = CARTESIAN_POINT ( 'NONE',  ( 21.09785597605719332, 24.56454579224780232, 47.04930799450051637 ) ) ;
#25311 = CARTESIAN_POINT ( 'NONE',  ( 21.09992658989238734, 38.56284415653841791, 47.04930799450051637 ) ) ;
#25312 = CIRCLE ( 'NONE', #10642, 0.1250000000000001110 ) ;
#25313 = FACE_OUTER_BOUND ( 'NONE', #24265, .T. ) ;
#25314 = ORIENTED_EDGE ( 'NONE', *, *, #25664, .F. ) ;
#25315 = ORIENTED_EDGE ( 'NONE', *, *, #29199, .F. ) ;
#25316 = CARTESIAN_POINT ( 'NONE',  ( -40.02540636251513462, 2.839176264122873050, 37.04930799450052348 ) ) ;
#25317 = DIRECTION ( 'NONE',  ( -3.761114140369701376E-15, -1.000000000000000000, -0.000000000000000000 ) ) ;
#25318 = EDGE_CURVE ( 'NONE', #9202, #31146, #28403, .T. ) ;
#25319 = CARTESIAN_POINT ( 'NONE',  ( 21.09992658989239089, 24.72145308207319303, 47.04930799450051637 ) ) ;
#25320 = EDGE_CURVE ( 'NONE', #27962, #32074, #9486, .T. ) ;
#25321 = CARTESIAN_POINT ( 'NONE',  ( -39.44363481821952888, 3.888719912690147940, 57.04930799450051637 ) ) ;
#25322 = ORIENTED_EDGE ( 'NONE', *, *, #12573, .T. ) ;
#25323 = TOROIDAL_SURFACE ( 'NONE', #30551, 12.40141737965286772, 0.1250000000000003331 ) ;
#25324 = CARTESIAN_POINT ( 'NONE',  ( -39.46567364092025798, -5.935459928907636851, 77.98438527425163613 ) ) ;
#25325 = CARTESIAN_POINT ( 'NONE',  ( 21.09992658989239089, 28.59164230456639544, 47.04930799450051637 ) ) ;
#25326 = LINE ( 'NONE', #2829, #7323 ) ;
#25327 = ORIENTED_EDGE ( 'NONE', *, *, #27999, .F. ) ;
#25328 = ORIENTED_EDGE ( 'NONE', *, *, #1816, .T. ) ;
#25329 = LINE ( 'NONE', #25486, #27809 ) ;
#25330 = CARTESIAN_POINT ( 'NONE',  ( 48.83862994770794330, 27.34118040159426499, 48.17861352429476796 ) ) ;
#25331 = CARTESIAN_POINT ( 'NONE',  ( 48.40186567930498285, 29.52957786121581307, 45.03923535223908203 ) ) ;
#25332 = CARTESIAN_POINT ( 'NONE',  ( -39.45090951743608088, -5.935454519444268051, 77.98460375324034999 ) ) ;
#25333 = FACE_OUTER_BOUND ( 'NONE', #6856, .T. ) ;
#25334 = ORIENTED_EDGE ( 'NONE', *, *, #9964, .T. ) ;
#25335 = CIRCLE ( 'NONE', #6959, 0.1250000000000001110 ) ;
#25336 = CIRCLE ( 'NONE', #11696, 2.000000000000001776 ) ;
#25337 = DIRECTION ( 'NONE',  ( -1.224646799147353207E-16, 0.000000000000000000, -1.000000000000000000 ) ) ;
#25338 = EDGE_LOOP ( 'NONE', ( #1060, #638, #11870, #30556 ) ) ;
#25339 = CIRCLE ( 'NONE', #30596, 0.2999999999999947153 ) ;
#25340 = AXIS2_PLACEMENT_3D ( 'NONE', #21133, #3749, #30849 ) ;
#25341 = CARTESIAN_POINT ( 'NONE',  ( 21.09785597605720042, -5.986312001189870280, 114.4134811058426209 ) ) ;
#25342 = CARTESIAN_POINT ( 'NONE',  ( 21.09785597605719332, 25.56454579224779167, 73.04930799450052348 ) ) ;
#25343 = ORIENTED_EDGE ( 'NONE', *, *, #20966, .F. ) ;
#25344 = DIRECTION ( 'NONE',  ( -0.000000000000000000, 1.000000000000000000, -0.000000000000000000 ) ) ;
#25345 = EDGE_LOOP ( 'NONE', ( #4948, #5804, #17593 ) ) ;
#25346 = CARTESIAN_POINT ( 'NONE',  ( 21.09992658989239089, 25.84164230456639899, 47.04930799450051637 ) ) ;
#25347 = LINE ( 'NONE', #22877, #23052 ) ;
#25348 = CYLINDRICAL_SURFACE ( 'NONE', #7944, 21.50000000000000000 ) ;
#25349 = PLANE ( 'NONE',  #22844 ) ;
#25350 = ORIENTED_EDGE ( 'NONE', *, *, #24831, .F. ) ;
#25351 = DIRECTION ( 'NONE',  ( 0.000000000000000000, 0.000000000000000000, -1.000000000000000000 ) ) ;
#25352 = DIRECTION ( 'NONE',  ( 0.2756373558169932236, -0.9612616959383204485, 1.479773560108267395E-16 ) ) ;
#25353 = CARTESIAN_POINT ( 'NONE',  ( 81.54614529590624272, -5.936959954202220224, 77.95369730613863624 ) ) ;
#25354 = EDGE_CURVE ( 'NONE', #3682, #180, #14547, .T. ) ;
#25355 = CARTESIAN_POINT ( 'NONE',  ( -37.49824857498671093, 12.70128680827697387, 56.14611646155296398 ) ) ;
#25356 = EDGE_CURVE ( 'NONE', #19002, #16387, #23146, .T. ) ;
#25357 = CIRCLE ( 'NONE', #6470, 0.1000000000000014905 ) ;
#25358 = EDGE_CURVE ( 'NONE', #1567, #4768, #17922, .T. ) ;
#25359 = DIRECTION ( 'NONE',  ( 7.588956326749211550E-18, -4.206627182996911684E-18, 1.000000000000000000 ) ) ;
#25360 = VERTEX_POINT ( 'NONE', #15697 ) ;
#25361 = CARTESIAN_POINT ( 'NONE',  ( 21.09785597605719332, -19.93545420775220123, 47.04930799450051637 ) ) ;
#25362 = DIRECTION ( 'NONE',  ( 1.000000000000000000, 0.000000000000000000, 0.000000000000000000 ) ) ;
#25363 = VERTEX_POINT ( 'NONE', #5867 ) ;
#25364 = CARTESIAN_POINT ( 'NONE',  ( -10.80400125034478087, -5.721341737285083440, -11.23070561388631816 ) ) ;
#25365 = DIRECTION ( 'NONE',  ( 0.4544104193609900810, 0.000000000000000000, 0.8907924397839089847 ) ) ;
#25366 = CARTESIAN_POINT ( 'NONE',  ( 33.46699938050304013, 24.96183152705960140, 47.04930799450051637 ) ) ;
#25367 = TOROIDAL_SURFACE ( 'NONE', #16421, 22.69860022854976123, 0.2999999999999999889 ) ;
#25368 = ORIENTED_EDGE ( 'NONE', *, *, #3361, .T. ) ;
#25369 = CIRCLE ( 'NONE', #17492, 0.1000000000000028644 ) ;
#25370 = DIRECTION ( 'NONE',  ( -0.7141240004913222972, 0.3958453973320028019, 0.5773502691896303940 ) ) ;
#25371 = ORIENTED_EDGE ( 'NONE', *, *, #24553, .F. ) ;
#25372 = VERTEX_POINT ( 'NONE', #25872 ) ;
#25373 = AXIS2_PLACEMENT_3D ( 'NONE', #29878, #5085, #7059 ) ;
#25374 = DIRECTION ( 'NONE',  ( 0.8746197071393858602, -0.4848096202463547666, 0.000000000000000000 ) ) ;
#25375 = CYLINDRICAL_SURFACE ( 'NONE', #32410, 40.00000000000000711 ) ;
#25376 = EDGE_LOOP ( 'NONE', ( #30355, #28589, #6299, #29542 ) ) ;
#25377 = ORIENTED_EDGE ( 'NONE', *, *, #19135, .T. ) ;
#25378 = CARTESIAN_POINT ( 'NONE',  ( 47.79865503179234310, 9.702389020015065313, -4.315940132965163656 ) ) ;
#25379 = CARTESIAN_POINT ( 'NONE',  ( -37.58300281841709989, 16.01180101885526597, 36.00717268343339583 ) ) ;
#25380 = CARTESIAN_POINT ( 'NONE',  ( -36.31527284916851528, -5.096557943222667753, 79.79328601240887053 ) ) ;
#25381 = CARTESIAN_POINT ( 'NONE',  ( 52.07598125402753197, -5.935454207809698346, -13.48459002699794063 ) ) ;
#25382 = VERTEX_POINT ( 'NONE', #10944 ) ;
#25383 = DIRECTION ( 'NONE',  ( 0.2756373558169974980, -0.9612616959383193382, 8.979771562518858393E-33 ) ) ;
#25384 = ORIENTED_EDGE ( 'NONE', *, *, #860, .F. ) ;
#25385 = FACE_OUTER_BOUND ( 'NONE', #4621, .T. ) ;
#25386 = LINE ( 'NONE', #17513, #25820 ) ;
#25387 = EDGE_LOOP ( 'NONE', ( #6168, #16720, #8156, #23049 ) ) ;
#25388 = CARTESIAN_POINT ( 'NONE',  ( 47.45244889970129520, 23.03451764446790051, 45.89330396155958169 ) ) ;
#25389 = ADVANCED_FACE ( 'NONE', ( #5209 ), #25549, .F. ) ;
#25390 = DIRECTION ( 'NONE',  ( -1.101824276508909887E-16, 1.000000000000000000, -0.000000000000000000 ) ) ;
#25391 = ADVANCED_FACE ( 'NONE', ( #3223 ), #920, .F. ) ;
#25392 = EDGE_CURVE ( 'NONE', #21602, #18307, #7678, .T. ) ;
#25393 = CARTESIAN_POINT ( 'NONE',  ( 48.83862994770794330, 27.25457786121582160, 48.17861352429476796 ) ) ;
#25394 = EDGE_CURVE ( 'NONE', #23085, #7990, #15538, .T. ) ;
#25395 = FACE_BOUND ( 'NONE', #11826, .T. ) ;
#25396 = CARTESIAN_POINT ( 'NONE',  ( 21.09785597605719332, 16.33322284159648063, 47.04930799450051637 ) ) ;
#25397 = ADVANCED_FACE ( 'NONE', ( #15218 ), #14249, .T. ) ;
#25398 = EDGE_CURVE ( 'NONE', #5228, #3250, #2725, .T. ) ;
#25399 = ORIENTED_EDGE ( 'NONE', *, *, #4149, .T. ) ;
#25400 = CARTESIAN_POINT ( 'NONE',  ( 8.577447724035948795, 32.54735957529758394, 47.04930799450051637 ) ) ;
#25401 = ORIENTED_EDGE ( 'NONE', *, *, #3519, .F. ) ;
#25402 = CARTESIAN_POINT ( 'NONE',  ( 45.52675994804781112, 28.23420399681022275, 49.47108226228596806 ) ) ;
#25403 = EDGE_LOOP ( 'NONE', ( #20762, #15140, #20851, #31318 ) ) ;
#25404 = AXIS2_PLACEMENT_3D ( 'NONE', #16119, #30598, #23357 ) ;
#25405 = AXIS2_PLACEMENT_3D ( 'NONE', #23325, #28252, #836 ) ;
#25406 = ORIENTED_EDGE ( 'NONE', *, *, #8139, .T. ) ;
#25407 = CARTESIAN_POINT ( 'NONE',  ( 21.09992658989238734, 31.96664230456639544, 47.04930799450051637 ) ) ;
#25408 = CIRCLE ( 'NONE', #21711, 2.000000000000000000 ) ;
#25409 = CIRCLE ( 'NONE', #11249, 12.62506659569710443 ) ;
#25410 = TOROIDAL_SURFACE ( 'NONE', #3917, 18.86195243859455672, 0.5000000000000000000 ) ;
#25411 = TOROIDAL_SURFACE ( 'NONE', #6008, 32.50000000000000000, 1.499999999999999556 ) ;
#25412 = ORIENTED_EDGE ( 'NONE', *, *, #21958, .F. ) ;
#25413 = ORIENTED_EDGE ( 'NONE', *, *, #17245, .F. ) ;
#25414 = CARTESIAN_POINT ( 'NONE',  ( 21.09992658989239089, 28.84164230456639544, 47.04930799450051637 ) ) ;
#25415 = ADVANCED_FACE ( 'NONE', ( #23086 ), #25767, .T. ) ;
#25416 = ORIENTED_EDGE ( 'NONE', *, *, #32207, .F. ) ;
#25417 = VECTOR ( 'NONE', #26747, 1000.000000000000000 ) ;
#25418 = DIRECTION ( 'NONE',  ( -1.000000000000000000, 0.000000000000000000, 0.000000000000000000 ) ) ;
#25419 = CARTESIAN_POINT ( 'NONE',  ( -42.50976151518963064, 14.59907569580870046, 37.04930799450052348 ) ) ;
#25420 = DIRECTION ( 'NONE',  ( 0.9612616959383198934, 0.2756373558169956106, 0.000000000000000000 ) ) ;
#25421 = TOROIDAL_SURFACE ( 'NONE', #21726, 12.61792373059858896, 0.1250000000000002220 ) ;
#25422 = CARTESIAN_POINT ( 'NONE',  ( 48.83862994770794330, 26.55457786121582231, 48.17861352429476796 ) ) ;
#25423 = VERTEX_POINT ( 'NONE', #10792 ) ;
#25424 = ORIENTED_EDGE ( 'NONE', *, *, #19205, .F. ) ;
#25426 = DIRECTION ( 'NONE',  ( -1.000000000000000000, 0.000000000000000000, 0.000000000000000000 ) ) ;
#25425 = CIRCLE ( 'NONE', #6053, 0.1000000000000013517 ) ;
#25427 = TOROIDAL_SURFACE ( 'NONE', #15476, 1.899999999999999467, 0.1000000000000000056 ) ;
#25428 = ORIENTED_EDGE ( 'NONE', *, *, #13716, .T. ) ;
#25429 = DIRECTION ( 'NONE',  ( 0.000000000000000000, 0.000000000000000000, 1.000000000000000000 ) ) ;
#25430 = TOROIDAL_SURFACE ( 'NONE', #11283, 12.40141737965283397, 0.1249999999999992922 ) ;
#25431 = CARTESIAN_POINT ( 'NONE',  ( 100.3079064823960493, -15.93545420775219945, 49.54930799450134771 ) ) ;
#25432 = CARTESIAN_POINT ( 'NONE',  ( -40.21210701746133509, 7.644196001419694575, 53.64930799450051779 ) ) ;
#25433 = CARTESIAN_POINT ( 'NONE',  ( 47.19823469859255738, 22.88065857334294861, 45.11653766655789610 ) ) ;
#25434 = CARTESIAN_POINT ( 'NONE',  ( 8.732853799281738105, 27.96183152705961206, 47.04930799450051637 ) ) ;
#25435 = EDGE_CURVE ( 'NONE', #28743, #31649, #11619, .T. ) ;
#25436 = EDGE_LOOP ( 'NONE', ( #18331, #6113 ) ) ;
#25437 = CARTESIAN_POINT ( 'NONE',  ( -40.73091736380679606, 9.483895492497154578, 38.64930799450052490 ) ) ;
#25438 = CARTESIAN_POINT ( 'NONE',  ( -40.69193635511749108, 9.347952559758585522, 39.44930799450052206 ) ) ;
#25439 = CARTESIAN_POINT ( 'NONE',  ( -9.806533335581546496, -5.936959954202215783, 107.4975973143492212 ) ) ;
#25440 = CARTESIAN_POINT ( 'NONE',  ( 48.18662509608405742, 27.28284706826093142, 49.18364984542562013 ) ) ;
#25441 = ORIENTED_EDGE ( 'NONE', *, *, #2432, .T. ) ;
#25442 = CARTESIAN_POINT ( 'NONE',  ( 21.09992658989238734, 38.56284415653841791, 47.04930799450051637 ) ) ;
#25443 = PLANE ( 'NONE',  #20348 ) ;
#25444 = APPLICATION_CONTEXT ( 'automotive_design' ) ;
#25445 = CARTESIAN_POINT ( 'NONE',  ( -40.70484894842233103, 8.274204744976163539, 59.64930799450051779 ) ) ;
#25446 = VECTOR ( 'NONE', #14605, 1000.000000000000227 ) ;
#25447 = ADVANCED_FACE ( 'NONE', ( #30802 ), #28922, .T. ) ;
#25448 = AXIS2_PLACEMENT_3D ( 'NONE', #16212, #6535, #11148 ) ;
#25449 = AXIS2_PLACEMENT_3D ( 'NONE', #6289, #876, #16294 ) ;
#25450 = ADVANCED_FACE ( 'NONE', ( #22761 ), #5125, .T. ) ;
#25451 = AXIS2_PLACEMENT_3D ( 'NONE', #11895, #24036, #6808 ) ;
#25452 = ORIENTED_EDGE ( 'NONE', *, *, #17465, .F. ) ;
#25453 = VERTEX_POINT ( 'NONE', #31131 ) ;
#25454 = DIRECTION ( 'NONE',  ( 0.000000000000000000, 0.000000000000000000, -1.000000000000000000 ) ) ;
#25455 = EDGE_CURVE ( 'NONE', #11782, #1013, #13206, .T. ) ;
#25456 = DIRECTION ( 'NONE',  ( -1.101824276508909887E-16, 1.000000000000000000, -0.000000000000000000 ) ) ;
#25457 = LINE ( 'NONE', #30713, #29363 ) ;
#25458 = ADVANCED_FACE ( 'NONE', ( #8641 ), #24045, .F. ) ;
#25459 = TOROIDAL_SURFACE ( 'NONE', #29653, 12.40141737965287128, 0.1249999999999993477 ) ;
#25460 = ORIENTED_EDGE ( 'NONE', *, *, #20157, .F. ) ;
#25461 = CARTESIAN_POINT ( 'NONE',  ( -40.16503835899720087, 7.510440877657817538, 35.29832907986742185 ) ) ;
#25462 = CARTESIAN_POINT ( 'NONE',  ( 21.09785597605719332, 25.56454579224780232, -34.66074251183835031 ) ) ;
#25463 = PLANE ( 'NONE',  #13787 ) ;
#25464 = DIRECTION ( 'NONE',  ( -0.000000000000000000, -1.000000000000000000, -0.000000000000000000 ) ) ;
#25465 = DIRECTION ( 'NONE',  ( -1.000000000000000000, -0.000000000000000000, -3.491481338843133355E-15 ) ) ;
#25466 = LINE ( 'NONE', #18222, #22277 ) ;
#25467 = FACE_OUTER_BOUND ( 'NONE', #30330, .T. ) ;
#25468 = CARTESIAN_POINT ( 'NONE',  ( 21.09992658989238734, 38.56284415653841791, 47.04930799450051637 ) ) ;
#25469 = DIRECTION ( 'NONE',  ( -1.101824276508909887E-16, 1.000000000000000000, -0.000000000000000000 ) ) ;
#25470 = CARTESIAN_POINT ( 'NONE',  ( 45.73035263060504718, 28.63954579807170475, 44.36855633853329550 ) ) ;
#25471 = ADVANCED_FACE ( 'NONE', ( #11265 ), #98, .T. ) ;
#25472 = ORIENTED_EDGE ( 'NONE', *, *, #23971, .T. ) ;
#25473 = ORIENTED_EDGE ( 'NONE', *, *, #13246, .F. ) ;
#25474 = LINE ( 'NONE', #21017, #12928 ) ;
#25475 = CIRCLE ( 'NONE', #21278, 0.1250000000000001110 ) ;
#25476 = AXIS2_PLACEMENT_3D ( 'NONE', #21823, #16571, #21492 ) ;
#25477 = CARTESIAN_POINT ( 'NONE',  ( 49.53646239908485427, 24.96864685363938818, 46.22604428272304489 ) ) ;
#25478 = CARTESIAN_POINT ( 'NONE',  ( 8.474859994195282908, 38.56284415653841791, 47.04930799450051637 ) ) ;
#25479 = CARTESIAN_POINT ( 'NONE',  ( -36.59542768321662720, 12.56771722797891400, 36.00717268343339583 ) ) ;
#25480 = ORIENTED_EDGE ( 'NONE', *, *, #30512, .T. ) ;
#25481 = DIRECTION ( 'NONE',  ( -0.000000000000000000, -1.000000000000000000, 0.000000000000000000 ) ) ;
#25482 = FACE_OUTER_BOUND ( 'NONE', #18471, .T. ) ;
#25483 = CARTESIAN_POINT ( 'NONE',  ( -24.90080973260340613, 13.80129159329807287, 47.04930799450052348 ) ) ;
#25484 = ORIENTED_EDGE ( 'NONE', *, *, #11653, .T. ) ;
#25485 = ORIENTED_EDGE ( 'NONE', *, *, #5597, .F. ) ;
#25486 = CARTESIAN_POINT ( 'NONE',  ( -40.61178118339597631, 9.038025460530262123, 57.95249952744806166 ) ) ;
#25487 = CARTESIAN_POINT ( 'NONE',  ( 45.35708200440645044, 27.69118040159426286, 45.92000246470679770 ) ) ;
#25488 = CARTESIAN_POINT ( 'NONE',  ( 49.49063479933183629, 29.41291119454914593, 47.17357720316391578 ) ) ;
#25489 = AXIS2_PLACEMENT_3D ( 'NONE', #11889, #26824, #12225 ) ;
#25490 = CARTESIAN_POINT ( 'NONE',  ( -34.31970563170440158, 11.92558985988973497, 54.04930799450052348 ) ) ;
#25491 = EDGE_CURVE ( 'NONE', #13589, #25773, #1660, .T. ) ;
#25492 = EDGE_CURVE ( 'NONE', #23355, #13639, #18632, .T. ) ;
#25493 = VERTEX_POINT ( 'NONE', #18949 ) ;
#25494 = CYLINDRICAL_SURFACE ( 'NONE', #24546, 12.62506659569710443 ) ;
#25495 = AXIS2_PLACEMENT_3D ( 'NONE', #19195, #16905, #6418 ) ;
#25496 = CARTESIAN_POINT ( 'NONE',  ( 47.40175035182062402, 22.86454579224780659, 49.06778623913097448 ) ) ;
#25497 = ORIENTED_EDGE ( 'NONE', *, *, #12628, .T. ) ;
#25498 = EDGE_CURVE ( 'NONE', #18486, #7700, #5357, .T. ) ;
#25499 = ORIENTED_EDGE ( 'NONE', *, *, #3666, .T. ) ;
#25500 = ADVANCED_FACE ( 'NONE', ( #11414 ), #13566, .T. ) ;
#25501 = CARTESIAN_POINT ( 'NONE',  ( -43.38408989745150990, 1.111547985471239786, 60.44930799450051495 ) ) ;
#25502 = CARTESIAN_POINT ( 'NONE',  ( 8.732853799281734553, 30.22145308207317527, 47.04930799450051637 ) ) ;
#25503 = CIRCLE ( 'NONE', #11354, 12.62506659569710266 ) ;
#25504 = EDGE_LOOP ( 'NONE', ( #16350, #26034, #11544, #17275 ) ) ;
#25505 = DIRECTION ( 'NONE',  ( 0.2756373558170082672, -0.9612616959383162296, 0.000000000000000000 ) ) ;
#25506 = CARTESIAN_POINT ( 'NONE',  ( 8.482002859293423569, 26.71664230456639899, 47.04930799450051637 ) ) ;
#25507 = CARTESIAN_POINT ( 'NONE',  ( -39.67555847965937943, 2.645252416024336028, 48.24930799450051211 ) ) ;
#25508 = CARTESIAN_POINT ( 'NONE',  ( 33.46699938050304013, 30.72145308207317882, 47.04930799450050927 ) ) ;
#25509 = CARTESIAN_POINT ( 'NONE',  ( -43.73393778030726509, 1.305471833569777695, 60.44930799450051495 ) ) ;
#25510 = EDGE_LOOP ( 'NONE', ( #5727, #6294, #14717, #826 ) ) ;
#25511 = CARTESIAN_POINT ( 'NONE',  ( 75.60381228737249160, -2.946992577399056845, 80.78646212873525201 ) ) ;
#25512 = CYLINDRICAL_SURFACE ( 'NONE', #9996, 21.50000000000000000 ) ;
#25513 = DIRECTION ( 'NONE',  ( 0.8746197071393926326, -0.4848096202463430537, -8.676864087101709653E-18 ) ) ;
#25514 = CARTESIAN_POINT ( 'NONE',  ( 64.09785597605721819, 14.86454579224779948, 47.04930799450051637 ) ) ;
#25515 = CARTESIAN_POINT ( 'NONE',  ( 77.26108931935814894, -3.866180060838781074, 80.58188637928151365 ) ) ;
#25516 = ORIENTED_EDGE ( 'NONE', *, *, #21431, .F. ) ;
#25517 = DIRECTION ( 'NONE',  ( -1.101824276508909887E-16, 1.000000000000000000, -0.000000000000000000 ) ) ;
#25518 = CARTESIAN_POINT ( 'NONE',  ( 21.09785597605719332, -9.935454207752199451, 47.04930799450051637 ) ) ;
#25519 = ORIENTED_EDGE ( 'NONE', *, *, #17465, .T. ) ;
#25520 = DIRECTION ( 'NONE',  ( 0.000000000000000000, 0.000000000000000000, -1.000000000000000000 ) ) ;
#25521 = DIRECTION ( 'NONE',  ( -1.000000000000000000, 0.000000000000000000, 0.000000000000000000 ) ) ;
#25522 = AXIS2_PLACEMENT_3D ( 'NONE', #8360, #10680, #20668 ) ;
#25523 = CYLINDRICAL_SURFACE ( 'NONE', #11509, 12.36707279061065101 ) ;
#25524 = DIRECTION ( 'NONE',  ( -1.000000000000000000, -1.101824276508909887E-16, 0.000000000000000000 ) ) ;
#25525 = ORIENTED_EDGE ( 'NONE', *, *, #30185, .T. ) ;
#25526 = CARTESIAN_POINT ( 'NONE',  ( 48.73394074504988538, 22.89977464660286444, 47.94256374451057212 ) ) ;
#25527 = ORIENTED_EDGE ( 'NONE', *, *, #5035, .T. ) ;
#25528 = EDGE_CURVE ( 'NONE', #7551, #28083, #31559, .T. ) ;
#25529 = VECTOR ( 'NONE', #5279, 1000.000000000000000 ) ;
#25530 = ADVANCED_FACE ( 'NONE', ( #6331 ), #2204, .F. ) ;
#25531 = ORIENTED_EDGE ( 'NONE', *, *, #17297, .T. ) ;
#25532 = EDGE_CURVE ( 'NONE', #27995, #13414, #15324, .T. ) ;
#25533 = DIRECTION ( 'NONE',  ( -1.000000000000000000, -1.101824276508909887E-16, 0.000000000000000000 ) ) ;
#25534 = CARTESIAN_POINT ( 'NONE',  ( -9.801550764381037339, -5.936960083300406588, 107.7467107960321329 ) ) ;
#25535 = DIRECTION ( 'NONE',  ( -1.000000000000000000, 0.000000000000000000, 0.000000000000000000 ) ) ;
#25536 = AXIS2_PLACEMENT_3D ( 'NONE', #1049, #11075, #18440 ) ;
#25537 = ORIENTED_EDGE ( 'NONE', *, *, #5317, .T. ) ;
#25538 = EDGE_LOOP ( 'NONE', ( #30837, #23368, #21756, #18726 ) ) ;
#25539 = CARTESIAN_POINT ( 'NONE',  ( -4.902144023942810236, 30.56454579224779522, 44.54930799450042400 ) ) ;
#25540 = CARTESIAN_POINT ( 'NONE',  ( -42.38687957179150345, 4.148162238788003719, 55.14930799450051779 ) ) ;
#25541 = VECTOR ( 'NONE', #16611, 1000.000000000000000 ) ;
#25542 = DIRECTION ( 'NONE',  ( 0.000000000000000000, 0.000000000000000000, 1.000000000000000000 ) ) ;
#25543 = VERTEX_POINT ( 'NONE', #31287 ) ;
#25544 = CARTESIAN_POINT ( 'NONE',  ( 47.09785597605719687, 15.77906836436399374, 47.04930799450078638 ) ) ;
#25545 = ORIENTED_EDGE ( 'NONE', *, *, #30221, .T. ) ;
#25546 = FACE_BOUND ( 'NONE', #10023, .T. ) ;
#25547 = DIRECTION ( 'NONE',  ( -0.000000000000000000, -1.000000000000000000, -0.000000000000000000 ) ) ;
#25548 = ORIENTED_EDGE ( 'NONE', *, *, #29084, .F. ) ;
#25549 = CYLINDRICAL_SURFACE ( 'NONE', #6370, 2.499999999999998668 ) ;
#25550 = CARTESIAN_POINT ( 'NONE',  ( 81.68751454973200055, -5.936602078651308290, 15.96907019450728349 ) ) ;
#25551 = DIRECTION ( 'NONE',  ( 0.000000000000000000, 0.000000000000000000, 1.000000000000000000 ) ) ;
#25552 = DIRECTION ( 'NONE',  ( 0.000000000000000000, 1.000000000000000000, 0.000000000000000000 ) ) ;
#25553 = CARTESIAN_POINT ( 'NONE',  ( 33.46699938050303302, 38.56284415653841791, 47.04930799450051637 ) ) ;
#25554 = CARTESIAN_POINT ( 'NONE',  ( 48.23388202445966044, 28.92822092656773947, 49.27628909396054979 ) ) ;
#25555 = CARTESIAN_POINT ( 'NONE',  ( 21.09992658989239089, 25.59143805560860940, 47.04930799450051637 ) ) ;
#25556 = EDGE_LOOP ( 'NONE', ( #24737, #18172, #30321, #25384 ) ) ;
#25557 = CARTESIAN_POINT ( 'NONE',  ( 67.84785597605720397, 13.61454579224779771, 47.04930799450051637 ) ) ;
#25558 = CARTESIAN_POINT ( 'NONE',  ( 44.87087493598345134, 28.17587066347689273, 48.18533415931919706 ) ) ;
#25559 = EDGE_LOOP ( 'NONE', ( #2044, #17768, #29652, #22621 ) ) ;
#25560 = EDGE_LOOP ( 'NONE', ( #23102, #26610, #15815, #9386, #17906 ) ) ;
#25561 = FACE_OUTER_BOUND ( 'NONE', #19516, .T. ) ;
#25562 = AXIS2_PLACEMENT_3D ( 'NONE', #8722, #30740, #16263 ) ;
#25563 = UNCERTAINTY_MEASURE_WITH_UNIT (LENGTH_MEASURE( 1.000000000000000082E-05 ), #30924, 'distance_accuracy_value', 'NONE');
#25564 = B_SPLINE_CURVE_WITH_KNOTS ( 'NONE', 3,
 ( #27680, #10128, #12920, #17824, #22415, #7665, #15208, #7334, #2892, #22910, #17659, #5041, #24897, #4707, #5197, #29660, #17505, #9960 ),
 .UNSPECIFIED., .F., .F.,
 ( 4, 2, 2, 2, 2, 2, 2, 2, 4 ),
 ( 0.0002279586355434578149, 0.0006426580022518073006, 0.001057357368960156786, 0.001472056735668506164, 0.001886756102376855758, 0.002301455469085205569, 0.002716154835793554295, 0.003130854202501903889, 0.003545553569210253483 ),
 .UNSPECIFIED. ) ;
#25565 = ORIENTED_EDGE ( 'NONE', *, *, #27579, .T. ) ;
#25566 = VECTOR ( 'NONE', #10106, 1000.000000000000114 ) ;
#25567 = EDGE_CURVE ( 'NONE', #12604, #28083, #20545, .T. ) ;
#25568 = AXIS2_PLACEMENT_3D ( 'NONE', #16482, #14362, #31596 ) ;
#25569 = EDGE_CURVE ( 'NONE', #4539, #11837, #28934, .T. ) ;
#25570 = EDGE_CURVE ( 'NONE', #26305, #28677, #28821, .T. ) ;
#25571 = ADVANCED_FACE ( 'NONE', ( #29964 ), #7144, .T. ) ;
#25572 = ORIENTED_EDGE ( 'NONE', *, *, #23204, .F. ) ;
#25573 = CARTESIAN_POINT ( 'NONE',  ( 80.77181806311267565, -5.983766253076982622, 14.98546771274985012 ) ) ;
#25574 = ORIENTED_EDGE ( 'NONE', *, *, #23611, .F. ) ;
#25575 = DIRECTION ( 'NONE',  ( -0.000000000000000000, 1.000000000000000000, -0.000000000000000000 ) ) ;
#25576 = FACE_OUTER_BOUND ( 'NONE', #3815, .T. ) ;
#25577 = CARTESIAN_POINT ( 'NONE',  ( 52.78302439342900954, -5.819500620027733717, 105.8370519042862981 ) ) ;
#25578 = CARTESIAN_POINT ( 'NONE',  ( 48.16694854572211426, 28.61789516297709568, 49.14507740233662503 ) ) ;
#25579 = ORIENTED_EDGE ( 'NONE', *, *, #31344, .F. ) ;
#25580 = VECTOR ( 'NONE', #24264, 1000.000000000000000 ) ;
#25581 = ORIENTED_EDGE ( 'NONE', *, *, #20403, .T. ) ;
#25582 = CARTESIAN_POINT ( 'NONE',  ( 8.732853799281732776, 25.72145308207319303, 47.04930799450051637 ) ) ;
#25583 = AXIS2_PLACEMENT_3D ( 'NONE', #24066, #9468, #21277 ) ;
#25584 = ORIENTED_EDGE ( 'NONE', *, *, #31345, .F. ) ;
#25585 = DIRECTION ( 'NONE',  ( 0.8746197071393926326, -0.4848096202463430537, -8.676864087101709653E-18 ) ) ;
#25586 = CARTESIAN_POINT ( 'NONE',  ( -40.05987053574653345, 7.506472619680471858, 35.39279590939684539 ) ) ;
#25587 = DIRECTION ( 'NONE',  ( 0.4544104193609900810, 5.611869858668441979E-17, 0.8907924397839090958 ) ) ;
#25588 = AXIS2_PLACEMENT_3D ( 'NONE', #15307, #7755, #10066 ) ;
#25589 = VECTOR ( 'NONE', #19813, 1000.000000000000000 ) ;
#25590 = DIRECTION ( 'NONE',  ( 0.8746197071393925215, -0.4848096202463429982, -8.676864087101708112E-18 ) ) ;
#25591 = DIRECTION ( 'NONE',  ( 1.000000000000000000, 0.000000000000000000, 0.000000000000000000 ) ) ;
#25592 = ORIENTED_EDGE ( 'NONE', *, *, #10034, .T. ) ;
#25593 = FACE_OUTER_BOUND ( 'NONE', #31472, .T. ) ;
#25594 = CARTESIAN_POINT ( 'NONE',  ( -40.65487266620045403, 9.475231293617264683, 38.63717596014456035 ) ) ;
#25595 = AXIS2_PLACEMENT_3D ( 'NONE', #13998, #9229, #16446 ) ;
#25596 = CARTESIAN_POINT ( 'NONE',  ( 21.09785597605720753, 15.57592086119046826, 47.04930799450052348 ) ) ;
#25597 = CYLINDRICAL_SURFACE ( 'NONE', #5671, 12.36707279061065101 ) ;
#25598 = ORIENTED_EDGE ( 'NONE', *, *, #1815, .F. ) ;
#25599 = DIRECTION ( 'NONE',  ( -1.000000000000000000, 0.000000000000000000, 0.000000000000000000 ) ) ;
#25600 = CARTESIAN_POINT ( 'NONE',  ( 21.09785597605719332, 28.56454579224779877, 46.64306900320794114 ) ) ;
#25601 = EDGE_CURVE ( 'NONE', #13599, #17931, #14797, .T. ) ;
#25602 = DIRECTION ( 'NONE',  ( 0.000000000000000000, 0.000000000000000000, 1.000000000000000000 ) ) ;
#25603 = ORIENTED_EDGE ( 'NONE', *, *, #27393, .T. ) ;
#25604 = CIRCLE ( 'NONE', #19832, 12.36707279061065101 ) ;
#25605 = AXIS2_PLACEMENT_3D ( 'NONE', #26079, #23626, #28882 ) ;
#25606 = ORIENTED_EDGE ( 'NONE', *, *, #11094, .F. ) ;
#25607 = AXIS2_PLACEMENT_3D ( 'NONE', #14788, #11672, #7230 ) ;
#25608 = ADVANCED_FACE ( 'NONE', ( #17138 ), #5887, .T. ) ;
#25609 = ADVANCED_FACE ( 'NONE', ( #1887 ), #4848, .T. ) ;
#25610 = EDGE_CURVE ( 'NONE', #23467, #22362, #29482, .T. ) ;
#25611 = AXIS2_PLACEMENT_3D ( 'NONE', #21588, #31618, #16345 ) ;
#25612 = ORIENTED_EDGE ( 'NONE', *, *, #12657, .T. ) ;
#25613 = ADVANCED_FACE ( 'NONE', ( #24871 ), #21901, .F. ) ;
#25614 = CARTESIAN_POINT ( 'NONE',  ( -42.38687957179149635, 4.148162238787999279, 35.74930799450051921 ) ) ;
#25615 = CARTESIAN_POINT ( 'NONE',  ( 21.09992658989238734, 30.72145308207317882, 47.04930799450051637 ) ) ;
#25616 = CARTESIAN_POINT ( 'NONE',  ( 21.09785597605719332, 13.74476430820393347, 47.04930799450051637 ) ) ;
#25617 = VECTOR ( 'NONE', #5095, 1000.000000000000000 ) ;
#25618 = EDGE_LOOP ( 'NONE', ( #13879, #21274, #1364, #6178 ) ) ;
#25619 = CYLINDRICAL_SURFACE ( 'NONE', #6203, 0.1000000000000014905 ) ;
#25620 = DIRECTION ( 'NONE',  ( -0.000000000000000000, -1.000000000000000000, -0.000000000000000000 ) ) ;
#25621 = CARTESIAN_POINT ( 'NONE',  ( 21.09785597605720397, -9.935454207752199451, -24.25069200549945947 ) ) ;
#25622 = CYLINDRICAL_SURFACE ( 'NONE', #14549, 12.36707279061065279 ) ;
#25623 = DIRECTION ( 'NONE',  ( -0.2756373558169973870, 0.9612616959383193382, -9.615507602343155278E-33 ) ) ;
#25624 = DIRECTION ( 'NONE',  ( 0.000000000000000000, 0.000000000000000000, -1.000000000000000000 ) ) ;
#25625 = DIRECTION ( 'NONE',  ( -1.000000000000000000, -1.101824276508909887E-16, 0.000000000000000000 ) ) ;
#25626 = DIRECTION ( 'NONE',  ( 0.000000000000000000, 0.000000000000000000, -1.000000000000000000 ) ) ;
#25627 = DIRECTION ( 'NONE',  ( 0.000000000000000000, 0.000000000000000000, 1.000000000000000000 ) ) ;
#25628 = CARTESIAN_POINT ( 'NONE',  ( 21.09785597605719687, -19.93545420775220123, 27.04930799450051637 ) ) ;
#25629 = CARTESIAN_POINT ( 'NONE',  ( 48.73570333863616355, 28.52287913140503761, 44.52463952959527660 ) ) ;
#25630 = VERTEX_POINT ( 'NONE', #12405 ) ;
#25631 = VERTEX_POINT ( 'NONE', #26841 ) ;
#25632 = DIRECTION ( 'NONE',  ( -0.1949050434465268433, 0.6797146636928677044, 0.7071067811865471286 ) ) ;
#25633 = CIRCLE ( 'NONE', #14628, 12.36707279061065101 ) ;
#25634 = CARTESIAN_POINT ( 'NONE',  ( 21.09992658989239089, 24.09164230456639544, 47.04930799450051637 ) ) ;
#25635 = AXIS2_PLACEMENT_3D ( 'NONE', #10920, #27834, #7979 ) ;
#25636 = DIRECTION ( 'NONE',  ( -1.101824276508909887E-16, 1.000000000000000000, -0.000000000000000000 ) ) ;
#25637 = EDGE_LOOP ( 'NONE', ( #24762, #16341, #23181 ) ) ;
#25638 = CARTESIAN_POINT ( 'NONE',  ( 21.09992658989238734, 32.34164230456639899, 47.04930799450051637 ) ) ;
#25639 = CARTESIAN_POINT ( 'NONE',  ( 49.19517401419062708, 28.28655426599985390, 48.40991706654173754 ) ) ;
#25640 = ORIENTED_EDGE ( 'NONE', *, *, #20377, .T. ) ;
#25641 = ORIENTED_EDGE ( 'NONE', *, *, #24054, .F. ) ;
#25642 = CARTESIAN_POINT ( 'NONE',  ( 21.09785597605719332, 14.86454579224779948, 47.04930799450051637 ) ) ;
#25643 = CARTESIAN_POINT ( 'NONE',  ( 45.24946171279598417, 28.50784706826092929, 47.99220971130007030 ) ) ;
#25644 = EDGE_CURVE ( 'NONE', #11408, #30811, #12168, .T. ) ;
#25645 = EDGE_CURVE ( 'NONE', #25156, #24129, #6392, .T. ) ;
#25646 = CARTESIAN_POINT ( 'NONE',  ( 45.24946171279598417, 27.72124452788248661, 47.99220971130007030 ) ) ;
#25647 = CIRCLE ( 'NONE', #31409, 0.1000000000000001305 ) ;
#25648 = LINE ( 'NONE', #5474, #12795 ) ;
#25649 = ORIENTED_EDGE ( 'NONE', *, *, #24852, .T. ) ;
#25650 = EDGE_CURVE ( 'NONE', #3723, #25296, #16880, .T. ) ;
#25651 = CARTESIAN_POINT ( 'NONE',  ( 47.09785597605719687, 15.77906836436399374, 47.04930799450078638 ) ) ;
#25652 = CARTESIAN_POINT ( 'NONE',  ( 8.482002859293434227, 27.71664230456639899, 47.04930799450051637 ) ) ;
#25653 = AXIS2_PLACEMENT_3D ( 'NONE', #20449, #30478, #18301 ) ;
#25654 = TOROIDAL_SURFACE ( 'NONE', #30910, 12.40141737965282154, 0.1250000000000006939 ) ;
#25655 = ORIENTED_EDGE ( 'NONE', *, *, #9403, .F. ) ;
#25656 = FACE_OUTER_BOUND ( 'NONE', #13624, .T. ) ;
#25657 = CYLINDRICAL_SURFACE ( 'NONE', #10080, 0.1000000000000004774 ) ;
#25658 = VECTOR ( 'NONE', #12206, 1000.000000000000114 ) ;
#25659 = ORIENTED_EDGE ( 'NONE', *, *, #29399, .T. ) ;
#25660 = AXIS2_PLACEMENT_3D ( 'NONE', #28629, #6141, #23222 ) ;
#25661 = LINE ( 'NONE', #8268, #12369 ) ;
#25662 = DIRECTION ( 'NONE',  ( -0.000000000000000000, -1.000000000000000000, 0.000000000000000000 ) ) ;
#25663 = DIRECTION ( 'NONE',  ( -1.000000000000000000, -0.000000000000000000, -0.000000000000000000 ) ) ;
#25664 = EDGE_CURVE ( 'NONE', #7765, #18056, #8505, .T. ) ;
#25665 = PLANE ( 'NONE',  #25225 ) ;
#25666 = DIRECTION ( 'NONE',  ( 0.9612616959383193382, 0.2756373558169973870, 8.795445018804928853E-19 ) ) ;
#25667 = ORIENTED_EDGE ( 'NONE', *, *, #15084, .T. ) ;
#25668 = CARTESIAN_POINT ( 'NONE',  ( 21.09992658989238734, 38.56284415653841791, 47.04930799450051637 ) ) ;
#25669 = CARTESIAN_POINT ( 'NONE',  ( 8.482002859293475083, 32.21664230456639899, 47.04930799450051637 ) ) ;
#25670 = FACE_OUTER_BOUND ( 'NONE', #2738, .T. ) ;
#25671 = EDGE_CURVE ( 'NONE', #1905, #2732, #11650, .T. ) ;
#25672 = CARTESIAN_POINT ( 'NONE',  ( -40.78929398160038744, 0.6853371204142075790, 42.04930799450051637 ) ) ;
#25673 = LINE ( 'NONE', #7968, #11060 ) ;
#25674 = ORIENTED_EDGE ( 'NONE', *, *, #370, .T. ) ;
#25675 = CARTESIAN_POINT ( 'NONE',  ( -40.70335362822509495, 9.387769322903325886, 39.54930799450052348 ) ) ;
#25676 = CARTESIAN_POINT ( 'NONE',  ( 49.69886365972154607, 24.87071433478734406, 46.18560630082799889 ) ) ;
#25677 = CYLINDRICAL_SURFACE ( 'NONE', #9620, 0.1000000000000018235 ) ;
#25678 = ORIENTED_EDGE ( 'NONE', *, *, #23311, .T. ) ;
#25679 = DIRECTION ( 'NONE',  ( -1.101824276508909887E-16, 1.000000000000000000, -0.000000000000000000 ) ) ;
#25680 = DIRECTION ( 'NONE',  ( -1.188208965918165239E-16, -1.880121038077813132E-16, -1.000000000000000000 ) ) ;
#25681 = ADVANCED_FACE ( 'NONE', ( #27157 ), #29473, .F. ) ;
#25682 = TOROIDAL_SURFACE ( 'NONE', #26185, 44.50000000000000000, 1.499999999999995115 ) ;
#25683 = AXIS2_PLACEMENT_3D ( 'NONE', #8429, #21044, #16121 ) ;
#25684 = EDGE_CURVE ( 'NONE', #14105, #27032, #9280, .T. ) ;
#25685 = DIRECTION ( 'NONE',  ( 0.000000000000000000, -0.000000000000000000, -1.000000000000000000 ) ) ;
#25686 = CARTESIAN_POINT ( 'NONE',  ( 21.09785597605720042, 15.56454579224779877, 101.5493079945004951 ) ) ;
#25687 = ADVANCED_FACE ( 'NONE', ( #4679 ), #629, .T. ) ;
#25688 = ORIENTED_EDGE ( 'NONE', *, *, #9426, .F. ) ;
#25689 = DIRECTION ( 'NONE',  ( -0.3428121700606640565, -0.6184495258776567805, -0.7071067811865474617 ) ) ;
#25690 = ORIENTED_EDGE ( 'NONE', *, *, #30035, .F. ) ;
#25691 = AXIS2_PLACEMENT_3D ( 'NONE', #7516, #32462, #1923 ) ;
#25692 = AXIS2_PLACEMENT_3D ( 'NONE', #23318, #829, #985 ) ;
#25693 = ORIENTED_EDGE ( 'NONE', *, *, #18960, .T. ) ;
#25694 = CIRCLE ( 'NONE', #9979, 12.62506659569710266 ) ;
#25695 = AXIS2_PLACEMENT_3D ( 'NONE', #4722, #7020, #9649 ) ;
#25696 = EDGE_CURVE ( 'NONE', #14804, #1265, #21590, .T. ) ;
#25697 = CIRCLE ( 'NONE', #11538, 1.200000000000006617 ) ;
#25698 = CARTESIAN_POINT ( 'NONE',  ( 47.20677300731728820, 19.86454579224779948, 44.95213440123257698 ) ) ;
#25699 = DIRECTION ( 'NONE',  ( -0.000000000000000000, -1.000000000000000000, 0.000000000000000000 ) ) ;
#25700 = CARTESIAN_POINT ( 'NONE',  ( 81.72575882806418690, -5.937449718911897101, 16.02633765848928249 ) ) ;
#25701 = TOROIDAL_SURFACE ( 'NONE', #23070, 35.50000000000000711, 1.500000000000001332 ) ;
#25702 = ORIENTED_EDGE ( 'NONE', *, *, #30706, .T. ) ;
#25703 = CARTESIAN_POINT ( 'NONE',  ( -34.36402903725590363, 11.90988715843502632, 40.33535946719864995 ) ) ;
#25704 = ORIENTED_EDGE ( 'NONE', *, *, #1336, .T. ) ;
#25705 = DIRECTION ( 'NONE',  ( -1.000000000000000000, 0.000000000000000000, 0.000000000000000000 ) ) ;
#25706 = CARTESIAN_POINT ( 'NONE',  ( -41.91739890389096956, 13.90674392281398930, 59.49868301348410426 ) ) ;
#25707 = DIRECTION ( 'NONE',  ( -1.101824276508909887E-16, 1.000000000000000000, -0.000000000000000000 ) ) ;
#25708 = ADVANCED_FACE ( 'NONE', ( #14701 ), #7461, .T. ) ;
#25709 = ORIENTED_EDGE ( 'NONE', *, *, #26065, .F. ) ;
#25710 = DIRECTION ( 'NONE',  ( -1.000000000000000000, 0.000000000000000000, 0.000000000000000000 ) ) ;
#25711 = ORIENTED_EDGE ( 'NONE', *, *, #25282, .T. ) ;
#25712 = CARTESIAN_POINT ( 'NONE',  ( 33.50134396954528171, 23.59164230456639544, 47.04930799450051637 ) ) ;
#25713 = DIRECTION ( 'NONE',  ( 1.313185983435984691E-29, -1.000000000000000000, -3.761114140369702165E-15 ) ) ;
#25714 = ORIENTED_EDGE ( 'NONE', *, *, #3569, .F. ) ;
#25715 = DIRECTION ( 'NONE',  ( 0.8746197071393925215, -0.4848096202463429982, -8.676864087101708112E-18 ) ) ;
#25716 = AXIS2_PLACEMENT_3D ( 'NONE', #2053, #24872, #12075 ) ;
#25717 = VECTOR ( 'NONE', #15202, 1000.000000000000000 ) ;
#25718 = EDGE_CURVE ( 'NONE', #10826, #24287, #25791, .T. ) ;
#25719 = DIRECTION ( 'NONE',  ( -1.101824276508909887E-16, 1.000000000000000000, -0.000000000000000000 ) ) ;
#25720 = CARTESIAN_POINT ( 'NONE',  ( 8.474859994195282908, 38.56284415653841791, 47.04930799450051637 ) ) ;
#25721 = CARTESIAN_POINT ( 'NONE',  ( 8.732853799281738105, 27.46183152705960850, 47.04930799450051637 ) ) ;
#25722 = DIRECTION ( 'NONE',  ( -1.000000000000000000, 0.000000000000000000, 0.000000000000000000 ) ) ;
#25723 = DIRECTION ( 'NONE',  ( 1.000000000000000000, 0.000000000000000000, -1.224646799147353207E-16 ) ) ;
#25724 = VERTEX_POINT ( 'NONE', #25194 ) ;
#25725 = CIRCLE ( 'NONE', #5271, 0.1250000000000001110 ) ;
#25726 = AXIS2_PLACEMENT_3D ( 'NONE', #13619, #18683, #8365 ) ;
#25727 = DIRECTION ( 'NONE',  ( 0.000000000000000000, 1.000000000000000000, -0.000000000000000000 ) ) ;
#25728 = ORIENTED_EDGE ( 'NONE', *, *, #28888, .T. ) ;
#25729 = AXIS2_PLACEMENT_3D ( 'NONE', #21261, #16978, #11588 ) ;
#25730 = EDGE_CURVE ( 'NONE', #7293, #15887, #31051, .T. ) ;
#25731 = LINE ( 'NONE', #21269, #19540 ) ;
#25732 = ORIENTED_EDGE ( 'NONE', *, *, #126, .T. ) ;
#25733 = ORIENTED_EDGE ( 'NONE', *, *, #26797, .F. ) ;
#25734 = CARTESIAN_POINT ( 'NONE',  ( -7.126919271800058908, 8.279996179725062078, 98.49479233384352028 ) ) ;
#25735 = AXIS2_PLACEMENT_3D ( 'NONE', #7345, #24743, #7679 ) ;
#25736 = EDGE_LOOP ( 'NONE', ( #4885, #20405, #12919, #8491 ) ) ;
#25737 = VECTOR ( 'NONE', #12937, 1000.000000000000114 ) ;
#25738 = VERTEX_POINT ( 'NONE', #13218 ) ;
#25739 = AXIS2_PLACEMENT_3D ( 'NONE', #17662, #28011, #8155 ) ;
#25740 = DIRECTION ( 'NONE',  ( 0.1949050434465251780, -0.6797146636928681485, -0.7071067811865470176 ) ) ;
#25741 = AXIS2_PLACEMENT_3D ( 'NONE', #4318, #8914, #3991 ) ;
#25742 = EDGE_LOOP ( 'NONE', ( #22822, #15141, #18895, #10431 ) ) ;
#25743 = CARTESIAN_POINT ( 'NONE',  ( 48.50919455764776700, 22.98879437201065912, 47.45523895251538704 ) ) ;
#25744 = CARTESIAN_POINT ( 'NONE',  ( 49.56570964645655408, 29.19876898723385139, 46.93360586032942194 ) ) ;
#25745 = FACE_OUTER_BOUND ( 'NONE', #15413, .T. ) ;
#25746 = CARTESIAN_POINT ( 'NONE',  ( 48.91284552371730143, 25.29289516297709994, 46.12344667017377020 ) ) ;
#25747 = ORIENTED_EDGE ( 'NONE', *, *, #1766, .F. ) ;
#25748 = ORIENTED_EDGE ( 'NONE', *, *, #8740, .F. ) ;
#25749 = DIRECTION ( 'NONE',  ( -1.101824276508909887E-16, 1.000000000000000000, -0.000000000000000000 ) ) ;
#25750 = AXIS2_PLACEMENT_3D ( 'NONE', #14325, #24163, #29423 ) ;
#25751 = ORIENTED_EDGE ( 'NONE', *, *, #9139, .F. ) ;
#25752 = CARTESIAN_POINT ( 'NONE',  ( 54.51561412322114109, -4.114116020023750764, 103.4405055751862079 ) ) ;
#25753 = LINE ( 'NONE', #20821, #18496 ) ;
#25754 = DIRECTION ( 'NONE',  ( -1.101824276508909887E-16, 1.000000000000000000, -0.000000000000000000 ) ) ;
#25755 = CYLINDRICAL_SURFACE ( 'NONE', #25340, 12.36707279061065101 ) ;
#25756 = ORIENTED_EDGE ( 'NONE', *, *, #3666, .F. ) ;
#25757 = CARTESIAN_POINT ( 'NONE',  ( -40.11286833322907341, 2.887657226147505973, 39.04930799450052348 ) ) ;
#25758 = EDGE_CURVE ( 'NONE', #27623, #13790, #6925, .T. ) ;
#25759 = CIRCLE ( 'NONE', #1128, 0.1250000000000001110 ) ;
#25760 = EDGE_CURVE ( 'NONE', #382, #26808, #26125, .T. ) ;
#25761 = DIRECTION ( 'NONE',  ( -1.224646799147353207E-16, 0.000000000000000000, -1.000000000000000000 ) ) ;
#25762 = FACE_OUTER_BOUND ( 'NONE', #15949, .T. ) ;
#25763 = AXIS2_PLACEMENT_3D ( 'NONE', #2711, #20103, #19770 ) ;
#25764 = VERTEX_POINT ( 'NONE', #30128 ) ;
#25765 = CARTESIAN_POINT ( 'NONE',  ( -41.91799733298573472, 13.87669230940966969, 59.51428496617474195 ) ) ;
#25766 = VERTEX_POINT ( 'NONE', #3014 ) ;
#25767 = CONICAL_SURFACE ( 'NONE', #30501, 30.00000000000000000, 1.378810109075523149 ) ;
#25768 = ORIENTED_EDGE ( 'NONE', *, *, #30031, .F. ) ;
#25769 = ORIENTED_EDGE ( 'NONE', *, *, #10097, .F. ) ;
#25770 = CARTESIAN_POINT ( 'NONE',  ( -40.23847960489091236, 6.935107575317838169, 39.54930799450052348 ) ) ;
#25771 = FACE_OUTER_BOUND ( 'NONE', #21565, .T. ) ;
#25772 = DIRECTION ( 'NONE',  ( -1.000000000000000000, 0.000000000000000000, 0.000000000000000000 ) ) ;
#25773 = VERTEX_POINT ( 'NONE', #13051 ) ;
#25774 = AXIS2_PLACEMENT_3D ( 'NONE', #22957, #7882, #2786 ) ;
#25775 = CIRCLE ( 'NONE', #11638, 0.09999999999999939493 ) ;
#25776 = CARTESIAN_POINT ( 'NONE',  ( 21.09785597605719332, 25.56454579224779877, 86.74871914086746472 ) ) ;
#25777 = AXIS2_PLACEMENT_3D ( 'NONE', #18276, #18441, #13057 ) ;
#25778 = DIRECTION ( 'NONE',  ( -0.2756373558169905591, 0.9612616959383213366, -2.072800435186483623E-19 ) ) ;
#25779 = DIRECTION ( 'NONE',  ( -1.000000000000000000, 0.000000000000000000, 0.000000000000000000 ) ) ;
#25780 = LINE ( 'NONE', #21321, #28692 ) ;
#25781 = DIRECTION ( 'NONE',  ( 0.000000000000000000, -0.000000000000000000, -1.000000000000000000 ) ) ;
#25782 = CARTESIAN_POINT ( 'NONE',  ( 8.474859994195281132, 30.84184655352422411, 47.04930799450051637 ) ) ;
#25783 = CARTESIAN_POINT ( 'NONE',  ( 21.09992658989239089, 29.34164230456639899, 47.04930799450051637 ) ) ;
#25784 = DIRECTION ( 'NONE',  ( -1.000000000000000000, -1.101824276508909764E-16, 0.000000000000000000 ) ) ;
#25785 = FACE_OUTER_BOUND ( 'NONE', #1345, .T. ) ;
#25786 = LINE ( 'NONE', #15301, #47 ) ;
#25787 = SURFACE_STYLE_FILL_AREA ( #23802 ) ;
#25788 = EDGE_LOOP ( 'NONE', ( #5888, #18918, #18605, #10347 ) ) ;
#25789 = EDGE_LOOP ( 'NONE', ( #10787, #9015, #659, #2217 ) ) ;
#25790 = CARTESIAN_POINT ( 'NONE',  ( 69.53401346131808225, -13.30632128221581567, 75.01995691340934513 ) ) ;
#25791 = CIRCLE ( 'NONE', #29999, 2.000000000000001776 ) ;
#25792 = FACE_OUTER_BOUND ( 'NONE', #25994, .T. ) ;
#25793 = EDGE_CURVE ( 'NONE', #18578, #4682, #15118, .T. ) ;
#25794 = DIRECTION ( 'NONE',  ( -1.101824276508909887E-16, 1.000000000000000000, -0.000000000000000000 ) ) ;
#25795 = AXIS2_PLACEMENT_3D ( 'NONE', #29827, #20126, #17661 ) ;
#25796 = ADVANCED_FACE ( 'NONE', ( #27651 ), #32414, .T. ) ;
#25797 = ORIENTED_EDGE ( 'NONE', *, *, #21617, .F. ) ;
#25798 = CARTESIAN_POINT ( 'NONE',  ( -40.02540636251514172, 2.839176264122877047, 58.24930799450051921 ) ) ;
#25799 = CARTESIAN_POINT ( 'NONE',  ( 45.82550680184641578, 24.86454579224779593, 44.55508916310584056 ) ) ;
#25800 = ADVANCED_FACE ( 'NONE', ( #5650 ), #10593, .F. ) ;
#25801 = VERTEX_POINT ( 'NONE', #8122 ) ;
#25802 = CARTESIAN_POINT ( 'NONE',  ( 33.72499318558949710, 25.84143805560860940, 47.04930799450051637 ) ) ;
#25803 = EDGE_CURVE ( 'NONE', #18077, #19861, #18747, .T. ) ;
#25804 = CARTESIAN_POINT ( 'NONE',  ( 44.77625694075214824, 29.51454579807170120, 48.23360063142255427 ) ) ;
#25805 = CARTESIAN_POINT ( 'NONE',  ( 45.24946171279598417, 29.82124452788248092, 47.99220971130007030 ) ) ;
#25806 = CIRCLE ( 'NONE', #13240, 12.62506659569710266 ) ;
#25807 = CARTESIAN_POINT ( 'NONE',  ( -39.40232922475848909, -5.936135130407838467, 77.93127265747673960 ) ) ;
#25808 = CIRCLE ( 'NONE', #15848, 0.2000000000000012601 ) ;
#25809 = EDGE_LOOP ( 'NONE', ( #2934, #15424, #23545, #21876 ) ) ;
#25810 = DIRECTION ( 'NONE',  ( -1.101824276508909887E-16, 1.000000000000000000, -0.000000000000000000 ) ) ;
#25811 = CARTESIAN_POINT ( 'NONE',  ( 21.09785597605719332, 34.11266481626051217, 59.53344952167763182 ) ) ;
#25812 = ORIENTED_EDGE ( 'NONE', *, *, #776, .F. ) ;
#25813 = VECTOR ( 'NONE', #21820, 1000.000000000000000 ) ;
#25814 = DIRECTION ( 'NONE',  ( -0.000000000000000000, 1.000000000000000000, -0.000000000000000000 ) ) ;
#25816 = CARTESIAN_POINT ( 'NONE',  ( 46.33206787849857022, 22.99884124225578574, 48.22973596570440691 ) ) ;
#25815 = AXIS2_PLACEMENT_3D ( 'NONE', #12146, #12304, #17698 ) ;
#25817 = EDGE_CURVE ( 'NONE', #12300, #23862, #28221, .T. ) ;
#25818 = DIRECTION ( 'NONE',  ( -1.224646799147353207E-16, -1.349345573449484691E-32, 1.000000000000000000 ) ) ;
#25819 = EDGE_CURVE ( 'NONE', #31321, #24672, #11431, .T. ) ;
#25820 = VECTOR ( 'NONE', #20456, 1000.000000000000000 ) ;
#25821 = ORIENTED_EDGE ( 'NONE', *, *, #18043, .F. ) ;
#25822 = CARTESIAN_POINT ( 'NONE',  ( 21.09785597605719332, -9.935454207752199451, 47.04930799450051637 ) ) ;
#25823 = SPHERICAL_SURFACE ( 'NONE', #11534, 0.1000000000000000056 ) ;
#25824 = CARTESIAN_POINT ( 'NONE',  ( 5.864109918520784781, 14.46497581658974063, 47.04930799450052348 ) ) ;
#25825 = VECTOR ( 'NONE', #8652, 1000.000000000000000 ) ;
#25826 = CARTESIAN_POINT ( 'NONE',  ( -39.31817303416427478, 4.733858564475564634, 57.04930799450051637 ) ) ;
#25827 = VERTEX_POINT ( 'NONE', #20584 ) ;
#25828 = CARTESIAN_POINT ( 'NONE',  ( 46.81682104422132085, 23.12036939723557083, 47.03471240234085116 ) ) ;
#25829 = DIRECTION ( 'NONE',  ( 0.8746197071393926326, -0.4848096202463430537, -8.676864087101709653E-18 ) ) ;
#25830 = DIRECTION ( 'NONE',  ( -0.000000000000000000, 1.000000000000000000, -0.000000000000000000 ) ) ;
#25831 = FACE_OUTER_BOUND ( 'NONE', #26932, .T. ) ;
#25832 = CARTESIAN_POINT ( 'NONE',  ( -40.46704588662232993, 7.410332433786888551, 38.79878528233096091 ) ) ;
#25833 = EDGE_LOOP ( 'NONE', ( #6511, #7471, #11760, #31404 ) ) ;
#25834 = DIRECTION ( 'NONE',  ( 0.1949050434465282311, -0.6797146636928674823, -0.7071067811865470176 ) ) ;
#25835 = DIRECTION ( 'NONE',  ( -1.000000000000000000, -1.101824276508909887E-16, 0.000000000000000000 ) ) ;
#25836 = ORIENTED_EDGE ( 'NONE', *, *, #15628, .F. ) ;
#25837 = CARTESIAN_POINT ( 'NONE',  ( -9.880269303432738681, -5.935454207752202116, -12.56967651669337727 ) ) ;
#25838 = ADVANCED_FACE ( 'NONE', ( #25670 ), #21918, .T. ) ;
#25839 = CARTESIAN_POINT ( 'NONE',  ( -40.06561427811386267, 7.496110634155836117, 56.04611646155296256 ) ) ;
#25840 = CARTESIAN_POINT ( 'NONE',  ( 8.698509210239503631, 23.84164230456639544, 47.04930799450051637 ) ) ;
#25841 = CARTESIAN_POINT ( 'NONE',  ( 54.50543043370684870, -4.161241697801258077, -9.378833830732101973 ) ) ;
#25842 = CIRCLE ( 'NONE', #15355, 0.9999999999999991118 ) ;
#25843 = EDGE_LOOP ( 'NONE', ( #25990, #24499, #1740, #16274 ) ) ;
#25844 = CARTESIAN_POINT ( 'NONE',  ( -40.61574147496727960, 7.605736927813758541, 60.17502049423573851 ) ) ;
#25845 = ORIENTED_EDGE ( 'NONE', *, *, #19481, .F. ) ;
#25846 = EDGE_LOOP ( 'NONE', ( #2596, #25649, #10303, #29462 ) ) ;
#25847 = AXIS2_PLACEMENT_3D ( 'NONE', #16792, #11720, #21381 ) ;
#25848 =( BOUNDED_CURVE ( )  B_SPLINE_CURVE ( 3, ( #19014, #14279, #18852, #6716 ),
 .UNSPECIFIED., .F., .F. ) 
 B_SPLINE_CURVE_WITH_KNOTS ( ( 4, 4 ),
 ( 5.062864179022700029, 5.184122060454620318 ),
 .UNSPECIFIED. ) 
 CURVE ( )  GEOMETRIC_REPRESENTATION_ITEM ( )  RATIONAL_B_SPLINE_CURVE ( ( 1.000000000000000000, 0.9987750858034806223, 0.9987750858034806223, 1.000000000000000000 ) ) 
 REPRESENTATION_ITEM ( '' )  );
#25849 = AXIS2_PLACEMENT_3D ( 'NONE', #3267, #5737, #26399 ) ;
#25850 = EDGE_CURVE ( 'NONE', #19852, #4736, #7246, .T. ) ;
#25851 = ADVANCED_FACE ( 'NONE', ( #5340 ), #20743, .F. ) ;
#25852 = FACE_OUTER_BOUND ( 'NONE', #11958, .T. ) ;
#25853 = DIRECTION ( 'NONE',  ( -1.101824276508909887E-16, 1.000000000000000000, -0.000000000000000000 ) ) ;
#25854 = CARTESIAN_POINT ( 'NONE',  ( 48.66895200406656841, 27.06155426599985958, 44.62753372671560470 ) ) ;
#25855 = EDGE_CURVE ( 'NONE', #23266, #21162, #18795, .T. ) ;
#25856 = ADVANCED_FACE ( 'NONE', ( #3987 ), #31571, .F. ) ;
#25857 = ORIENTED_EDGE ( 'NONE', *, *, #10166, .T. ) ;
#25858 = DIRECTION ( 'NONE',  ( -1.188208965918165239E-16, -1.880121038077813132E-16, -1.000000000000000000 ) ) ;
#25859 = ORIENTED_EDGE ( 'NONE', *, *, #1801, .T. ) ;
#25860 = CIRCLE ( 'NONE', #8576, 31.50000000000000000 ) ;
#25861 = CARTESIAN_POINT ( 'NONE',  ( 8.474859994195282908, 38.56284415653841791, 47.04930799450051637 ) ) ;
#25862 = DIRECTION ( 'NONE',  ( 0.4544104193609903586, 0.000000000000000000, 0.8907924397839087627 ) ) ;
#25863 = FACE_OUTER_BOUND ( 'NONE', #5567, .T. ) ;
#25864 = CYLINDRICAL_SURFACE ( 'NONE', #18368, 12.36707279061065279 ) ;
#25866 = ORIENTED_EDGE ( 'NONE', *, *, #17634, .F. ) ;
#25865 =( REPRESENTATION_RELATIONSHIP ('NONE','NONE', #20382, #3604 ) REPRESENTATION_RELATIONSHIP_WITH_TRANSFORMATION ( #2941 )SHAPE_REPRESENTATION_RELATIONSHIP( ) );
#25867 = DIRECTION ( 'NONE',  ( -1.000000000000000000, 0.000000000000000000, 0.000000000000000000 ) ) ;
#25868 = ORIENTED_EDGE ( 'NONE', *, *, #5668, .F. ) ;
#25869 = CARTESIAN_POINT ( 'NONE',  ( 21.09785597605719332, 25.56454579224779167, 21.04930799450051282 ) ) ;
#25870 = DIRECTION ( 'NONE',  ( 0.000000000000000000, -0.000000000000000000, -1.000000000000000000 ) ) ;
#25871 = ORIENTED_EDGE ( 'NONE', *, *, #5668, .T. ) ;
#25872 = CARTESIAN_POINT ( 'NONE',  ( 48.23388202445966755, 26.95087065737812182, 49.27628909396054979 ) ) ;
#25873 = LINE ( 'NONE', #20461, #12098 ) ;
#25874 = DIRECTION ( 'NONE',  ( -1.101824276508909887E-16, 1.000000000000000000, -0.000000000000000000 ) ) ;
#25875 = DIRECTION ( 'NONE',  ( 0.8746197071393926326, -0.4848096202463430537, -8.676864087101709653E-18 ) ) ;
#25876 = AXIS2_PLACEMENT_3D ( 'NONE', #12035, #16944, #3995 ) ;
#25877 = CARTESIAN_POINT ( 'NONE',  ( 45.79384627280941089, 25.67957786121582231, 49.05938063676249072 ) ) ;
#25878 = VECTOR ( 'NONE', #27302, 1000.000000000000114 ) ;
#25879 = ORIENTED_EDGE ( 'NONE', *, *, #15239, .T. ) ;
#25880 = CIRCLE ( 'NONE', #713, 12.62506659569710443 ) ;
#25881 = CARTESIAN_POINT ( 'NONE',  ( 49.40414881150629611, 22.80400562401889530, 47.16908566558144855 ) ) ;
#25882 = DIRECTION ( 'NONE',  ( 0.9612616959383193382, 0.2756373558169973870, 8.795445018804928853E-19 ) ) ;
#25883 = B_SPLINE_CURVE_WITH_KNOTS ( 'NONE', 3,
 ( #7683, #9650, #7182, #19807, #27196, #24746 ),
 .UNSPECIFIED., .F., .F.,
 ( 4, 2, 4 ),
 ( 0.000000000000000000, 0.5000000000000000000, 1.000000000000000000 ),
 .UNSPECIFIED. ) ;
#25884 = ORIENTED_EDGE ( 'NONE', *, *, #4340, .F. ) ;
#25885 = EDGE_CURVE ( 'NONE', #31909, #32279, #10925, .T. ) ;
#25886 = CARTESIAN_POINT ( 'NONE',  ( 21.09785597605720753, 14.98269195386757602, 47.04930799450052348 ) ) ;
#25887 = FACE_OUTER_BOUND ( 'NONE', #24545, .T. ) ;
#25888 = ORIENTED_EDGE ( 'NONE', *, *, #23351, .F. ) ;
#25889 = VERTEX_POINT ( 'NONE', #3345 ) ;
#25890 = CARTESIAN_POINT ( 'NONE',  ( -11.78368228729793543, -4.961365878511771577, 104.2979330918141585 ) ) ;
#25891 = UNCERTAINTY_MEASURE_WITH_UNIT (LENGTH_MEASURE( 1.000000000000000082E-05 ), #18266, 'distance_accuracy_value', 'NONE');
#25892 = ORIENTED_EDGE ( 'NONE', *, *, #24278, .F. ) ;
#25893 = ADVANCED_FACE ( 'NONE', ( #31089 ), #25986, .T. ) ;
#25894 = AXIS2_PLACEMENT_3D ( 'NONE', #19279, #26681, #4200 ) ;
#25895 = VERTEX_POINT ( 'NONE', #8598 ) ;
#25896 = CARTESIAN_POINT ( 'NONE',  ( 21.09785597605719332, -16.72540370141334520, 47.04930799450051637 ) ) ;
#25897 = EDGE_CURVE ( 'NONE', #13560, #12063, #12507, .T. ) ;
#25898 = ORIENTED_EDGE ( 'NONE', *, *, #11930, .F. ) ;
#25899 = EDGE_CURVE ( 'NONE', #9845, #31626, #25081, .T. ) ;
#25900 = FACE_OUTER_BOUND ( 'NONE', #1622, .T. ) ;
#25901 = FACE_OUTER_BOUND ( 'NONE', #30161, .T. ) ;
#25902 = CARTESIAN_POINT ( 'NONE',  ( 21.09992658989238734, 38.56284415653841791, 47.04930799450051637 ) ) ;
#25903 = CARTESIAN_POINT ( 'NONE',  ( 46.02876340639226527, 26.16789516297709639, 44.95353858666495483 ) ) ;
#25904 = ORIENTED_EDGE ( 'NONE', *, *, #16402, .T. ) ;
#25905 = ORIENTED_EDGE ( 'NONE', *, *, #3569, .T. ) ;
#25906 = VERTEX_POINT ( 'NONE', #18911 ) ;
#25907 = CARTESIAN_POINT ( 'NONE',  ( 44.25300042956540381, 11.55930814891847902, 98.98522354484056507 ) ) ;
#25908 = CARTESIAN_POINT ( 'NONE',  ( 50.84143616388391251, 6.334306897662570712, 98.87890954738082883 ) ) ;
#25909 = AXIS2_PLACEMENT_3D ( 'NONE', #12681, #30230, #2329 ) ;
#25910 = CARTESIAN_POINT ( 'NONE',  ( 21.09785597605720753, 14.86454579224779948, 47.04930799450052348 ) ) ;
#25911 = CARTESIAN_POINT ( 'NONE',  ( -40.11286833322908052, 2.887657226147511302, 55.14930799450051779 ) ) ;
#25912 = AXIS2_PLACEMENT_3D ( 'NONE', #23076, #30312, #8307 ) ;
#25913 = ORIENTED_EDGE ( 'NONE', *, *, #19620, .F. ) ;
#25914 = CARTESIAN_POINT ( 'NONE',  ( 8.732853799281732776, 38.56284415653841791, 47.04930799450051637 ) ) ;
#25915 = AXIS2_PLACEMENT_3D ( 'NONE', #10053, #14813, #29583 ) ;
#25916 = DIRECTION ( 'NONE',  ( 0.8746197071393926326, -0.4848096202463430537, -8.676864087101709653E-18 ) ) ;
#25917 = CYLINDRICAL_SURFACE ( 'NONE', #5221, 12.62506659569710266 ) ;
#25918 = CARTESIAN_POINT ( 'NONE',  ( 46.99023568444674481, 25.82451373492760283, 49.12151524109405898 ) ) ;
#25919 = ORIENTED_EDGE ( 'NONE', *, *, #371, .F. ) ;
#25920 = LINE ( 'NONE', #3275, #29343 ) ;
#25921 = CARTESIAN_POINT ( 'NONE',  ( -40.50746472795130870, 7.570599710249083181, 53.85997431717469652 ) ) ;
#25922 = ORIENTED_EDGE ( 'NONE', *, *, #8258, .T. ) ;
#25923 = ADVANCED_FACE ( 'NONE', ( #11541 ), #7789, .T. ) ;
#25924 = ORIENTED_EDGE ( 'NONE', *, *, #7275, .T. ) ;
#25925 = AXIS2_PLACEMENT_3D ( 'NONE', #1799, #14286, #21317 ) ;
#25926 = EDGE_LOOP ( 'NONE', ( #20904, #31607, #8626, #10265, #17689 ) ) ;
#25927 = TOROIDAL_SURFACE ( 'NONE', #26988, 83.95485889133257729, 94.44530576803552435 ) ;
#25928 = CARTESIAN_POINT ( 'NONE',  ( -36.21250238186772208, 8.895094119121829124, 60.29072935073781991 ) ) ;
#25929 = CARTESIAN_POINT ( 'NONE',  ( -44.94873447355087137, -5.453371160069278467, 52.74359862448790892 ) ) ;
#25930 = VECTOR ( 'NONE', #20694, 1000.000000000000114 ) ;
#25931 = VECTOR ( 'NONE', #20622, 1000.000000000000000 ) ;
#25932 = EDGE_CURVE ( 'NONE', #1400, #11991, #13527, .T. ) ;
#25933 = AXIS2_PLACEMENT_3D ( 'NONE', #31992, #26741, #29367 ) ;
#25934 = VERTEX_POINT ( 'NONE', #23371 ) ;
#25935 = CARTESIAN_POINT ( 'NONE',  ( 21.09992658989239089, 23.84164230456639544, 47.04930799450051637 ) ) ;
#25936 = DIRECTION ( 'NONE',  ( 0.9612616959383221138, 0.2756373558169876170, 0.000000000000000000 ) ) ;
#25937 = DIRECTION ( 'NONE',  ( -1.000000000000000000, 0.000000000000000000, 0.000000000000000000 ) ) ;
#25938 = VERTEX_POINT ( 'NONE', #878 ) ;
#25939 = DIRECTION ( 'NONE',  ( -1.000000000000000000, 0.000000000000000000, -1.224646799147353207E-16 ) ) ;
#25940 = ORIENTED_EDGE ( 'NONE', *, *, #26011, .F. ) ;
#25941 = CARTESIAN_POINT ( 'NONE',  ( 45.36511207810799107, 27.33213139976340500, 45.12672418911605376 ) ) ;
#25942 = CARTESIAN_POINT ( 'NONE',  ( 21.09785597605719332, 14.58544108513610027, 47.04930799450051637 ) ) ;
#25943 = DIRECTION ( 'NONE',  ( -1.101824276508909887E-16, 1.000000000000000000, -0.000000000000000000 ) ) ;
#25944 = DIRECTION ( 'NONE',  ( -1.101824276508909887E-16, 1.000000000000000000, -0.000000000000000000 ) ) ;
#25945 = VERTEX_POINT ( 'NONE', #31249 ) ;
#25946 = ORIENTED_EDGE ( 'NONE', *, *, #18874, .T. ) ;
#25947 = CYLINDRICAL_SURFACE ( 'NONE', #16550, 0.1000000000000028644 ) ;
#25948 = DIRECTION ( 'NONE',  ( 0.000000000000000000, 0.000000000000000000, -1.000000000000000000 ) ) ;
#25949 = DIRECTION ( 'NONE',  ( -1.000000000000000000, 0.000000000000000000, 0.000000000000000000 ) ) ;
#25950 = VECTOR ( 'NONE', #27227, 1000.000000000000000 ) ;
#25951 = ORIENTED_EDGE ( 'NONE', *, *, #16881, .F. ) ;
#25952 = DIRECTION ( 'NONE',  ( 0.8746197071393926326, -0.4848096202463430537, -8.676864087101709653E-18 ) ) ;
#25953 = CARTESIAN_POINT ( 'NONE',  ( 47.22751897799751220, 28.51988759933318818, 44.55267275764142454 ) ) ;
#25954 = PRODUCT_DEFINITION ( 'UNKNOWN', '', #18150, #9789 ) ;
#25955 = ORIENTED_EDGE ( 'NONE', *, *, #20116, .F. ) ;
#25957 = AXIS2_PLACEMENT_3D ( 'NONE', #6576, #16568, #6730 ) ;
#25956 = CARTESIAN_POINT ( 'NONE',  ( 8.732853799281738105, 30.47145308207317882, 47.04930799450051637 ) ) ;
#25958 = CARTESIAN_POINT ( 'NONE',  ( 48.73570333863616355, 27.82287913140503832, 44.52463952959527660 ) ) ;
#25959 = AXIS2_PLACEMENT_3D ( 'NONE', #13561, #18306, #3217 ) ;
#25960 = AXIS2_PLACEMENT_3D ( 'NONE', #15864, #10631, #5864 ) ;
#25961 = CARTESIAN_POINT ( 'NONE',  ( -39.41385926433662235, -5.936084327709292729, 77.91473385016919906 ) ) ;
#25962 = AXIS2_PLACEMENT_3D ( 'NONE', #11575, #23877, #11402 ) ;
#25963 = B_SPLINE_CURVE_WITH_KNOTS ( 'NONE', 3,
 ( #9799, #2566, #14888, #2733, #30155, #7504, #27356, #7825, #4874, #25378 ),
 .UNSPECIFIED., .F., .F.,
 ( 4, 2, 2, 2, 4 ),
 ( 0.0006716755660530369584, 0.002413276598758841776, 0.004154877631464646594, 0.005896478664170451411, 0.007638079696876256229 ),
 .UNSPECIFIED. ) ;
#25964 = VERTEX_POINT ( 'NONE', #13692 ) ;
#25965 = PLANE ( 'NONE',  #26974 ) ;
#25966 = CARTESIAN_POINT ( 'NONE',  ( 21.09785597605719332, 15.63322284159649556, 47.04930799450051637 ) ) ;
#25967 = EDGE_CURVE ( 'NONE', #22254, #32203, #30302, .T. ) ;
#25968 = EDGE_LOOP ( 'NONE', ( #13430, #14916, #5391, #28807 ) ) ;
#25969 = ADVANCED_FACE ( 'NONE', ( #20900 ), #17730, .T. ) ;
#25970 = ADVANCED_FACE ( 'NONE', ( #18432 ), #23845, .T. ) ;
#25971 = ADVANCED_FACE ( 'NONE', ( #3827 ), #1465, .T. ) ;
#25972 = EDGE_CURVE ( 'NONE', #30053, #18805, #4688, .T. ) ;
#25973 = DIRECTION ( 'NONE',  ( -2.779292025043186357E-18, 1.288349127009862211E-17, -1.000000000000000000 ) ) ;
#25974 = DIRECTION ( 'NONE',  ( 0.000000000000000000, 0.000000000000000000, -1.000000000000000000 ) ) ;
#25975 = CIRCLE ( 'NONE', #17596, 12.62506659569710266 ) ;
#25976 = CARTESIAN_POINT ( 'NONE',  ( 21.09785597605719332, 25.56454579224779877, 47.04930799450051637 ) ) ;
#25977 = TOROIDAL_SURFACE ( 'NONE', #21234, 58.86319174311611846, 0.1999999999999984290 ) ;
#25978 = ORIENTED_EDGE ( 'NONE', *, *, #2349, .T. ) ;
#25979 = DIRECTION ( 'NONE',  ( -0.9275012328650846793, -0.3738200944756017163, 0.000000000000000000 ) ) ;
#25980 = DIRECTION ( 'NONE',  ( -0.000000000000000000, -1.000000000000000000, 0.000000000000000000 ) ) ;
#25981 = DIRECTION ( 'NONE',  ( 0.000000000000000000, 0.000000000000000000, -1.000000000000000000 ) ) ;
#25982 = CYLINDRICAL_SURFACE ( 'NONE', #10570, 12.36707279061065101 ) ;
#25983 = ORIENTED_EDGE ( 'NONE', *, *, #28399, .T. ) ;
#25984 = DIRECTION ( 'NONE',  ( -1.000000000000000000, 0.000000000000000000, 0.000000000000000000 ) ) ;
#25985 = CARTESIAN_POINT ( 'NONE',  ( 47.20547626766765603, 29.58791119454915020, 44.97710074790751378 ) ) ;
#25986 = PLANE ( 'NONE',  #22440 ) ;
#25987 = DIRECTION ( 'NONE',  ( -1.101824276508909887E-16, 1.000000000000000000, -0.000000000000000000 ) ) ;
#25988 = CIRCLE ( 'NONE', #11312, 11.79999999999997762 ) ;
#25989 = CARTESIAN_POINT ( 'NONE',  ( 79.15081694298606863, -5.581242224120285478, 79.20493092526746182 ) ) ;
#25990 = ORIENTED_EDGE ( 'NONE', *, *, #21145, .T. ) ;
#25991 = CARTESIAN_POINT ( 'NONE',  ( 47.24492228087488144, 29.61131241985434670, 45.00104688274142006 ) ) ;
#25992 = CARTESIAN_POINT ( 'NONE',  ( -21.90214402394278892, 14.86454579224779948, 47.04930799450052348 ) ) ;
#25993 = DIRECTION ( 'NONE',  ( 0.000000000000000000, -0.000000000000000000, -1.000000000000000000 ) ) ;
#25994 = EDGE_LOOP ( 'NONE', ( #27818, #9902, #8158, #11128 ) ) ;
#25995 = DIRECTION ( 'NONE',  ( 0.2756373558169932236, -0.9612616959383206705, 1.479773560108267395E-16 ) ) ;
#25996 = CARTESIAN_POINT ( 'NONE',  ( 48.23388202445966755, 15.77906836436399374, 49.27628909396055690 ) ) ;
#25997 = DIRECTION ( 'NONE',  ( -0.000000000000000000, -1.000000000000000000, 0.000000000000000000 ) ) ;
#25998 = FACE_OUTER_BOUND ( 'NONE', #27354, .T. ) ;
#25999 = EDGE_LOOP ( 'NONE', ( #6869, #3974, #6976, #1723 ) ) ;
#26000 = DIRECTION ( 'NONE',  ( 0.000000000000000000, -0.7071067811865378028, -0.7071067811865573427 ) ) ;
#26001 = ORIENTED_EDGE ( 'NONE', *, *, #28401, .F. ) ;
#26002 = EDGE_CURVE ( 'NONE', #25278, #17298, #32057, .T. ) ;
#26003 = AXIS2_PLACEMENT_3D ( 'NONE', #5614, #18549, #3135 ) ;
#26004 = MECHANICAL_DESIGN_GEOMETRIC_PRESENTATION_REPRESENTATION (  '', ( #19174 ), #18655 ) ;
#26005 = ORIENTED_EDGE ( 'NONE', *, *, #10803, .F. ) ;
#26006 = AXIS2_PLACEMENT_3D ( 'NONE', #22540, #10090, #20086 ) ;
#26007 = ADVANCED_FACE ( 'NONE', ( #19569 ), #22354, .T. ) ;
#26008 = ADVANCED_FACE ( 'NONE', ( #14334 ), #9402, .T. ) ;
#26009 = DIRECTION ( 'NONE',  ( -1.000000000000000000, 0.000000000000000000, 0.000000000000000000 ) ) ;
#26010 = CARTESIAN_POINT ( 'NONE',  ( -40.59581018552366061, 9.375516295340281303, 34.64930799450051779 ) ) ;
#26011 = EDGE_CURVE ( 'NONE', #16189, #32468, #9893, .T. ) ;
#26012 = ORIENTED_EDGE ( 'NONE', *, *, #12985, .F. ) ;
#26013 = FACE_OUTER_BOUND ( 'NONE', #8495, .T. ) ;
#26014 = EDGE_LOOP ( 'NONE', ( #6734, #19037, #27078, #20599 ) ) ;
#26015 = CARTESIAN_POINT ( 'NONE',  ( 21.09992658989239089, 24.09184655352419213, 47.04930799450051637 ) ) ;
#26016 = CARTESIAN_POINT ( 'NONE',  ( 21.09785597605719332, 14.56957104541719694, 47.04930799450051637 ) ) ;
#26017 = CARTESIAN_POINT ( 'NONE',  ( 21.09785597605720753, 13.61454579224779771, 47.04930799450052348 ) ) ;
#26018 = LINE ( 'NONE', #13558, #18900 ) ;
#26019 = ORIENTED_EDGE ( 'NONE', *, *, #23480, .T. ) ;
#26020 = CARTESIAN_POINT ( 'NONE',  ( 21.09992658989239089, 27.96183152705961206, 47.04930799450051637 ) ) ;
#26021 = ORIENTED_EDGE ( 'NONE', *, *, #25567, .F. ) ;
#26022 = DIRECTION ( 'NONE',  ( 0.4114095458597712973, 0.6546536707079773088, -0.6341693441061526659 ) ) ;
#26024 = LINE ( 'NONE', #13564, #15287 ) ;
#26023 = TOROIDAL_SURFACE ( 'NONE', #8731, 12.40141737965287305, 0.1250000000000000833 ) ;
#26025 = ORIENTED_EDGE ( 'NONE', *, *, #2953, .F. ) ;
#26026 = DIRECTION ( 'NONE',  ( 0.000000000000000000, 0.000000000000000000, 1.000000000000000000 ) ) ;
#26027 = CARTESIAN_POINT ( 'NONE',  ( -40.12608762486730996, 7.344210729236881008, 60.41996114768177506 ) ) ;
#26028 = FACE_OUTER_BOUND ( 'NONE', #12046, .T. ) ;
#26029 = FACE_OUTER_BOUND ( 'NONE', #25162, .T. ) ;
#26030 = SURFACE_SIDE_STYLE ('',( #16024 ) ) ;
#26031 = ORIENTED_EDGE ( 'NONE', *, *, #6636, .F. ) ;
#26032 = DIRECTION ( 'NONE',  ( 0.000000000000000000, 0.000000000000000000, -1.000000000000000000 ) ) ;
#26033 = DIRECTION ( 'NONE',  ( -1.000000000000000000, -1.101824276508909887E-16, 0.000000000000000000 ) ) ;
#26034 = ORIENTED_EDGE ( 'NONE', *, *, #11767, .T. ) ;
#26035 = CARTESIAN_POINT ( 'NONE',  ( -40.68422973805265030, 6.807290781432338456, 34.77612644482307758 ) ) ;
#26036 = EDGE_CURVE ( 'NONE', #23355, #28042, #9350, .T. ) ;
#26037 = TOROIDAL_SURFACE ( 'NONE', #17123, 12.61792373059894068, 0.1249999999999991118 ) ;
#26038 = FACE_OUTER_BOUND ( 'NONE', #9741, .T. ) ;
#26039 = ORIENTED_EDGE ( 'NONE', *, *, #9337, .T. ) ;
#26040 =( BOUNDED_CURVE ( )  B_SPLINE_CURVE ( 3, ( #8728, #21508, #24144, #11199 ),
 .UNSPECIFIED., .F., .F. ) 
 B_SPLINE_CURVE_WITH_KNOTS ( ( 4, 4 ),
 ( 4.712388980384687009, 6.283185307179586232 ),
 .UNSPECIFIED. ) 
 CURVE ( )  GEOMETRIC_REPRESENTATION_ITEM ( )  RATIONAL_B_SPLINE_CURVE ( ( 1.000000000000000000, 0.8047378541243643824, 0.8047378541243643824, 1.000000000000000000 ) ) 
 REPRESENTATION_ITEM ( '' )  );
#26041 = ORIENTED_EDGE ( 'NONE', *, *, #11524, .F. ) ;
#26042 = FACE_OUTER_BOUND ( 'NONE', #4384, .T. ) ;
#26043 = ADVANCED_FACE ( 'NONE', ( #24326 ), #10396, .T. ) ;
#26044 = ADVANCED_FACE ( 'NONE', ( #29928 ), #22295, .T. ) ;
#26045 = ORIENTED_EDGE ( 'NONE', *, *, #31985, .F. ) ;
#26046 = AXIS2_PLACEMENT_3D ( 'NONE', #14748, #25075, #2588 ) ;
#26047 = ORIENTED_EDGE ( 'NONE', *, *, #482, .T. ) ;
#26048 = CARTESIAN_POINT ( 'NONE',  ( 21.09785597605719332, 17.16451738380053271, 47.04930799450051637 ) ) ;
#26049 = EDGE_CURVE ( 'NONE', #8721, #23768, #13547, .T. ) ;
#26050 = ORIENTED_EDGE ( 'NONE', *, *, #20038, .F. ) ;
#26051 = CARTESIAN_POINT ( 'NONE',  ( 33.50134396954525329, 26.09164230456639899, 47.04930799450051637 ) ) ;
#26052 = DIRECTION ( 'NONE',  ( -0.000000000000000000, -1.000000000000000000, 0.000000000000000000 ) ) ;
#26053 = CARTESIAN_POINT ( 'NONE',  ( 52.20364351894168919, -5.936611295272324895, 106.6063773940375228 ) ) ;
#26054 = CARTESIAN_POINT ( 'NONE',  ( 44.74832014356462651, 25.58456182964376779, 46.92728461490987257 ) ) ;
#26055 = ORIENTED_EDGE ( 'NONE', *, *, #28029, .F. ) ;
#26056 = ORIENTED_EDGE ( 'NONE', *, *, #17488, .T. ) ;
#26057 = SURFACE_STYLE_FILL_AREA ( #8350 ) ;
#26058 = ORIENTED_EDGE ( 'NONE', *, *, #4157, .T. ) ;
#26059 = DIRECTION ( 'NONE',  ( -1.101824276508909887E-16, 1.000000000000000000, -0.000000000000000000 ) ) ;
#26060 = CARTESIAN_POINT ( 'NONE',  ( 47.09785597605719687, 25.56454579224779877, 44.54930799450042400 ) ) ;
#26061 = CIRCLE ( 'NONE', #11916, 12.36707279061065101 ) ;
#26062 = CARTESIAN_POINT ( 'NONE',  ( 49.40414881150629611, 22.80400562401889530, 47.16908566558144855 ) ) ;
#26063 = LINE ( 'NONE', #16058, #14220 ) ;
#26064 = DIRECTION ( 'NONE',  ( 0.000000000000000000, 1.000000000000000000, -0.000000000000000000 ) ) ;
#26065 = EDGE_CURVE ( 'NONE', #22190, #28560, #419, .T. ) ;
#26066 = ORIENTED_EDGE ( 'NONE', *, *, #6481, .T. ) ;
#26067 = DIRECTION ( 'NONE',  ( 0.000000000000000000, 0.000000000000000000, -1.000000000000000000 ) ) ;
#26068 = CARTESIAN_POINT ( 'NONE',  ( -34.91457700022733945, -4.675691201108098660, 13.95142249688010949 ) ) ;
#26069 = AXIS2_PLACEMENT_3D ( 'NONE', #1692, #2186, #11712 ) ;
#26070 = DIRECTION ( 'NONE',  ( -1.000000000000000000, 0.000000000000000000, 0.000000000000000000 ) ) ;
#26071 = AXIS2_PLACEMENT_3D ( 'NONE', #1936, #27049, #31814 ) ;
#26072 = EDGE_CURVE ( 'NONE', #27014, #28135, #4612, .T. ) ;
#26073 = CARTESIAN_POINT ( 'NONE',  ( 48.79980305660560447, 22.93328494799376571, 46.81390877062097644 ) ) ;
#26074 = CARTESIAN_POINT ( 'NONE',  ( -40.39697993529618003, 8.288924485351975235, 54.52001867261917312 ) ) ;
#26075 = CARTESIAN_POINT ( 'NONE',  ( 47.09785597605719687, 24.86454579224779948, 47.04930799450042400 ) ) ;
#26076 = AXIS2_PLACEMENT_3D ( 'NONE', #1687, #11709, #9571 ) ;
#26077 = ORIENTED_EDGE ( 'NONE', *, *, #14891, .T. ) ;
#26078 = DIRECTION ( 'NONE',  ( -1.000000000000000000, 0.000000000000000000, 0.000000000000000000 ) ) ;
#26079 = CARTESIAN_POINT ( 'NONE',  ( -40.23672901771082877, 7.760455916344221272, 39.54930799450052348 ) ) ;
#26080 = ADVANCED_FACE ( 'NONE', ( #5133 ), #27457, .F. ) ;
#26081 = EDGE_CURVE ( 'NONE', #12497, #17250, #3036, .T. ) ;
#26082 = AXIS2_PLACEMENT_3D ( 'NONE', #28968, #29286, #4012 ) ;
#26083 = EDGE_CURVE ( 'NONE', #16169, #21481, #516, .T. ) ;
#26084 = ORIENTED_EDGE ( 'NONE', *, *, #18554, .F. ) ;
#26085 = VERTEX_POINT ( 'NONE', #20061 ) ;
#26086 = DIRECTION ( 'NONE',  ( -1.224646799147353207E-16, -1.349345573449484691E-32, 1.000000000000000000 ) ) ;
#26087 = TOROIDAL_SURFACE ( 'NONE', #22406, 55.72393233686778302, 0.09999999999999760469 ) ;
#26088 = FACE_BOUND ( 'NONE', #18686, .T. ) ;
#26089 = DIRECTION ( 'NONE',  ( 0.000000000000000000, 0.000000000000000000, -1.000000000000000000 ) ) ;
#26090 = AXIS2_PLACEMENT_3D ( 'NONE', #17500, #27516, #7162 ) ;
#26091 = VERTEX_POINT ( 'NONE', #5460 ) ;
#26092 = AXIS2_PLACEMENT_3D ( 'NONE', #12735, #20255, #28302 ) ;
#26093 = CARTESIAN_POINT ( 'NONE',  ( 21.09785597605720753, 13.86454579224779948, 47.04930799450052348 ) ) ;
#26094 = VECTOR ( 'NONE', #2101, 1000.000000000000000 ) ;
#26095 = FACE_OUTER_BOUND ( 'NONE', #2341, .T. ) ;
#26096 = DIRECTION ( 'NONE',  ( 0.4848096202463673676, 0.8746197071393789768, 0.000000000000000000 ) ) ;
#26097 = ORIENTED_EDGE ( 'NONE', *, *, #13229, .T. ) ;
#26098 = CARTESIAN_POINT ( 'NONE',  ( 47.23884743062419744, 22.86454579224779948, 45.05393496349946503 ) ) ;
#26099 = ORIENTED_EDGE ( 'NONE', *, *, #27050, .T. ) ;
#26100 = DIRECTION ( 'NONE',  ( -0.000000000000000000, -1.000000000000000000, -0.000000000000000000 ) ) ;
#26101 = VECTOR ( 'NONE', #11697, 1000.000000000000114 ) ;
#26102 = DIRECTION ( 'NONE',  ( -1.101824276508909887E-16, 1.000000000000000000, -0.000000000000000000 ) ) ;
#26103 = LINE ( 'NONE', #8236, #9563 ) ;
#26104 = DIRECTION ( 'NONE',  ( 0.8746197071393926326, -0.4848096202463430537, -8.676864087101709653E-18 ) ) ;
#26105 = ADVANCED_FACE ( 'NONE', ( #15463 ), #19821, .T. ) ;
#26106 =( LENGTH_UNIT ( ) NAMED_UNIT ( * ) SI_UNIT ( .MILLI., .METRE. ) );
#26107 = ORIENTED_EDGE ( 'NONE', *, *, #913, .F. ) ;
#26108 = ORIENTED_EDGE ( 'NONE', *, *, #23027, .F. ) ;
#26109 = DIRECTION ( 'NONE',  ( -1.101824276508909887E-16, 1.000000000000000000, -0.000000000000000000 ) ) ;
#26110 = CARTESIAN_POINT ( 'NONE',  ( 21.09992658989238734, 31.84184655352418503, 47.04930799450051637 ) ) ;
#26111 = EDGE_CURVE ( 'NONE', #13529, #18870, #20706, .T. ) ;
#26112 = DIRECTION ( 'NONE',  ( 0.2756373558169974980, -0.9612616959383193382, -1.315048337272770589E-17 ) ) ;
#26113 = ORIENTED_EDGE ( 'NONE', *, *, #29715, .F. ) ;
#26114 = CARTESIAN_POINT ( 'NONE',  ( 21.09785597605719332, 17.16451738380053271, 60.03349819502753348 ) ) ;
#26115 = DIRECTION ( 'NONE',  ( 0.4544104193609905806, 5.611869858668446909E-17, 0.8907924397839086517 ) ) ;
#26116 = ORIENTED_EDGE ( 'NONE', *, *, #9719, .T. ) ;
#26117 = CARTESIAN_POINT ( 'NONE',  ( 33.72499318558949710, 27.59143805560860940, 47.04930799450051637 ) ) ;
#26118 = CARTESIAN_POINT ( 'NONE',  ( 45.46000861347822308, 27.47287913140503690, 49.57397645940629616 ) ) ;
#26119 = AXIS2_PLACEMENT_3D ( 'NONE', #6107, #1177, #18248 ) ;
#26120 = CIRCLE ( 'NONE', #21388, 0.7928932188134565351 ) ;
#26121 = ADVANCED_FACE ( 'NONE', ( #22845 ), #16668, .T. ) ;
#26122 = AXIS2_PLACEMENT_3D ( 'NONE', #22967, #2949, #2637 ) ;
#26123 = CARTESIAN_POINT ( 'NONE',  ( 21.09785597605719332, -9.935454207752199451, 47.04930799450051637 ) ) ;
#26124 = EDGE_CURVE ( 'NONE', #25360, #15904, #12490, .T. ) ;
#26125 = CIRCLE ( 'NONE', #11973, 1.042135311067126979 ) ;
#26126 = CIRCLE ( 'NONE', #20351, 15.28675991284684343 ) ;
#26127 = B_SPLINE_CURVE_WITH_KNOTS ( 'NONE', 3,
 ( #25490, #13025, #10725, #3149, #13194, #23186, #20721, #30747, #8254, #18241, #6431, #16588 ),
 .UNSPECIFIED., .F., .F.,
 ( 4, 2, 2, 2, 2, 4 ),
 ( 0.0002000209647945283933, 0.001054195637184463354, 0.001481282973379431742, 0.001908370309574400348, 0.002762544981964341027, 0.003616719654354280840 ),
 .UNSPECIFIED. ) ;
#26128 = TOROIDAL_SURFACE ( 'NONE', #29289, 12.61792373059895134, 0.1249999999999985151 ) ;
#26129 = ORIENTED_EDGE ( 'NONE', *, *, #31274, .T. ) ;
#26130 = DIRECTION ( 'NONE',  ( 0.000000000000000000, -0.000000000000000000, -1.000000000000000000 ) ) ;
#26131 = CARTESIAN_POINT ( 'NONE',  ( 49.32483701613094240, 28.52587066347689415, 45.91328182968236860 ) ) ;
#26132 = LINE ( 'NONE', #8421, #9628 ) ;
#26133 = EDGE_LOOP ( 'NONE', ( #20169, #25904, #8707, #27241 ) ) ;
#26134 = DIRECTION ( 'NONE',  ( -0.000000000000000000, -1.000000000000000000, 0.000000000000000000 ) ) ;
#26135 = DIRECTION ( 'NONE',  ( -0.9612616959383186721, -0.2756373558169996629, -8.795445018805237002E-19 ) ) ;
#26136 = AXIS2_PLACEMENT_3D ( 'NONE', #26746, #19673, #29702 ) ;
#26137 = VECTOR ( 'NONE', #11556, 1000.000000000000227 ) ;
#26138 = EDGE_LOOP ( 'NONE', ( #27461, #22935, #6187, #8249 ) ) ;
#26139 = FACE_OUTER_BOUND ( 'NONE', #30942, .T. ) ;
#26140 = TOROIDAL_SURFACE ( 'NONE', #4122, 12.40141737965288193, 0.1250000000000005829 ) ;
#26141 = DIRECTION ( 'NONE',  ( 0.9097384655268496711, 0.4151817967359032746, -1.524080105319609646E-17 ) ) ;
#26142 = CARTESIAN_POINT ( 'NONE',  ( 48.23388202445966044, 28.35087065737811685, 49.27628909396054979 ) ) ;
#26143 = DIRECTION ( 'NONE',  ( 1.000000000000000000, 0.000000000000000000, -1.224646799147353207E-16 ) ) ;
#26144 = CARTESIAN_POINT ( 'NONE',  ( -40.58095149058966200, 7.465239395913044973, 60.18771704643254594 ) ) ;
#26145 = EDGE_LOOP ( 'NONE', ( #20102, #8775, #12768, #24469, #27970 ) ) ;
#26146 = DIRECTION ( 'NONE',  ( -0.000000000000000000, -1.000000000000000000, 0.000000000000000000 ) ) ;
#26147 = CARTESIAN_POINT ( 'NONE',  ( 33.46699938050304013, 32.21183152705962272, 47.04930799450051637 ) ) ;
#26148 = CARTESIAN_POINT ( 'NONE',  ( -40.38516919650994197, 8.640923867788874446, 34.64930799450051779 ) ) ;
#26149 = LINE ( 'NONE', #23847, #32366 ) ;
#26150 = CIRCLE ( 'NONE', #24061, 67.32891250266496286 ) ;
#26151 = CARTESIAN_POINT ( 'NONE',  ( 21.09785597605720753, 13.86454579224779948, 47.04930799450052348 ) ) ;
#26152 = ORIENTED_EDGE ( 'NONE', *, *, #5837, .F. ) ;
#26153 = CARTESIAN_POINT ( 'NONE',  ( 48.15252827834996907, 29.60698769386672424, 45.26040870260538895 ) ) ;
#26154 = CARTESIAN_POINT ( 'NONE',  ( 49.66186032787856419, 24.92772031883689010, 46.53160128828346132 ) ) ;
#26155 = CARTESIAN_POINT ( 'NONE',  ( 48.41757674592806637, 19.86454579224779948, 45.01501767854993119 ) ) ;
#26156 = EDGE_LOOP ( 'NONE', ( #26809, #26759, #9833, #27565 ) ) ;
#26157 = CARTESIAN_POINT ( 'NONE',  ( -40.66586793973302605, 8.138261812237592707, 59.50788663826320146 ) ) ;
#26158 = CARTESIAN_POINT ( 'NONE',  ( 48.19974268340787660, 19.86454579224779948, 49.20936486508634289 ) ) ;
#26159 = CARTESIAN_POINT ( 'NONE',  ( 48.83059987400639557, 28.95948166895302833, 48.97189179988551899 ) ) ;
#26160 = ADVANCED_FACE ( 'NONE', ( #689 ), #6210, .T. ) ;
#26161 = CARTESIAN_POINT ( 'NONE',  ( 53.14761115485138276, 2.529769287487982687, -5.868558487217412356 ) ) ;
#26162 = EDGE_CURVE ( 'NONE', #1265, #11047, #30246, .T. ) ;
#26163 = EDGE_LOOP ( 'NONE', ( #15460, #14348, #18285, #13794 ) ) ;
#26164 = ADVANCED_FACE ( 'NONE', ( #8088 ), #31915, .T. ) ;
#26165 = CARTESIAN_POINT ( 'NONE',  ( -41.07560527903737579, 9.385057823277968225, 39.44930799450052206 ) ) ;
#26166 = ORIENTED_EDGE ( 'NONE', *, *, #23846, .F. ) ;
#26167 = CIRCLE ( 'NONE', #12574, 12.36707279061065101 ) ;
#26168 = VECTOR ( 'NONE', #1370, 1000.000000000000000 ) ;
#26169 = VERTEX_POINT ( 'NONE', #28111 ) ;
#26170 = AXIS2_PLACEMENT_3D ( 'NONE', #16791, #4491, #28786 ) ;
#26171 = AXIS2_PLACEMENT_3D ( 'NONE', #4410, #11644, #19501 ) ;
#26172 = CARTESIAN_POINT ( 'NONE',  ( 21.09992658989239089, 23.72145308207319658, 47.04930799450051637 ) ) ;
#26173 = CARTESIAN_POINT ( 'NONE',  ( 81.79463805813215060, -5.936463533621012090, 77.90792605297762918 ) ) ;
#26174 = ORIENTED_EDGE ( 'NONE', *, *, #20482, .F. ) ;
#26175 = CARTESIAN_POINT ( 'NONE',  ( -41.09927805198056916, 10.76852187697755880, 36.12712545380572493 ) ) ;
#26176 = ORIENTED_EDGE ( 'NONE', *, *, #24199, .F. ) ;
#26177 = DIRECTION ( 'NONE',  ( -1.101824276508909887E-16, 1.000000000000000000, -0.000000000000000000 ) ) ;
#26178 = FACE_OUTER_BOUND ( 'NONE', #31455, .T. ) ;
#26179 = CARTESIAN_POINT ( 'NONE',  ( -42.67312000749024747, 15.16877446138198238, 38.54930799450052348 ) ) ;
#26180 = ORIENTED_EDGE ( 'NONE', *, *, #18961, .F. ) ;
#26181 = FACE_OUTER_BOUND ( 'NONE', #20472, .T. ) ;
#26182 = FACE_OUTER_BOUND ( 'NONE', #12051, .T. ) ;
#26183 = DIRECTION ( 'NONE',  ( -1.101824276508909887E-16, 1.000000000000000000, -0.000000000000000000 ) ) ;
#26184 = CYLINDRICAL_SURFACE ( 'NONE', #4864, 12.36707279061065279 ) ;
#26185 = AXIS2_PLACEMENT_3D ( 'NONE', #11737, #21399, #11897 ) ;
#26186 = VERTEX_POINT ( 'NONE', #847 ) ;
#26187 = CARTESIAN_POINT ( 'NONE',  ( 21.09785597605719332, 25.56454579224779167, 47.04930799450051637 ) ) ;
#26188 = AXIS2_PLACEMENT_3D ( 'NONE', #21678, #9546, #7240 ) ;
#26189 = CARTESIAN_POINT ( 'NONE',  ( 33.46699938050302592, 31.97145308207317882, 47.04930799450050927 ) ) ;
#26190 = DIRECTION ( 'NONE',  ( 0.2072038891212098777, -0.4540212254542328463, 0.8665629089512670857 ) ) ;
#26191 = FACE_OUTER_BOUND ( 'NONE', #14952, .T. ) ;
#26192 = CARTESIAN_POINT ( 'NONE',  ( 48.83862994770794330, 25.85457786121582302, 48.17861352429476796 ) ) ;
#26193 = ORIENTED_EDGE ( 'NONE', *, *, #6439, .F. ) ;
#26194 = CARTESIAN_POINT ( 'NONE',  ( 47.37889090789306579, 23.12036939723557083, 47.06390358666074292 ) ) ;
#26195 = CARTESIAN_POINT ( 'NONE',  ( -40.55769077061455619, 7.370228602978611043, 35.39483402557622327 ) ) ;
#26196 = VERTEX_POINT ( 'NONE', #26281 ) ;
#26197 = FACE_OUTER_BOUND ( 'NONE', #30371, .T. ) ;
#26198 = AXIS2_PLACEMENT_3D ( 'NONE', #14668, #17274, #17108 ) ;
#26199 = AXIS2_PLACEMENT_3D ( 'NONE', #29766, #7452, #4818 ) ;
#26200 = CARTESIAN_POINT ( 'NONE',  ( -41.50472230201275892, 5.945882615091422352, 57.04930799450051637 ) ) ;
#26201 = ADVANCED_FACE ( 'NONE', ( #11188 ), #26140, .T. ) ;
#26202 = EDGE_CURVE ( 'NONE', #8364, #16525, #2558, .T. ) ;
#26203 = ORIENTED_EDGE ( 'NONE', *, *, #20222, .T. ) ;
#26204 = EDGE_CURVE ( 'NONE', #11711, #12276, #5780, .T. ) ;
#26205 = AXIS2_PLACEMENT_3D ( 'NONE', #8433, #23522, #23835 ) ;
#26206 = ORIENTED_EDGE ( 'NONE', *, *, #17195, .T. ) ;
#26207 = ADVANCED_FACE ( 'NONE', ( #25792 ), #31052, .F. ) ;
#26208 = AXIS2_PLACEMENT_3D ( 'NONE', #6172, #23569, #21410 ) ;
#26209 = AXIS2_PLACEMENT_3D ( 'NONE', #31497, #26725, #18999 ) ;
#26210 = ORIENTED_EDGE ( 'NONE', *, *, #4571, .T. ) ;
#26211 = CIRCLE ( 'NONE', #7370, 55.85791022362053582 ) ;
#26212 = ORIENTED_EDGE ( 'NONE', *, *, #15958, .F. ) ;
#26213 = DIRECTION ( 'NONE',  ( 0.000000000000000000, 0.000000000000000000, 1.000000000000000000 ) ) ;
#26214 = AXIS2_PLACEMENT_3D ( 'NONE', #30843, #30688, #2936 ) ;
#26215 = AXIS2_PLACEMENT_3D ( 'NONE', #30870, #3447, #3608 ) ;
#26216 = EDGE_LOOP ( 'NONE', ( #28242, #26176, #30254, #11401 ) ) ;
#26217 = CARTESIAN_POINT ( 'NONE',  ( 48.54667866842090973, 22.95310733321322161, 47.81819468219185865 ) ) ;
#26218 = TOROIDAL_SURFACE ( 'NONE', #12089, 12.40141737965280200, 0.1249999999999999445 ) ;
#26219 = DIRECTION ( 'NONE',  ( -0.000000000000000000, -1.000000000000000000, -0.000000000000000000 ) ) ;
#26220 = CARTESIAN_POINT ( 'NONE',  ( 45.28286642839709231, 27.04289516297709639, 47.97516931882780966 ) ) ;
#26221 = CIRCLE ( 'NONE', #16268, 12.27848799348798892 ) ;
#26222 = CIRCLE ( 'NONE', #2644, 46.27992121592387065 ) ;
#26223 = EDGE_CURVE ( 'NONE', #12384, #15696, #4641, .T. ) ;
#26224 = ORIENTED_EDGE ( 'NONE', *, *, #14354, .F. ) ;
#26225 = EDGE_LOOP ( 'NONE', ( #16845, #6726, #21885, #18663 ) ) ;
#26226 = DIRECTION ( 'NONE',  ( -1.000000000000000000, 0.000000000000000000, 0.000000000000000000 ) ) ;
#26227 = EDGE_CURVE ( 'NONE', #13441, #116, #30349, .T. ) ;
#26228 = VECTOR ( 'NONE', #612, 1000.000000000000000 ) ;
#26229 = ORIENTED_EDGE ( 'NONE', *, *, #7233, .F. ) ;
#26230 = DIRECTION ( 'NONE',  ( -0.4848096202463368365, -0.8746197071393959632, 0.000000000000000000 ) ) ;
#26231 = CARTESIAN_POINT ( 'NONE',  ( -40.55769077061466987, 7.370228602979226551, 38.70378196342478105 ) ) ;
#26232 = LINE ( 'NONE', #13605, #10253 ) ;
#26233 = CARTESIAN_POINT ( 'NONE',  ( -5.602943079677954685, 9.702389020015065313, 132.0493079945005377 ) ) ;
#26234 =( BOUNDED_SURFACE ( )  B_SPLINE_SURFACE ( 1, 2, ( 
 ( #29443, #27132, #29937, #7451, #26811, #2359, #4328, #32235, #12378, #17278, #9415, #12040, #6952, #24502, #7114, #27300, #4817, #22365, #5472, #5623, #28272, #18238, #10391, #27952, #25643, #5791, #20232, #22527, #3146, #22856, #17770, #2512, #10723, #8097, #15473, #15797, #12539, #58, #25487, #12711, #369, #23183, #5142, #20073, #25330, #20390, #13191, #5311, #10564, #27789, #10076, #2680, #30102, #698, #7610, #2988, #20716, #13019, #17933, #15624, #30744, #30257, #2833, #17609, #27626, #23015, #15316, #8251, #15155, #7769, #20554, #12865, #533, #25164, #22700, #216, #10236, #30420, #7937, #30585, #18091, #28118, #13822, #28436, #3638 ),
 ( #8570, #28921, #18562, #28591, #30898, #11507, #11196, #16269, #21506, #16430, #13345, #6103, #25804, #26288, #29069, #16104, #3315, #23978, #8411, #21027, #18406, #5956, #31544, #6428, #1489, #23502, #15950, #23344, #3474, #21179, #855, #31225, #3795, #8726, #23813, #26444, #10880, #31376, #1331, #20870, #19044, #25958, #9050, #11353, #1169, #18882, #13983, #26118, #13663, #3962, #18714, #13502, #6590, #1015, #11041, #28745, #6263, #31060, #23665, #21338, #8884, #9705, #11682, #12333, #29403, #11842, #9374, #29231, #2154, #16584, #19370, #6745, #24796, #21835, #24307, #31858, #32355, #14307, #7074, #26934, #16745, #9864, #21992, #26771, #29569 ) ),
 .UNSPECIFIED., .F., .F., .F. ) 
 B_SPLINE_SURFACE_WITH_KNOTS ( ( 2, 2 ),
 ( 3, 2, 2, 2, 2, 2, 2, 2, 2, 2, 2, 2, 2, 2, 2, 2, 2, 2, 2, 2, 2, 2, 2, 2, 2, 2, 2, 2, 2, 2, 2, 2, 2, 2, 2, 2, 2, 2, 2, 2, 2, 2, 3 ),
 ( 0.000000000000000000, 1.000000000000000000 ),
 ( 0.000000000000000000, 0.02380952380952380820, 0.04761904761904761640, 0.07142857142857142461, 0.09523809523809523281, 0.1190476190476190410, 0.1428571428571428492, 0.1666666666666666574, 0.1904761904761904656, 0.2142857142857142738, 0.2380952380952380820, 0.2619047619047619180, 0.2857142857142856984, 0.3095238095238095344, 0.3333333333333333148, 0.3571428571428571508, 0.3809523809523809312, 0.4047619047619047672, 0.4285714285714285476, 0.4523809523809523836, 0.4761904761904761640, 0.5000000000000000000, 0.5238095238095238360, 0.5476190476190476719, 0.5714285714285713969, 0.5952380952380952328, 0.6190476190476190688, 0.6428571428571429047, 0.6666666666666666297, 0.6904761904761904656, 0.7142857142857143016, 0.7380952380952381375, 0.7619047619047618625, 0.7857142857142856984, 0.8095238095238095344, 0.8333333333333333703, 0.8571428571428570953, 0.8809523809523809312, 0.9047619047619047672, 0.9285714285714286031, 0.9523809523809523281, 0.9761904761904761640, 1.000000000000000000 ),
 .UNSPECIFIED. ) 
 GEOMETRIC_REPRESENTATION_ITEM ( )  RATIONAL_B_SPLINE_SURFACE ( (
 ( 1.000000000000000000, 0.8660254037844387076, 1.000000000000000000, 0.8660254037844387076, 1.000000000000000000, 0.8660254037844387076, 1.000000000000000000, 0.8660254037844387076, 1.000000000000000000, 0.8660254037844387076, 1.000000000000000000, 0.8660254037844387076, 1.000000000000000000, 0.8660254037844387076, 1.000000000000000000, 0.8660254037844387076, 1.000000000000000000, 0.8660254037844387076, 1.000000000000000000, 0.8660254037844387076, 1.000000000000000000, 0.8660254037844387076, 1.000000000000000000, 0.8660254037844387076, 1.000000000000000000, 0.8660254037844387076, 1.000000000000000000, 0.8660254037844387076, 1.000000000000000000, 0.8660254037844387076, 1.000000000000000000, 0.8660254037844387076, 1.000000000000000000, 0.8660254037844387076, 1.000000000000000000, 0.8660254037844387076, 1.000000000000000000, 0.8660254037844387076, 1.000000000000000000, 0.8660254037844387076, 1.000000000000000000, 0.8660254037844387076, 1.000000000000000000, 0.8660254037844387076, 1.000000000000000000, 0.8660254037844387076, 1.000000000000000000, 0.8660254037844387076, 1.000000000000000000, 0.8660254037844387076, 1.000000000000000000, 0.8660254037844387076, 1.000000000000000000, 0.8660254037844387076, 1.000000000000000000, 0.8660254037844387076, 1.000000000000000000, 0.8660254037844387076, 1.000000000000000000, 0.8660254037844387076, 1.000000000000000000, 0.8660254037844387076, 1.000000000000000000, 0.8660254037844387076, 1.000000000000000000, 0.8660254037844387076, 1.000000000000000000, 0.8660254037844387076, 1.000000000000000000, 0.8660254037844387076, 1.000000000000000000, 0.8660254037844387076, 1.000000000000000000, 0.8660254037844387076, 1.000000000000000000, 0.8660254037844387076, 1.000000000000000000, 0.8660254037844387076, 1.000000000000000000, 0.8660254037844387076, 1.000000000000000000, 0.8660254037844387076, 1.000000000000000000, 0.8660254037844387076, 1.000000000000000000),
 ( 1.000000000000000000, 0.8660254037844387076, 1.000000000000000000, 0.8660254037844387076, 1.000000000000000000, 0.8660254037844387076, 1.000000000000000000, 0.8660254037844387076, 1.000000000000000000, 0.8660254037844387076, 1.000000000000000000, 0.8660254037844387076, 1.000000000000000000, 0.8660254037844387076, 1.000000000000000000, 0.8660254037844387076, 1.000000000000000000, 0.8660254037844387076, 1.000000000000000000, 0.8660254037844387076, 1.000000000000000000, 0.8660254037844387076, 1.000000000000000000, 0.8660254037844387076, 1.000000000000000000, 0.8660254037844387076, 1.000000000000000000, 0.8660254037844387076, 1.000000000000000000, 0.8660254037844387076, 1.000000000000000000, 0.8660254037844387076, 1.000000000000000000, 0.8660254037844387076, 1.000000000000000000, 0.8660254037844387076, 1.000000000000000000, 0.8660254037844387076, 1.000000000000000000, 0.8660254037844387076, 1.000000000000000000, 0.8660254037844387076, 1.000000000000000000, 0.8660254037844387076, 1.000000000000000000, 0.8660254037844387076, 1.000000000000000000, 0.8660254037844387076, 1.000000000000000000, 0.8660254037844387076, 1.000000000000000000, 0.8660254037844387076, 1.000000000000000000, 0.8660254037844387076, 1.000000000000000000, 0.8660254037844387076, 1.000000000000000000, 0.8660254037844387076, 1.000000000000000000, 0.8660254037844387076, 1.000000000000000000, 0.8660254037844387076, 1.000000000000000000, 0.8660254037844387076, 1.000000000000000000, 0.8660254037844387076, 1.000000000000000000, 0.8660254037844387076, 1.000000000000000000, 0.8660254037844387076, 1.000000000000000000, 0.8660254037844387076, 1.000000000000000000, 0.8660254037844387076, 1.000000000000000000, 0.8660254037844387076, 1.000000000000000000, 0.8660254037844387076, 1.000000000000000000, 0.8660254037844387076, 1.000000000000000000, 0.8660254037844387076, 1.000000000000000000, 0.8660254037844387076, 1.000000000000000000) ) ) 
 REPRESENTATION_ITEM ( '' )  SURFACE ( )  );
#26235 = DIRECTION ( 'NONE',  ( -0.2756373558170082672, 0.9612616959383162296, 0.000000000000000000 ) ) ;
#26236 = DIRECTION ( 'NONE',  ( -1.101824276508909887E-16, 1.000000000000000000, -0.000000000000000000 ) ) ;
#26237 = ORIENTED_EDGE ( 'NONE', *, *, #13279, .F. ) ;
#26238 = DIRECTION ( 'NONE',  ( 0.000000000000000000, 0.000000000000000000, -1.000000000000000000 ) ) ;
#26239 = CARTESIAN_POINT ( 'NONE',  ( 33.50134396954518934, 32.09164230456639899, 47.04930799450051637 ) ) ;
#26240 = AXIS2_PLACEMENT_3D ( 'NONE', #2971, #30883, #20539 ) ;
#26241 = FACE_OUTER_BOUND ( 'NONE', #5739, .T. ) ;
#26242 = DIRECTION ( 'NONE',  ( 0.000000000000000000, 0.000000000000000000, -1.000000000000000000 ) ) ;
#26243 = DIRECTION ( 'NONE',  ( -1.101824276508909887E-16, 1.000000000000000000, -0.000000000000000000 ) ) ;
#26244 = ORIENTED_EDGE ( 'NONE', *, *, #25358, .F. ) ;
#26245 = FACE_OUTER_BOUND ( 'NONE', #22774, .T. ) ;
#26246 = ORIENTED_EDGE ( 'NONE', *, *, #30471, .F. ) ;
#26247 = LINE ( 'NONE', #19169, #16214 ) ;
#26248 = CARTESIAN_POINT ( 'NONE',  ( 40.31237200149237765, 7.264443105416139801, 47.04930799450051637 ) ) ;
#26249 = EDGE_CURVE ( 'NONE', #18953, #9681, #10961, .T. ) ;
#26250 = CIRCLE ( 'NONE', #27831, 12.68414152717711119 ) ;
#26251 = ORIENTED_EDGE ( 'NONE', *, *, #12776, .T. ) ;
#26252 = CIRCLE ( 'NONE', #12103, 12.36707279061065101 ) ;
#26253 = VECTOR ( 'NONE', #16168, 1000.000000000000000 ) ;
#26254 = AXIS2_PLACEMENT_3D ( 'NONE', #26151, #26478, #23849 ) ;
#26255 = B_SPLINE_CURVE_WITH_KNOTS ( 'NONE', 3,
 ( #12715, #14455, #22636, #19846, #156, #2134, #15096, #24779, #9846, #2295 ),
 .UNSPECIFIED., .F., .F.,
 ( 4, 2, 2, 2, 4 ),
 ( 2.968785590477208419E-05, 0.0003298221638443240276, 0.0006299564717838759473, 0.0009300907797234278128, 0.001230225087662979678 ),
 .UNSPECIFIED. ) ;
#26256 = VERTEX_POINT ( 'NONE', #20865 ) ;
#26257 = EDGE_CURVE ( 'NONE', #6352, #10039, #3603, .T. ) ;
#26258 = CARTESIAN_POINT ( 'NONE',  ( 48.82187354100420151, 22.88065857334294861, 46.16985335424439540 ) ) ;
#26259 = CARTESIAN_POINT ( 'NONE',  ( 33.72499318558949000, 38.56284415653841791, 47.04930799450051637 ) ) ;
#26260 = LINE ( 'NONE', #3769, #13654 ) ;
#26261 = EDGE_CURVE ( 'NONE', #1392, #11505, #23658, .T. ) ;
#26262 = ORIENTED_EDGE ( 'NONE', *, *, #32139, .F. ) ;
#26263 = CARTESIAN_POINT ( 'NONE',  ( -29.06857593705904819, -13.30632128221580857, 22.31577484639326769 ) ) ;
#26264 = FACE_OUTER_BOUND ( 'NONE', #1417, .T. ) ;
#26265 = CARTESIAN_POINT ( 'NONE',  ( 74.00358335591296566, 2.565965067347307116, 15.01823474329995811 ) ) ;
#26266 = EDGE_CURVE ( 'NONE', #7305, #17564, #31369, .T. ) ;
#26267 = ORIENTED_EDGE ( 'NONE', *, *, #11893, .T. ) ;
#26268 = CARTESIAN_POINT ( 'NONE',  ( 33.72499318558949710, 25.09184655352419213, 47.04930799450051637 ) ) ;
#26269 = ADVANCED_FACE ( 'NONE', ( #1161 ), #3467, .F. ) ;
#26270 = VERTEX_POINT ( 'NONE', #1007 ) ;
#26271 = ADVANCED_FACE ( 'NONE', ( #3307 ), #21941, .T. ) ;
#26272 = DIRECTION ( 'NONE',  ( 0.000000000000000000, 0.000000000000000000, -1.000000000000000000 ) ) ;
#26273 = DIRECTION ( 'NONE',  ( 0.8746197071393926326, -0.4848096202463430537, -8.676864087101709653E-18 ) ) ;
#26274 = CIRCLE ( 'NONE', #32038, 0.1250000000000001110 ) ;
#26275 = FACE_OUTER_BOUND ( 'NONE', #7012, .T. ) ;
#26276 = AXIS2_PLACEMENT_3D ( 'NONE', #7960, #23206, #17953 ) ;
#26277 = ORIENTED_EDGE ( 'NONE', *, *, #14948, .F. ) ;
#26278 = ORIENTED_EDGE ( 'NONE', *, *, #3782, .F. ) ;
#26279 = CARTESIAN_POINT ( 'NONE',  ( 21.09785597605719687, -13.30631372918550959, -8.763520691563154941 ) ) ;
#26280 = AXIS2_PLACEMENT_3D ( 'NONE', #29145, #18950, #28823 ) ;
#26281 = CARTESIAN_POINT ( 'NONE',  ( 34.91272994418231690, 15.57592086119046826, 47.04930799450052348 ) ) ;
#26282 = FACE_OUTER_BOUND ( 'NONE', #22632, .T. ) ;
#26283 = VERTEX_POINT ( 'NONE', #5942 ) ;
#26284 = DIRECTION ( 'NONE',  ( 0.9612616959383206705, 0.2756373558169926130, 8.795445018804289444E-19 ) ) ;
#26285 = CARTESIAN_POINT ( 'NONE',  ( 21.09785597605719332, -13.74048473023143835, -11.17459240385188934 ) ) ;
#26286 = VERTEX_POINT ( 'NONE', #16096 ) ;
#26287 = LINE ( 'NONE', #6427, #29368 ) ;
#26288 = CARTESIAN_POINT ( 'NONE',  ( 44.09250526802607340, 29.45621246473837118, 46.89322480343881949 ) ) ;
#26289 = EDGE_CURVE ( 'NONE', #2830, #6661, #16419, .T. ) ;
#26290 = DIRECTION ( 'NONE',  ( -0.000000000000000000, -1.000000000000000000, 0.000000000000000000 ) ) ;
#26291 = ORIENTED_EDGE ( 'NONE', *, *, #3712, .T. ) ;
#26292 = AXIS2_PLACEMENT_3D ( 'NONE', #5691, #25547, #23252 ) ;
#26293 = DIRECTION ( 'NONE',  ( -1.101824276508909887E-16, 1.000000000000000000, -0.000000000000000000 ) ) ;
#26294 = ADVANCED_FACE ( 'NONE', ( #23806 ), #27721, .T. ) ;
#26295 = DIRECTION ( 'NONE',  ( 0.000000000000000000, 0.000000000000000000, -1.000000000000000000 ) ) ;
#26296 = DIRECTION ( 'NONE',  ( 1.000000000000000000, 0.000000000000000000, -1.224646799147353207E-16 ) ) ;
#26297 = CARTESIAN_POINT ( 'NONE',  ( 48.91284552371730143, 25.33619643316631809, 46.12344667017377020 ) ) ;
#26298 = EDGE_CURVE ( 'NONE', #21636, #12799, #8719, .T. ) ;
#26299 = EDGE_LOOP ( 'NONE', ( #21070, #27232, #15082, #29122 ) ) ;
#26300 = FACE_OUTER_BOUND ( 'NONE', #762, .T. ) ;
#26301 = CARTESIAN_POINT ( 'NONE',  ( 21.09785597605720397, -16.43042895458278352, 119.0543332476699021 ) ) ;
#26302 = CIRCLE ( 'NONE', #13742, 12.62506659569710443 ) ;
#26303 = FACE_OUTER_BOUND ( 'NONE', #25345, .T. ) ;
#26304 = ADVANCED_FACE ( 'NONE', ( #28739 ), #23966, .T. ) ;
#26305 = VERTEX_POINT ( 'NONE', #7066 ) ;
#26306 = DIRECTION ( 'NONE',  ( 0.000000000000000000, 0.000000000000000000, -1.000000000000000000 ) ) ;
#26307 = EDGE_CURVE ( 'NONE', #28686, #23334, #32439, .T. ) ;
#26308 = DIRECTION ( 'NONE',  ( -0.000000000000000000, -1.000000000000000000, 0.000000000000000000 ) ) ;
#26309 = LINE ( 'NONE', #3818, #13641 ) ;
#26310 = CARTESIAN_POINT ( 'NONE',  ( 21.09785597605719332, 25.76454579224781227, 59.04930799450051637 ) ) ;
#26311 = EDGE_LOOP ( 'NONE', ( #31366, #19353, #1595, #19018 ) ) ;
#26312 = DIRECTION ( 'NONE',  ( 0.2756373558169938898, -0.9612616959383203374, 0.000000000000000000 ) ) ;
#26313 = CARTESIAN_POINT ( 'NONE',  ( 44.70507715278255034, 26.96291119454915020, 46.92503878583765697 ) ) ;
#26314 = CARTESIAN_POINT ( 'NONE',  ( -42.59587854516874472, -0.7667456371672803916, 32.14930799450051779 ) ) ;
#26315 = AXIS2_PLACEMENT_3D ( 'NONE', #27728, #472, #30356 ) ;
#26316 = CARTESIAN_POINT ( 'NONE',  ( 48.75540398364718442, 22.86454579224779948, 48.16909669137300654 ) ) ;
#26317 = DIRECTION ( 'NONE',  ( -1.101824276508909887E-16, 1.000000000000000000, -0.000000000000000000 ) ) ;
#26318 = ORIENTED_EDGE ( 'NONE', *, *, #4413, .T. ) ;
#26319 = CIRCLE ( 'NONE', #9576, 33.50000000000000000 ) ;
#26320 = CARTESIAN_POINT ( 'NONE',  ( 8.698509210239560474, 29.34164230456639899, 47.04930799450051637 ) ) ;
#26321 = DIRECTION ( 'NONE',  ( -1.101824276508909887E-16, 1.000000000000000000, -0.000000000000000000 ) ) ;
#26322 = CARTESIAN_POINT ( 'NONE',  ( 21.09992658989238734, 38.56284415653841791, 47.04930799450051637 ) ) ;
#26323 = ORIENTED_EDGE ( 'NONE', *, *, #30183, .T. ) ;
#26324 = DIRECTION ( 'NONE',  ( 0.000000000000000000, 1.000000000000000000, -0.000000000000000000 ) ) ;
#26325 = LINE ( 'NONE', #6301, #26168 ) ;
#26326 = DIRECTION ( 'NONE',  ( -0.000000000000000000, -1.000000000000000000, 0.000000000000000000 ) ) ;
#26327 = DIRECTION ( 'NONE',  ( 0.000000000000000000, 0.000000000000000000, 1.000000000000000000 ) ) ;
#26328 = ORIENTED_EDGE ( 'NONE', *, *, #31345, .T. ) ;
#26329 = FACE_OUTER_BOUND ( 'NONE', #30140, .T. ) ;
#26330 = VERTEX_POINT ( 'NONE', #14297 ) ;
#26331 = VERTEX_POINT ( 'NONE', #14620 ) ;
#26332 = VECTOR ( 'NONE', #12801, 1000.000000000000000 ) ;
#26333 = VECTOR ( 'NONE', #15057, 1000.000000000000000 ) ;
#26334 = CIRCLE ( 'NONE', #20034, 19.25826962553310295 ) ;
#26335 = CARTESIAN_POINT ( 'NONE',  ( -30.88361636257000598, 11.92558985988973141, 67.49515520264003499 ) ) ;
#26336 = CARTESIAN_POINT ( 'NONE',  ( -58.11219453028166981, -16.63545420775219696, 47.04930799450023926 ) ) ;
#26337 = CARTESIAN_POINT ( 'NONE',  ( 21.09992658989239089, 23.96183152705959785, 47.04930799450051637 ) ) ;
#26338 = ADVANCED_FACE ( 'NONE', ( #9534 ), #1651, .F. ) ;
#26339 = ORIENTED_EDGE ( 'NONE', *, *, #1138, .T. ) ;
#26340 = ORIENTED_EDGE ( 'NONE', *, *, #21358, .T. ) ;
#26341 = ADVANCED_FACE ( 'NONE', ( #31851 ), #26925, .T. ) ;
#26342 = CARTESIAN_POINT ( 'NONE',  ( 33.50134396954528171, 23.84164230456639544, 47.04930799450051637 ) ) ;
#26343 = CARTESIAN_POINT ( 'NONE',  ( -39.58809650894544774, 2.596771453999702661, 47.04930799450051637 ) ) ;
#26344 = LINE ( 'NONE', #29137, #26253 ) ;
#26345 = ORIENTED_EDGE ( 'NONE', *, *, #6818, .T. ) ;
#26346 = DIRECTION ( 'NONE',  ( 0.9761574614375596592, 0.2110602665713100512, 0.05069688703093144788 ) ) ;
#26347 = DIRECTION ( 'NONE',  ( -1.224646799147353207E-16, 0.000000000000000000, -1.000000000000000000 ) ) ;
#26348 = CARTESIAN_POINT ( 'NONE',  ( 8.823509210239521394, 25.59164230456639899, 47.04930799450051637 ) ) ;
#26349 = DIRECTION ( 'NONE',  ( -1.101824276508909887E-16, 1.000000000000000000, -0.000000000000000000 ) ) ;
#26350 = EDGE_LOOP ( 'NONE', ( #8376, #26442, #23796, #17042 ) ) ;
#26351 = CARTESIAN_POINT ( 'NONE',  ( 46.59775284999513900, 22.99884124225578930, 45.72485089329623520 ) ) ;
#26352 = CARTESIAN_POINT ( 'NONE',  ( 67.63274615763145903, 14.16454579224779842, 47.04930799450051637 ) ) ;
#26353 = CARTESIAN_POINT ( 'NONE',  ( -18.90214402394279603, 13.86454579224779948, 47.04930799450052348 ) ) ;
#26354 = FACE_OUTER_BOUND ( 'NONE', #29215, .T. ) ;
#26355 = CIRCLE ( 'NONE', #30566, 0.1000000000000012962 ) ;
#26356 = DIRECTION ( 'NONE',  ( -1.000000000000000000, 0.000000000000000000, 0.000000000000000000 ) ) ;
#26357 = ORIENTED_EDGE ( 'NONE', *, *, #12776, .F. ) ;
#26358 = CARTESIAN_POINT ( 'NONE',  ( -40.13646513110857938, 7.213257191582266969, 35.13906202186969097 ) ) ;
#26359 = CARTESIAN_POINT ( 'NONE',  ( -40.50410981870283678, 7.604537000166495808, 35.33853321918559942 ) ) ;
#26360 = AXIS2_PLACEMENT_3D ( 'NONE', #4543, #19474, #17166 ) ;
#26361 = ORIENTED_EDGE ( 'NONE', *, *, #12988, .F. ) ;
#26362 = CYLINDRICAL_SURFACE ( 'NONE', #5675, 12.62506659569710266 ) ;
#26363 = DIRECTION ( 'NONE',  ( -1.101824276508909887E-16, 1.000000000000000000, -0.000000000000000000 ) ) ;
#26364 = ORIENTED_EDGE ( 'NONE', *, *, #22654, .F. ) ;
#26365 = AXIS2_PLACEMENT_3D ( 'NONE', #28995, #32108, #29154 ) ;
#26366 = AXIS2_PLACEMENT_3D ( 'NONE', #9162, #16865, #9493 ) ;
#26367 = VERTEX_POINT ( 'NONE', #29560 ) ;
#26368 = ORIENTED_EDGE ( 'NONE', *, *, #13205, .F. ) ;
#26369 = B_SPLINE_CURVE_WITH_KNOTS ( 'NONE', 3,
 ( #10855, #18536, #28723, #20690, #16243, #28570, #26420, #3611, #3450, #18858, #30874, #1145, #26263, #16404, #31037, #3288, #30716, #3943, #11014, #28895, #8226, #989, #13635, #23641, #21159, #10703, #3772, #28411, #673, #13795, #21003, #11330, #23154, #15926 ),
 .UNSPECIFIED., .F., .F.,
 ( 4, 2, 2, 2, 2, 2, 2, 2, 2, 2, 2, 2, 2, 2, 2, 2, 4 ),
 ( 0.000000000000000000, 0.03125000000000000694, 0.06250000000000001388, 0.09375000000000002776, 0.1250000000000000278, 0.1562500000000000278, 0.1875000000000000555, 0.2187500000000000278, 0.2500000000000000000, 0.2812500000000000000, 0.3125000000000000000, 0.3437500000000000000, 0.3750000000000000000, 0.4062500000000000555, 0.4375000000000000555, 0.4687500000000000555, 0.5000000000000000000 ),
 .UNSPECIFIED. ) ;
#26370 = AXIS2_PLACEMENT_3D ( 'NONE', #10468, #28184, #1562 ) ;
#26371 = VERTEX_POINT ( 'NONE', #4771 ) ;
#26372 = AXIS2_PLACEMENT_3D ( 'NONE', #29169, #26869, #6197 ) ;
#26373 = FACE_OUTER_BOUND ( 'NONE', #15908, .T. ) ;
#26374 = ADVANCED_FACE ( 'NONE', ( #1814 ), #7814, .F. ) ;
#26375 = ORIENTED_EDGE ( 'NONE', *, *, #12086, .T. ) ;
#26376 = DIRECTION ( 'NONE',  ( -1.000000000000000000, 0.000000000000000000, 0.000000000000000000 ) ) ;
#26377 = TOROIDAL_SURFACE ( 'NONE', #7536, 12.61792373059859962, 0.1250000000000011380 ) ;
#26378 = ADVANCED_FACE ( 'NONE', ( #24624 ), #19317, .F. ) ;
#26379 = EDGE_CURVE ( 'NONE', #4855, #6740, #16731, .T. ) ;
#26380 = CARTESIAN_POINT ( 'NONE',  ( 47.09785597605719687, 30.56554579224779644, 44.54930799450078638 ) ) ;
#26381 = EDGE_CURVE ( 'NONE', #18056, #15722, #22152, .T. ) ;
#26382 = AXIS2_PLACEMENT_3D ( 'NONE', #30778, #23383, #15992 ) ;
#26383 = AXIS2_PLACEMENT_3D ( 'NONE', #12615, #22430, #17353 ) ;
#26384 = CYLINDRICAL_SURFACE ( 'NONE', #30171, 2.500000000000002220 ) ;
#26385 = CARTESIAN_POINT ( 'NONE',  ( 21.09785597605719332, -15.93545420775219945, 128.7593585008393973 ) ) ;
#26386 = EDGE_CURVE ( 'NONE', #23253, #9190, #2305, .T. ) ;
#26387 = EDGE_CURVE ( 'NONE', #2410, #7171, #26595, .T. ) ;
#26388 = CARTESIAN_POINT ( 'NONE',  ( 46.99218062947583974, 27.20286309983298878, 49.08406571254116102 ) ) ;
#26389 = VERTEX_POINT ( 'NONE', #17067 ) ;
#26390 = EDGE_LOOP ( 'NONE', ( #23483, #10450, #29346, #9332 ) ) ;
#26391 = CARTESIAN_POINT ( 'NONE',  ( -10.61756623293725177, -5.811083640285386487, -10.47712082112068188 ) ) ;
#26392 = ORIENTED_EDGE ( 'NONE', *, *, #26249, .T. ) ;
#26393 = DIRECTION ( 'NONE',  ( -1.224646799147353207E-16, -1.349345573449484691E-32, 1.000000000000000000 ) ) ;
#26394 = DIRECTION ( 'NONE',  ( -1.000000000000000000, 0.000000000000000000, 0.000000000000000000 ) ) ;
#26395 = LINE ( 'NONE', #1769, #23063 ) ;
#26396 = DIRECTION ( 'NONE',  ( -1.000000000000000000, 0.000000000000000000, 0.000000000000000000 ) ) ;
#26397 = CARTESIAN_POINT ( 'NONE',  ( 44.09250526802607340, 26.65621246473837402, 46.89322480343881949 ) ) ;
#26398 = DIRECTION ( 'NONE',  ( 0.000000000000000000, 0.000000000000000000, -1.000000000000000000 ) ) ;
#26399 = DIRECTION ( 'NONE',  ( -1.000000000000000000, 0.000000000000000000, 0.000000000000000000 ) ) ;
#26400 = ORIENTED_EDGE ( 'NONE', *, *, #30522, .F. ) ;
#26401 = CARTESIAN_POINT ( 'NONE',  ( 41.51205063648687599, 11.92558985988973497, -5.803495753465989893 ) ) ;
#26402 = FACE_OUTER_BOUND ( 'NONE', #9000, .T. ) ;
#26403 = DIRECTION ( 'NONE',  ( 0.000000000000000000, -1.000000000000000000, 0.000000000000000000 ) ) ;
#26404 = CIRCLE ( 'NONE', #18017, 0.09999999999999795164 ) ;
#26405 = ORIENTED_EDGE ( 'NONE', *, *, #15620, .F. ) ;
#26406 = CARTESIAN_POINT ( 'NONE',  ( 21.09992658989239089, 23.96183152705959785, 47.04930799450051637 ) ) ;
#26407 = ORIENTED_EDGE ( 'NONE', *, *, #7757, .F. ) ;
#26409 = EDGE_CURVE ( 'NONE', #18170, #1048, #4598, .T. ) ;
#26408 = DIRECTION ( 'NONE',  ( 7.539678551159015339E-17, -0.7880107536067239016, 0.6156614753256557382 ) ) ;
#26410 = CARTESIAN_POINT ( 'NONE',  ( -40.58856461370174173, 7.499380836222963254, 53.94930799450051495 ) ) ;
#26411 = AXIS2_PLACEMENT_3D ( 'NONE', #7149, #1566, #31934 ) ;
#26412 = VERTEX_POINT ( 'NONE', #19034 ) ;
#26413 = EDGE_CURVE ( 'NONE', #25382, #8568, #12531, .T. ) ;
#26414 = ORIENTED_EDGE ( 'NONE', *, *, #18477, .F. ) ;
#26415 = CYLINDRICAL_SURFACE ( 'NONE', #17030, 0.1000000000000018235 ) ;
#26416 = DIRECTION ( 'NONE',  ( 0.2756373558169947779, -0.9612616959383200044, 0.000000000000000000 ) ) ;
#26417 = CARTESIAN_POINT ( 'NONE',  ( 21.09785597605720042, -13.88867167006704939, 47.04930799450051637 ) ) ;
#26418 = VERTEX_POINT ( 'NONE', #24132 ) ;
#26419 = AXIS2_PLACEMENT_3D ( 'NONE', #14483, #4956, #24477 ) ;
#26420 = CARTESIAN_POINT ( 'NONE',  ( -6.872792942851614129, -13.30632128221581212, -1.386849490760369008 ) ) ;
#26421 = EDGE_CURVE ( 'NONE', #1958, #9202, #3065, .T. ) ;
#26422 =( BOUNDED_CURVE ( )  B_SPLINE_CURVE ( 2, ( #31244, #1040, #14169, #1353, #6285, #13521, #21696, #29095, #26468 ),
 .UNSPECIFIED., .F., .F. ) 
 B_SPLINE_CURVE_WITH_KNOTS ( ( 3, 2, 2, 2, 3 ),
 ( 0.8214285725898440305, 0.8333333333333333703, 0.8571428571428570953, 0.8809523809523809312, 0.8928571440184154273 ),
 .UNSPECIFIED. ) 
 CURVE ( )  GEOMETRIC_REPRESENTATION_ITEM ( )  RATIONAL_B_SPLINE_CURVE ( ( 0.9330127018922200755, 0.9330127084266224280, 1.000000000000000000, 0.8660254037844388186, 1.000000000000000000, 0.8660254037844388186, 1.000000000000000000, 0.9330126953578163906, 0.9330127018922200755 ) ) 
 REPRESENTATION_ITEM ( '' )  );
#26423 = DIRECTION ( 'NONE',  ( 1.000000000000000000, 0.000000000000000000, 0.000000000000000000 ) ) ;
#26424 = CARTESIAN_POINT ( 'NONE',  ( 21.09992658989238734, 38.56284415653841791, 47.04930799450051637 ) ) ;
#26425 = EDGE_CURVE ( 'NONE', #19411, #18170, #17228, .T. ) ;
#26426 = ORIENTED_EDGE ( 'NONE', *, *, #1110, .T. ) ;
#26427 = DIRECTION ( 'NONE',  ( 0.000000000000000000, 0.000000000000000000, 1.000000000000000000 ) ) ;
#26428 = ORIENTED_EDGE ( 'NONE', *, *, #18551, .T. ) ;
#26429 = CIRCLE ( 'NONE', #12295, 12.27641737965286772 ) ;
#26430 = DIRECTION ( 'NONE',  ( 0.000000000000000000, 0.000000000000000000, 1.000000000000000000 ) ) ;
#26431 = CARTESIAN_POINT ( 'NONE',  ( 21.09992658989239089, 28.59184655352419213, 47.04930799450051637 ) ) ;
#26432 = DIRECTION ( 'NONE',  ( -1.224646799147353207E-16, -1.349345573449484691E-32, 1.000000000000000000 ) ) ;
#26433 = SHAPE_REPRESENTATION_RELATIONSHIP ( 'NONE' , 'NONE' ,  #14743, #12811 ) ;
#26434 = VERTEX_POINT ( 'NONE', #27243 ) ;
#26435 = EDGE_LOOP ( 'NONE', ( #25836, #16728, #26906, #18981 ) ) ;
#26436 = DIRECTION ( 'NONE',  ( 0.2756373558169941118, -0.9612616959383204485, -1.315048337272770897E-17 ) ) ;
#26437 = CARTESIAN_POINT ( 'NONE',  ( 21.09992658989238734, 38.56284415653841791, 47.04930799450051637 ) ) ;
#26438 = PLANE ( 'NONE',  #6220 ) ;
#26439 = VERTEX_POINT ( 'NONE', #9367 ) ;
#26440 = DIRECTION ( 'NONE',  ( 0.000000000000000000, 0.000000000000000000, 1.000000000000000000 ) ) ;
#26441 = DIRECTION ( 'NONE',  ( -1.101824276508909887E-16, 1.000000000000000000, -0.000000000000000000 ) ) ;
#26442 = ORIENTED_EDGE ( 'NONE', *, *, #12500, .T. ) ;
#26443 = CARTESIAN_POINT ( 'NONE',  ( -40.50764110105879467, 7.565280838256598805, 60.25772877010867745 ) ) ;
#26444 = CARTESIAN_POINT ( 'NONE',  ( 45.46000861347822308, 28.17287913140503619, 49.57397645940629616 ) ) ;
#26445 = ADVANCED_FACE ( 'NONE', ( #6738 ), #11994, .F. ) ;
#26446 = CYLINDRICAL_SURFACE ( 'NONE', #24823, 12.62506659569710266 ) ;
#26447 = CIRCLE ( 'NONE', #18055, 56.65825807113184709 ) ;
#26448 = CIRCLE ( 'NONE', #16483, 0.1000000000000014905 ) ;
#26449 = EDGE_CURVE ( 'NONE', #8640, #32001, #6907, .T. ) ;
#26450 = CIRCLE ( 'NONE', #31705, 12.62506659569710266 ) ;
#26451 = ADVANCED_FACE ( 'NONE', ( #166 ), #12658, .F. ) ;
#26452 = CIRCLE ( 'NONE', #30668, 55.00000000000000000 ) ;
#26453 = AXIS2_PLACEMENT_3D ( 'NONE', #17867, #15406, #28528 ) ;
#26454 = ORIENTED_EDGE ( 'NONE', *, *, #11379, .T. ) ;
#26455 = DIRECTION ( 'NONE',  ( -0.5319835227803569877, -0.2110602665713105230, 0.8200287161831886218 ) ) ;
#26456 = DIRECTION ( 'NONE',  ( 0.000000000000000000, 0.000000000000000000, 1.000000000000000000 ) ) ;
#26457 = FACE_OUTER_BOUND ( 'NONE', #25637, .T. ) ;
#26458 = CARTESIAN_POINT ( 'NONE',  ( 48.40186567930498285, 28.91618040159426073, 45.03923535223908203 ) ) ;
#26459 = ORIENTED_EDGE ( 'NONE', *, *, #3221, .F. ) ;
#26460 = CARTESIAN_POINT ( 'NONE',  ( 33.46699938050303302, 38.56284415653841791, 47.04930799450051637 ) ) ;
#26461 = DIRECTION ( 'NONE',  ( -1.101824276508909887E-16, 1.000000000000000000, -0.000000000000000000 ) ) ;
#26462 = EDGE_CURVE ( 'NONE', #21567, #19469, #30368, .T. ) ;
#26463 = CARTESIAN_POINT ( 'NONE',  ( -40.76199410932685652, 8.110698076655891597, 54.59072935073782418 ) ) ;
#26464 = DIRECTION ( 'NONE',  ( -1.101824276508909887E-16, 1.000000000000000000, -0.000000000000000000 ) ) ;
#26465 = CARTESIAN_POINT ( 'NONE',  ( -40.51522877113607990, 7.610537050327680575, 53.90050461276381100 ) ) ;
#26466 = CARTESIAN_POINT ( 'NONE',  ( -40.11598084786749752, 7.671759737001393908, 53.80788663826320573 ) ) ;
#26467 = AXIS2_PLACEMENT_3D ( 'NONE', #2610, #22305, #22457 ) ;
#26468 = CARTESIAN_POINT ( 'NONE',  ( 45.96182992765471909, 25.20087065737812182, 44.82232689504102296 ) ) ;
#26469 = VECTOR ( 'NONE', #23161, 1000.000000000000000 ) ;
#26470 = ADVANCED_BREP_SHAPE_REPRESENTATION ( '', ( #12454, #8172 ), #9736 ) ;
#26471 = SURFACE_STYLE_USAGE ( .BOTH. , #23999 ) ;
#26472 = ORIENTED_EDGE ( 'NONE', *, *, #32315, .F. ) ;
#26473 = CARTESIAN_POINT ( 'NONE',  ( -40.59290754354907449, 7.518856927436786464, 53.97121855808759250 ) ) ;
#26474 = CARTESIAN_POINT ( 'NONE',  ( 45.79384627280941089, 29.17957786121581165, 49.05938063676249072 ) ) ;
#26475 = AXIS2_PLACEMENT_3D ( 'NONE', #30966, #11107, #28650 ) ;
#26476 = CARTESIAN_POINT ( 'NONE',  ( 21.09785597605720753, 13.86454579224779948, 47.04930799450052348 ) ) ;
#26477 = AXIS2_PLACEMENT_3D ( 'NONE', #10888, #20881, #28445 ) ;
#26478 = DIRECTION ( 'NONE',  ( -0.000000000000000000, -1.000000000000000000, 0.000000000000000000 ) ) ;
#26479 = ORIENTED_EDGE ( 'NONE', *, *, #12241, .T. ) ;
#26480 = CARTESIAN_POINT ( 'NONE',  ( -39.53252429583445604, -5.935481122642606522, 77.87649032733463628 ) ) ;
#26481 = CARTESIAN_POINT ( 'NONE',  ( -40.18117225532236603, 7.056010640735439488, 39.15497037975539740 ) ) ;
#26482 = DIRECTION ( 'NONE',  ( -0.000000000000000000, -1.000000000000000000, 0.000000000000000000 ) ) ;
#26483 = EDGE_CURVE ( 'NONE', #29567, #26975, #11455, .T. ) ;
#26484 = ORIENTED_EDGE ( 'NONE', *, *, #29684, .T. ) ;
#26485 = CARTESIAN_POINT ( 'NONE',  ( 21.09785597605720753, 14.99513937955032716, 47.04930799450052348 ) ) ;
#26486 = DIRECTION ( 'NONE',  ( 0.1949050434465282311, -0.6797146636928673713, -0.7071067811865467956 ) ) ;
#26487 = B_SPLINE_CURVE_WITH_KNOTS ( 'NONE', 3,
 ( #31732, #16939, #22193, #29592, #9242, #26802, #31887, #9404, #19405, #26957, #4480, #7104, #14499, #27123, #24492, #17102, #14660, #24666, #2183, #32224, #13613, #8524, #7928, #12529, #2825, #17600, #12854, #22846, #20986, #17924, #31014, #359, #27612, #3588, #6064, #26068, #24993, #27942, #15308, #10067, #23618, #10382, #18516, #7756 ),
 .UNSPECIFIED., .F., .F.,
 ( 4, 2, 2, 2, 2, 2, 2, 2, 2, 2, 2, 2, 2, 2, 2, 2, 2, 2, 2, 2, 2, 4 ),
 ( 0.000000000000000000, 0.001748345063742785897, 0.003496690127485571793, 0.005245035191228358123, 0.006119207723099748253, 0.006993380254971139250, 0.008741725318713916906, 0.01049007038245669370, 0.01223841544619947048, 0.01398676050994224727, 0.01573510557368502233, 0.01748345063742779912, 0.01923179570117057244, 0.02010596823304195563, 0.02098014076491334229, 0.02272848582865609826, 0.02360265836052748145, 0.02447683089239886464, 0.02535100342427025130, 0.02622517595614163102, 0.02709934848801301768, 0.02797352101988440087 ),
 .UNSPECIFIED. ) ;
#26488 = DIRECTION ( 'NONE',  ( 1.000000000000000000, 0.000000000000000000, 0.000000000000000000 ) ) ;
#26489 = ADVANCED_FACE ( 'NONE', ( #22321 ), #22961, .F. ) ;
#26490 = FACE_OUTER_BOUND ( 'NONE', #9889, .T. ) ;
#26491 = VERTEX_POINT ( 'NONE', #30536 ) ;
#26492 = CARTESIAN_POINT ( 'NONE',  ( 72.46310410352296572, 9.702389020015065313, 20.34850893876554778 ) ) ;
#26493 = ORIENTED_EDGE ( 'NONE', *, *, #23838, .F. ) ;
#26494 = EDGE_CURVE ( 'NONE', #18267, #22755, #17717, .T. ) ;
#26495 = ORIENTED_EDGE ( 'NONE', *, *, #27239, .F. ) ;
#26496 = ADVANCED_FACE ( 'NONE', ( #28067 ), #15267, .F. ) ;
#26497 = AXIS2_PLACEMENT_3D ( 'NONE', #12527, #22513, #46 ) ;
#26498 =( GEOMETRIC_REPRESENTATION_CONTEXT ( 3 ) GLOBAL_UNCERTAINTY_ASSIGNED_CONTEXT ( ( #1251 ) ) GLOBAL_UNIT_ASSIGNED_CONTEXT ( ( #14331, #19226, #4801 ) ) REPRESENTATION_CONTEXT ( 'NONE', 'WORKASPACE' ) );
#26499 = CIRCLE ( 'NONE', #24339, 84.30000000000001137 ) ;
#26500 = DIRECTION ( 'NONE',  ( 0.000000000000000000, 0.000000000000000000, 1.000000000000000000 ) ) ;
#26501 = CARTESIAN_POINT ( 'NONE',  ( 21.09992658989239089, 25.84143805560860940, 47.04930799450051637 ) ) ;
#26502 = CARTESIAN_POINT ( 'NONE',  ( 81.78746918506877250, -5.936918610400974572, 77.96063504348295226 ) ) ;
#26503 = TOROIDAL_SURFACE ( 'NONE', #27023, 12.40141737965282509, 0.1249999999999980849 ) ;
#26504 = ORIENTED_EDGE ( 'NONE', *, *, #25455, .F. ) ;
#26505 = CARTESIAN_POINT ( 'NONE',  ( 21.09785597605720753, -13.59284023713420630, 102.7732403313682994 ) ) ;
#26506 = EDGE_LOOP ( 'NONE', ( #24735, #20001, #29278, #2875 ) ) ;
#26507 = CARTESIAN_POINT ( 'NONE',  ( -43.38408989745150990, 1.111547985471240674, 53.64930799450051779 ) ) ;
#26508 = CARTESIAN_POINT ( 'NONE',  ( 0.1399989214664148496, 11.92558985988973852, 98.82976274952495999 ) ) ;
#26509 = ORIENTED_EDGE ( 'NONE', *, *, #29543, .F. ) ;
#26510 = CARTESIAN_POINT ( 'NONE',  ( -24.83466114100572852, 14.61319044934410627, 47.04930799450052348 ) ) ;
#26511 = LINE ( 'NONE', #28976, #21552 ) ;
#26512 = CARTESIAN_POINT ( 'NONE',  ( 21.09785597605720753, -13.59284023713420630, 102.6732403313682909 ) ) ;
#26513 = CARTESIAN_POINT ( 'NONE',  ( 21.09785597605720753, 17.16474120167318063, 47.04930799450052348 ) ) ;
#26514 = B_SPLINE_CURVE_WITH_KNOTS ( 'NONE', 3,
 ( #18571, #16755, #16594, #23986, #1669, #4296, #1500, #11516 ),
 .UNSPECIFIED., .F., .F.,
 ( 4, 2, 2, 4 ),
 ( 0.000000000000000000, 0.0005357332384296896628, 0.0008035998576445335185, 0.001071466476859377374 ),
 .UNSPECIFIED. ) ;
#26515 = ORIENTED_EDGE ( 'NONE', *, *, #28610, .F. ) ;
#26516 = CARTESIAN_POINT ( 'NONE',  ( 21.09992658989238734, 38.56284415653841791, 47.04930799450051637 ) ) ;
#26517 = DIRECTION ( 'NONE',  ( 0.000000000000000000, 1.000000000000000000, 0.000000000000000000 ) ) ;
#26518 = LINE ( 'NONE', #31289, #1064 ) ;
#26519 = DIRECTION ( 'NONE',  ( 0.000000000000000000, 0.000000000000000000, -1.000000000000000000 ) ) ;
#26520 = CYLINDRICAL_SURFACE ( 'NONE', #22575, 12.36707279061065101 ) ;
#26521 = ORIENTED_EDGE ( 'NONE', *, *, #29076, .F. ) ;
#26522 = CARTESIAN_POINT ( 'NONE',  ( 50.59785597605720397, 14.86454579224779948, 47.04930799450051637 ) ) ;
#26523 = LINE ( 'NONE', #21750, #740 ) ;
#26524 = EDGE_CURVE ( 'NONE', #22685, #20447, #24802, .T. ) ;
#26525 = ORIENTED_EDGE ( 'NONE', *, *, #8803, .F. ) ;
#26526 = DIRECTION ( 'NONE',  ( 0.000000000000000000, -0.7071067811865474617, -0.7071067811865474617 ) ) ;
#26527 = CIRCLE ( 'NONE', #21803, 13.50178401536290984 ) ;
#26528 = PRODUCT_DEFINITION_FORMATION_WITH_SPECIFIED_SOURCE ( 'ANY', '', #7490, .NOT_KNOWN. ) ;
#26529 = EDGE_CURVE ( 'NONE', #756, #12577, #2515, .T. ) ;
#26530 = DIRECTION ( 'NONE',  ( -1.101824276508909887E-16, 1.000000000000000000, -0.000000000000000000 ) ) ;
#26531 = VERTEX_POINT ( 'NONE', #22475 ) ;
#26532 = EDGE_LOOP ( 'NONE', ( #15102, #1528, #29060, #5297 ) ) ;
#26533 = EDGE_CURVE ( 'NONE', #21772, #19940, #9266, .T. ) ;
#26534 = VECTOR ( 'NONE', #17293, 1000.000000000000114 ) ;
#26535 = ORIENTED_EDGE ( 'NONE', *, *, #1296, .F. ) ;
#26536 = FACE_OUTER_BOUND ( 'NONE', #1010, .T. ) ;
#26537 = CIRCLE ( 'NONE', #9784, 12.62506659569710266 ) ;
#26538 = PRODUCT_DEFINITION_FORMATION_WITH_SPECIFIED_SOURCE ( 'ANY', '', #20053, .NOT_KNOWN. ) ;
#26539 = ORIENTED_EDGE ( 'NONE', *, *, #25170, .F. ) ;
#26540 = DIRECTION ( 'NONE',  ( -0.000000000000000000, -1.000000000000000000, 0.000000000000000000 ) ) ;
#26541 = DIRECTION ( 'NONE',  ( 1.000000000000000000, 0.000000000000000000, -1.110223024625154963E-14 ) ) ;
#26542 = CARTESIAN_POINT ( 'NONE',  ( 21.09785597605719332, 40.06454579224778456, 35.04930799450050927 ) ) ;
#26543 = FACE_OUTER_BOUND ( 'NONE', #29873, .T. ) ;
#26544 = CARTESIAN_POINT ( 'NONE',  ( 46.02876340639226527, 27.61119643316632022, 44.95353858666495483 ) ) ;
#26545 = VERTEX_POINT ( 'NONE', #12491 ) ;
#26546 = ORIENTED_EDGE ( 'NONE', *, *, #28875, .T. ) ;
#26547 = CARTESIAN_POINT ( 'NONE',  ( -10.26669494407825134, -5.913508961333113767, -10.73378008532072414 ) ) ;
#26548 = EDGE_LOOP ( 'NONE', ( #25922, #7037, #28188, #11770 ) ) ;
#26549 = DIRECTION ( 'NONE',  ( -1.101824276508909887E-16, 1.000000000000000000, -0.000000000000000000 ) ) ;
#26550 = CARTESIAN_POINT ( 'NONE',  ( 8.732853799281729223, 26.72145308207318948, 47.04930799450051637 ) ) ;
#26551 = TOROIDAL_SURFACE ( 'NONE', #10325, 12.61792373059898331, 0.1249999999999965583 ) ;
#26552 = DIRECTION ( 'NONE',  ( -1.000000000000000000, 0.000000000000000000, 0.000000000000000000 ) ) ;
#26553 = CARTESIAN_POINT ( 'NONE',  ( -18.40214402394278892, 13.86454579224779948, 47.04930799450052348 ) ) ;
#26554 = FACE_OUTER_BOUND ( 'NONE', #20225, .T. ) ;
#26555 = CARTESIAN_POINT ( 'NONE',  ( 46.96268396749378127, 25.43121246473837971, 49.65201805493727960 ) ) ;
#26556 = DIRECTION ( 'NONE',  ( 0.000000000000000000, 0.000000000000000000, -1.000000000000000000 ) ) ;
#26557 = CARTESIAN_POINT ( 'NONE',  ( 33.37634396954523908, 27.09164230456639899, 47.04930799450051637 ) ) ;
#26558 = ORIENTED_EDGE ( 'NONE', *, *, #12061, .T. ) ;
#26559 = FACE_OUTER_BOUND ( 'NONE', #23333, .T. ) ;
#26560 = CARTESIAN_POINT ( 'NONE',  ( 21.09992658989239089, 29.71664230456640254, 47.04930799450051637 ) ) ;
#26561 = CARTESIAN_POINT ( 'NONE',  ( 8.732853799281732776, 28.47145308207318237, 47.04930799450051637 ) ) ;
#26562 = CARTESIAN_POINT ( 'NONE',  ( 48.81241343884743600, 22.91413368675619111, 46.49136847324655974 ) ) ;
#26563 = CARTESIAN_POINT ( 'NONE',  ( 49.98072202819531640, 25.54488759933319386, 47.19902993264913960 ) ) ;
#26564 = ORIENTED_EDGE ( 'NONE', *, *, #30357, .T. ) ;
#26565 = CARTESIAN_POINT ( 'NONE',  ( -25.57662701300441555, 13.66454579224780019, 47.04930799450052348 ) ) ;
#26566 = EDGE_LOOP ( 'NONE', ( #15028, #6969, #17992, #19990, #26864, #24570, #29322, #8514, #3647, #30317, #9471, #26845, #4565, #18203, #20278, #31005, #30514, #18387, #18500, #16999, #19827, #10491 ) ) ;
#26567 = DIRECTION ( 'NONE',  ( -1.101824276508909887E-16, 1.000000000000000000, -0.000000000000000000 ) ) ;
#26568 = CIRCLE ( 'NONE', #1397, 12.62506659569710266 ) ;
#26569 = EDGE_CURVE ( 'NONE', #11074, #28974, #30823, .T. ) ;
#26570 = ORIENTED_EDGE ( 'NONE', *, *, #8030, .F. ) ;
#26571 = ADVANCED_FACE ( 'NONE', ( #5580 ), #9844, .T. ) ;
#26572 = EDGE_CURVE ( 'NONE', #27727, #27500, #10025, .T. ) ;
#26573 = ADVANCED_FACE ( 'NONE', ( #14946 ), #31333, .T. ) ;
#26574 = ORIENTED_EDGE ( 'NONE', *, *, #28617, .F. ) ;
#26575 = DIRECTION ( 'NONE',  ( -0.000000000000000000, -1.000000000000000000, 0.000000000000000000 ) ) ;
#26576 = LINE ( 'NONE', #4086, #17611 ) ;
#26577 = DIRECTION ( 'NONE',  ( 1.000000000000000000, 0.000000000000000000, 0.000000000000000000 ) ) ;
#26578 = EDGE_LOOP ( 'NONE', ( #14182, #5161, #23057, #10815 ) ) ;
#26579 = CARTESIAN_POINT ( 'NONE',  ( 21.09992658989239089, 25.97145308207318593, 47.04930799450051637 ) ) ;
#26580 = LINE ( 'NONE', #4266, #18582 ) ;
#26581 = CARTESIAN_POINT ( 'NONE',  ( -40.01416947921579492, 7.179266651195999493, 38.85693688870069451 ) ) ;
#26582 = AXIS2_PLACEMENT_3D ( 'NONE', #13657, #6099, #3634 ) ;
#26583 = EDGE_LOOP ( 'NONE', ( #7325, #27824, #27268, #17129 ) ) ;
#26584 = DIRECTION ( 'NONE',  ( -0.4848096202463655358, -0.8746197071393799760, 0.000000000000000000 ) ) ;
#26585 = ORIENTED_EDGE ( 'NONE', *, *, #17656, .F. ) ;
#26586 = DIRECTION ( 'NONE',  ( 0.000000000000000000, -1.000000000000000000, 0.000000000000000000 ) ) ;
#26587 = DIRECTION ( 'NONE',  ( -0.8907924397839086517, -1.100109291107993817E-16, 0.4544104193609908027 ) ) ;
#26588 = PRODUCT_DEFINITION_SHAPE ( 'NONE', 'NONE',  #8108 ) ;
#26589 = AXIS2_PLACEMENT_3D ( 'NONE', #3177, #8278, #22555 ) ;
#26590 = DIRECTION ( 'NONE',  ( -0.000000000000000000, -1.000000000000000000, -0.000000000000000000 ) ) ;
#26591 = ORIENTED_EDGE ( 'NONE', *, *, #29233, .T. ) ;
#26592 = ORIENTED_EDGE ( 'NONE', *, *, #7125, .F. ) ;
#26593 = EDGE_CURVE ( 'NONE', #8390, #14305, #7294, .T. ) ;
#26594 = CARTESIAN_POINT ( 'NONE',  ( -39.59300248568538194, 7.744584186742828891, 61.94930799450052206 ) ) ;
#26595 = LINE ( 'NONE', #9039, #18766 ) ;
#26596 = LINE ( 'NONE', #23659, #20356 ) ;
#26597 = ORIENTED_EDGE ( 'NONE', *, *, #7159, .T. ) ;
#26598 = CARTESIAN_POINT ( 'NONE',  ( 21.09992658989239089, 27.59164230456639544, 47.04930799450051637 ) ) ;
#26599 = DIRECTION ( 'NONE',  ( -1.000000000000000000, 0.000000000000000000, 0.000000000000000000 ) ) ;
#26600 = ORIENTED_EDGE ( 'NONE', *, *, #21617, .T. ) ;
#26601 = CARTESIAN_POINT ( 'NONE',  ( 33.72499318558949710, 30.59143805560860585, 47.04930799450051637 ) ) ;
#26602 = DIRECTION ( 'NONE',  ( -1.000000000000000000, 0.000000000000000000, 0.000000000000000000 ) ) ;
#26603 = EDGE_CURVE ( 'NONE', #10451, #22848, #1446, .T. ) ;
#26604 = ADVANCED_FACE ( 'NONE', ( #13460 ), #31332, .F. ) ;
#26605 = ADVANCED_FACE ( 'NONE', ( #23458 ), #19787, .T. ) ;
#26606 = ADVANCED_FACE ( 'NONE', ( #23135, #26241 ), #28388, .F. ) ;
#26608 = ADVANCED_FACE ( 'NONE', ( #28552 ), #28195, .T. ) ;
#26607 = CIRCLE ( 'NONE', #24518, 12.27848799348799069 ) ;
#26609 = CIRCLE ( 'NONE', #11920, 32.50000000000000000 ) ;
#26610 = ORIENTED_EDGE ( 'NONE', *, *, #30543, .T. ) ;
#26611 = CIRCLE ( 'NONE', #29237, 39.49999999999999289 ) ;
#26612 = DIRECTION ( 'NONE',  ( -1.101824276508909887E-16, 1.000000000000000000, -0.000000000000000000 ) ) ;
#26613 = LINE ( 'NONE', #1990, #11766 ) ;
#26614 = DIRECTION ( 'NONE',  ( 0.000000000000000000, 0.000000000000000000, -1.000000000000000000 ) ) ;
#26615 = CARTESIAN_POINT ( 'NONE',  ( 48.94625023931840246, 29.55784706826092645, 46.10640627770150246 ) ) ;
#26616 = AXIS2_PLACEMENT_3D ( 'NONE', #6967, #16963, #14851 ) ;
#26617 = VERTEX_POINT ( 'NONE', #11310 ) ;
#26618 = CARTESIAN_POINT ( 'NONE',  ( -40.70484894842233103, 8.274204744976163539, 54.44930799450051495 ) ) ;
#26619 = DIRECTION ( 'NONE',  ( -1.000000000000000000, 0.000000000000000000, 0.000000000000000000 ) ) ;
#26620 = CARTESIAN_POINT ( 'NONE',  ( 54.71524953585419127, -1.428409478025996160, -6.539106349574636212 ) ) ;
#26621 = CARTESIAN_POINT ( 'NONE',  ( 46.96819297411687444, 26.76988759933318818, 49.54594323136014822 ) ) ;
#26622 = CARTESIAN_POINT ( 'NONE',  ( 21.09785597605719332, -15.93545420775219945, 47.04930799450051637 ) ) ;
#26623 = CARTESIAN_POINT ( 'NONE',  ( 17.28711060612849337, -13.74047052604243824, -11.17459240441506019 ) ) ;
#26624 = DIRECTION ( 'NONE',  ( 0.7549115352271290602, -0.6546536707079775308, 0.03920644602090544995 ) ) ;
#26625 = FACE_OUTER_BOUND ( 'NONE', #15055, .T. ) ;
#26626 = VERTEX_POINT ( 'NONE', #25757 ) ;
#26627 = EDGE_CURVE ( 'NONE', #25250, #19596, #12993, .T. ) ;
#26628 = DIRECTION ( 'NONE',  ( 0.000000000000000000, -0.000000000000000000, -1.000000000000000000 ) ) ;
#26630 = CARTESIAN_POINT ( 'NONE',  ( 45.35708200440645044, 26.20457786121582444, 45.92000246470680480 ) ) ;
#26629 = CIRCLE ( 'NONE', #446, 4.100000000000001421 ) ;
#26631 = EDGE_CURVE ( 'NONE', #31093, #25031, #3590, .T. ) ;
#26632 = AXIS2_PLACEMENT_3D ( 'NONE', #16671, #16841, #13914 ) ;
#26633 = CARTESIAN_POINT ( 'NONE',  ( 45.60118599681192109, 25.28986642951281638, 49.35635783644741537 ) ) ;
#26634 = CARTESIAN_POINT ( 'NONE',  ( -43.69495677161796010, 1.169528900831203311, 60.54930799450051637 ) ) ;
#26635 = AXIS2_PLACEMENT_3D ( 'NONE', #9737, #12367, #1685 ) ;
#26636 = ORIENTED_EDGE ( 'NONE', *, *, #22403, .T. ) ;
#26637 = CARTESIAN_POINT ( 'NONE',  ( 21.09785597605719332, 40.56454579224779877, 79.54930799450052348 ) ) ;
#26638 = CARTESIAN_POINT ( 'NONE',  ( 21.09785597605719332, 13.74476430820393347, 103.0493079945005093 ) ) ;
#26639 = DIRECTION ( 'NONE',  ( -0.000000000000000000, -1.000000000000000000, 0.000000000000000000 ) ) ;
#26640 = VECTOR ( 'NONE', #11754, 1000.000000000000000 ) ;
#26641 = ORIENTED_EDGE ( 'NONE', *, *, #25850, .F. ) ;
#26642 = FACE_OUTER_BOUND ( 'NONE', #11392, .T. ) ;
#26643 = CARTESIAN_POINT ( 'NONE',  ( -38.32955388700093380, 6.929907785659375818, 32.14930799450051779 ) ) ;
#26644 = DIRECTION ( 'NONE',  ( -2.946248497964555786E-19, -3.001156285468303092E-19, -1.000000000000000000 ) ) ;
#26645 = AXIS2_PLACEMENT_3D ( 'NONE', #1836, #29088, #1347 ) ;
#26646 = CARTESIAN_POINT ( 'NONE',  ( 46.61910388458303345, 22.93328494799376216, 45.39920705986084215 ) ) ;
#26647 = EDGE_LOOP ( 'NONE', ( #11393, #29509, #16538, #27163 ) ) ;
#26648 = CARTESIAN_POINT ( 'NONE',  ( -40.60922101150776342, 7.585765375989710790, 60.19601566531913051 ) ) ;
#26649 = ORIENTED_EDGE ( 'NONE', *, *, #329, .F. ) ;
#26650 = EDGE_CURVE ( 'NONE', #17679, #30342, #27197, .T. ) ;
#26651 = ORIENTED_EDGE ( 'NONE', *, *, #14390, .T. ) ;
#26652 = CARTESIAN_POINT ( 'NONE',  ( 21.09992658989238734, 32.21664230456639899, 47.04930799450051637 ) ) ;
#26653 = VECTOR ( 'NONE', #19197, 1000.000000000000000 ) ;
#26654 = AXIS2_PLACEMENT_3D ( 'NONE', #11911, #14543, #12572 ) ;
#26655 = ADVANCED_FACE ( 'NONE', ( #23771 ), #11154, .T. ) ;
#26656 = CARTESIAN_POINT ( 'NONE',  ( -31.14390254341316577, 1.751253714874866141, 79.49571236864932189 ) ) ;
#26657 = FACE_OUTER_BOUND ( 'NONE', #26999, .T. ) ;
#26658 = EDGE_CURVE ( 'NONE', #1564, #28978, #21341, .T. ) ;
#26659 = ORIENTED_EDGE ( 'NONE', *, *, #3709, .T. ) ;
#26660 = AXIS2_PLACEMENT_3D ( 'NONE', #6258, #31053, #6420 ) ;
#26661 = CARTESIAN_POINT ( 'NONE',  ( 52.07878664889356912, -5.935345006353229813, -13.65255231306078798 ) ) ;
#26662 = EDGE_LOOP ( 'NONE', ( #19889, #16118, #32316, #28771 ) ) ;
#26663 = CYLINDRICAL_SURFACE ( 'NONE', #2601, 31.50000000000000000 ) ;
#26664 = DIRECTION ( 'NONE',  ( -1.101824276508909887E-16, 1.000000000000000000, -0.000000000000000000 ) ) ;
#26665 = CARTESIAN_POINT ( 'NONE',  ( 21.09785597605719332, 11.92558985988973497, 47.04930799450051637 ) ) ;
#26666 = ORIENTED_EDGE ( 'NONE', *, *, #1320, .F. ) ;
#26667 = EDGE_CURVE ( 'NONE', #18606, #21751, #28766, .T. ) ;
#26668 = DIRECTION ( 'NONE',  ( 0.8746197071393926326, -0.4848096202463430537, -8.676864087101709653E-18 ) ) ;
#26669 = CARTESIAN_POINT ( 'NONE',  ( 8.732853799281738105, 30.21183152705961561, 47.04930799450051637 ) ) ;
#26670 = CARTESIAN_POINT ( 'NONE',  ( -41.02113223168485234, 7.230835263863472306, 39.54930799450052348 ) ) ;
#26671 = EDGE_CURVE ( 'NONE', #3483, #154, #22407, .T. ) ;
#26672 = ORIENTED_EDGE ( 'NONE', *, *, #14233, .F. ) ;
#26673 = CARTESIAN_POINT ( 'NONE',  ( 8.698509210239587119, 32.34164230456639899, 47.04930799450051637 ) ) ;
#26674 = CARTESIAN_POINT ( 'NONE',  ( 21.09785597605719332, 11.78014697381582643, 47.04930799450051637 ) ) ;
#26675 = CARTESIAN_POINT ( 'NONE',  ( -48.24907229644473716, 10.92050229712533316, 54.54930799450051637 ) ) ;
#26676 = CARTESIAN_POINT ( 'NONE',  ( 21.09785597605719332, -5.935454207752083988, 47.04930799450039558 ) ) ;
#26677 = EDGE_CURVE ( 'NONE', #17732, #27591, #4663, .T. ) ;
#26678 =( LENGTH_UNIT ( ) NAMED_UNIT ( * ) SI_UNIT ( .MILLI., .METRE. ) );
#26679 = ORIENTED_EDGE ( 'NONE', *, *, #16879, .T. ) ;
#26680 = CARTESIAN_POINT ( 'NONE',  ( -40.01678386995647685, 7.136726190597861397, 35.21344202038847726 ) ) ;
#26681 = DIRECTION ( 'NONE',  ( 0.2756373558169932236, -0.9612616959383205595, 1.479773560108267395E-16 ) ) ;
#26682 = EDGE_LOOP ( 'NONE', ( #3068, #9824, #30264, #24696 ) ) ;
#26683 = CYLINDRICAL_SURFACE ( 'NONE', #1495, 2.499999999999997335 ) ;
#26684 = AXIS2_PLACEMENT_3D ( 'NONE', #8508, #20810, #10662 ) ;
#26685 = AXIS2_PLACEMENT_3D ( 'NONE', #6555, #11806, #19333 ) ;
#26686 = LINE ( 'NONE', #31619, #32141 ) ;
#26687 = ORIENTED_EDGE ( 'NONE', *, *, #29691, .T. ) ;
#26688 = ORIENTED_EDGE ( 'NONE', *, *, #10733, .F. ) ;
#26689 = EDGE_CURVE ( 'NONE', #3106, #21227, #18798, .T. ) ;
#26690 = AXIS2_PLACEMENT_3D ( 'NONE', #25596, #13139, #15748 ) ;
#26691 = EDGE_LOOP ( 'NONE', ( #18666, #10885, #2986, #24960 ) ) ;
#26692 = EDGE_CURVE ( 'NONE', #18982, #7619, #3013, .T. ) ;
#26693 = CARTESIAN_POINT ( 'NONE',  ( 21.09785597605719332, 7.881678200673687407, 27.79103836896735302 ) ) ;
#26694 = AXIS2_PLACEMENT_3D ( 'NONE', #16010, #8630, #3695 ) ;
#26695 = AXIS2_PLACEMENT_3D ( 'NONE', #21712, #14509, #11877 ) ;
#26696 = EDGE_CURVE ( 'NONE', #20780, #20710, #7216, .T. ) ;
#26697 = ORIENTED_EDGE ( 'NONE', *, *, #19661, .T. ) ;
#26698 = CARTESIAN_POINT ( 'NONE',  ( 21.09785597605719332, 30.56454579224779522, 47.04930799450051637 ) ) ;
#26699 = DIRECTION ( 'NONE',  ( 1.000000000000000000, 0.000000000000000000, 1.224646799147353207E-16 ) ) ;
#26700 = FACE_OUTER_BOUND ( 'NONE', #7147, .T. ) ;
#26701 = CARTESIAN_POINT ( 'NONE',  ( -40.50755597040444655, 7.564707434449536194, 53.84113122998387979 ) ) ;
#26702 = CARTESIAN_POINT ( 'NONE',  ( 46.02876340639226527, 29.71119643316631809, 44.95353858666495483 ) ) ;
#26703 = ORIENTED_EDGE ( 'NONE', *, *, #16298, .T. ) ;
#26704 = CARTESIAN_POINT ( 'NONE',  ( -40.52510752649232728, 7.677764709599123272, 39.54930799450052348 ) ) ;
#26705 = VERTEX_POINT ( 'NONE', #969 ) ;
#26706 = DIRECTION ( 'NONE',  ( -0.4441739386572048920, 0.2110602665713095516, -0.8707256032141200697 ) ) ;
#26707 = ADVANCED_FACE ( 'NONE', ( #10993 ), #28700, .T. ) ;
#26708 = VERTEX_POINT ( 'NONE', #9658 ) ;
#26709 = CARTESIAN_POINT ( 'NONE',  ( -44.16105795751995799, -3.935454207752190126, 42.04930799450051637 ) ) ;
#26710 = FACE_OUTER_BOUND ( 'NONE', #27404, .T. ) ;
#26711 = AXIS2_PLACEMENT_3D ( 'NONE', #15313, #4812, #14834 ) ;
#26712 = AXIS2_PLACEMENT_3D ( 'NONE', #8609, #16142, #20594 ) ;
#26713 = CARTESIAN_POINT ( 'NONE',  ( -42.03703168893574116, 3.954238390689462257, 48.34930799450052064 ) ) ;
#26714 = CARTESIAN_POINT ( 'NONE',  ( -40.68496126738414631, 6.805971067583988621, 39.32862205504143560 ) ) ;
#26715 = CARTESIAN_POINT ( 'NONE',  ( -40.51522948349269626, 7.610540244934343335, 60.19810810903209131 ) ) ;
#26716 = EDGE_CURVE ( 'NONE', #24189, #31962, #21421, .T. ) ;
#26717 = CARTESIAN_POINT ( 'NONE',  ( 47.23302798462060537, 27.18121246473837616, 44.44659793406428605 ) ) ;
#26718 = AXIS2_PLACEMENT_3D ( 'NONE', #2917, #22932, #20307 ) ;
#26719 = CARTESIAN_POINT ( 'NONE',  ( 47.45197874502928670, 22.98879437201065912, 48.47452853850663246 ) ) ;
#26720 = CARTESIAN_POINT ( 'NONE',  ( 21.09785597605720753, 13.86454579224779948, 47.04930799450052348 ) ) ;
#26721 = EDGE_LOOP ( 'NONE', ( #1176, #17162, #4415, #18174 ) ) ;
#26722 = DIRECTION ( 'NONE',  ( 0.000000000000000000, 0.000000000000000000, 1.000000000000000000 ) ) ;
#26723 = CIRCLE ( 'NONE', #31438, 12.50967055512594150 ) ;
#26724 = DIRECTION ( 'NONE',  ( -0.2756373558169974980, 0.9612616959383194493, 1.315048337272770743E-17 ) ) ;
#26725 = DIRECTION ( 'NONE',  ( -0.9612616959383206705, -0.2756373558169931681, 1.660411357259282445E-16 ) ) ;
#26726 = CARTESIAN_POINT ( 'NONE',  ( 48.15243707092404435, 22.93807716476589675, 45.72078620869762489 ) ) ;
#26727 = PLANE ( 'NONE',  #29316 ) ;
#26728 = VERTEX_POINT ( 'NONE', #14262 ) ;
#26729 = LINE ( 'NONE', #9175, #3556 ) ;
#26730 = ORIENTED_EDGE ( 'NONE', *, *, #9003, .T. ) ;
#26731 = DIRECTION ( 'NONE',  ( -1.101824276508909887E-16, 1.000000000000000000, -0.000000000000000000 ) ) ;
#26732 = DIRECTION ( 'NONE',  ( -1.000000000000000000, -1.101824276508909887E-16, 0.000000000000000000 ) ) ;
#26733 = CIRCLE ( 'NONE', #30938, 1.000000000000000888 ) ;
#26734 = CIRCLE ( 'NONE', #17284, 12.62506659569710266 ) ;
#26735 = EDGE_LOOP ( 'NONE', ( #25598, #5872, #7766, #29723 ) ) ;
#26736 = AXIS2_PLACEMENT_3D ( 'NONE', #13129, #23126, #643 ) ;
#26737 = VECTOR ( 'NONE', #4986, 1000.000000000000227 ) ;
#26738 = AXIS2_PLACEMENT_3D ( 'NONE', #20736, #1189, #1351 ) ;
#26739 = ORIENTED_EDGE ( 'NONE', *, *, #29684, .F. ) ;
#26740 = CIRCLE ( 'NONE', #9983, 12.62506659569710266 ) ;
#26741 = DIRECTION ( 'NONE',  ( 0.000000000000000000, -1.000000000000000000, 0.000000000000000000 ) ) ;
#26742 = AXIS2_PLACEMENT_3D ( 'NONE', #17445, #22364, #12538 ) ;
#26743 = DIRECTION ( 'NONE',  ( 0.000000000000000000, 0.000000000000000000, 1.000000000000000000 ) ) ;
#26744 = FACE_OUTER_BOUND ( 'NONE', #6839, .T. ) ;
#26745 = ORIENTED_EDGE ( 'NONE', *, *, #23110, .T. ) ;
#26746 = CARTESIAN_POINT ( 'NONE',  ( 21.09992658989239089, 28.09164230456639544, 47.04930799450051637 ) ) ;
#26747 = DIRECTION ( 'NONE',  ( -1.101824276508909887E-16, 1.000000000000000000, -0.000000000000000000 ) ) ;
#26748 = CARTESIAN_POINT ( 'NONE',  ( -42.38351229602917414, 14.72295342448899014, 55.13902476097742777 ) ) ;
#26749 = B_SPLINE_CURVE_WITH_KNOTS ( 'NONE', 3,
 ( #991, #5927, #8706, #3613 ),
 .UNSPECIFIED., .F., .F.,
 ( 4, 4 ),
 ( 0.000000000000000000, 1.000000000000000000 ),
 .UNSPECIFIED. ) ;
#26750 = EDGE_LOOP ( 'NONE', ( #29267, #12411, #2931, #12090 ) ) ;
#26751 = DIRECTION ( 'NONE',  ( 0.000000000000000000, 0.000000000000000000, 1.000000000000000000 ) ) ;
#26752 = AXIS2_PLACEMENT_3D ( 'NONE', #2175, #20051, #26952 ) ;
#26753 = ADVANCED_FACE ( 'NONE', ( #24094 ), #19653, .F. ) ;
#26754 = ORIENTED_EDGE ( 'NONE', *, *, #28861, .F. ) ;
#26755 = CARTESIAN_POINT ( 'NONE',  ( 21.09785597605720042, -17.03545420775220265, -31.35069200549948221 ) ) ;
#26756 = EDGE_CURVE ( 'NONE', #32254, #14591, #23006, .T. ) ;
#26757 = CARTESIAN_POINT ( 'NONE',  ( 21.09785597605719332, 40.56454579224780588, 34.54930799450048795 ) ) ;
#26758 = ORIENTED_EDGE ( 'NONE', *, *, #22972, .F. ) ;
#26759 = ORIENTED_EDGE ( 'NONE', *, *, #15204, .T. ) ;
#26760 = CARTESIAN_POINT ( 'NONE',  ( 69.53401346131808225, -13.30632128221581212, 19.07865907559169472 ) ) ;
#26761 = DIRECTION ( 'NONE',  ( 1.141485058121273114E-16, 2.056979540075764156E-16, 1.000000000000000000 ) ) ;
#26762 = AXIS2_PLACEMENT_3D ( 'NONE', #26674, #28981, #3871 ) ;
#26763 = CARTESIAN_POINT ( 'NONE',  ( 21.09785597605720397, -9.935454207752199451, -24.95069200549946586 ) ) ;
#26764 = EDGE_LOOP ( 'NONE', ( #10341, #5470, #31854, #20269 ) ) ;
#26765 = CARTESIAN_POINT ( 'NONE',  ( -12.44131731965827292, -3.812314126620122146, -9.074964031059534975 ) ) ;
#26766 = TOROIDAL_SURFACE ( 'NONE', #31990, 12.61792373059860850, 0.1249999999999999445 ) ;
#26767 = CARTESIAN_POINT ( 'NONE',  ( 73.43141673955737758, -13.74047052604243646, 72.85129969572992081 ) ) ;
#26768 = EDGE_LOOP ( 'NONE', ( #24875, #6072, #18889, #29800 ) ) ;
#26769 = DIRECTION ( 'NONE',  ( -0.000000000000000000, -1.000000000000000000, -0.000000000000000000 ) ) ;
#26770 = AXIS2_PLACEMENT_3D ( 'NONE', #27523, #30158, #4711 ) ;
#26771 = CARTESIAN_POINT ( 'NONE',  ( 45.46000861347822308, 25.37287913140504614, 49.57397645940629616 ) ) ;
#26772 = CONICAL_SURFACE ( 'NONE', #45, 30.00000000000000000, 0.5934119456780768687 ) ;
#26773 = CIRCLE ( 'NONE', #12634, 12.62506659569710266 ) ;
#26774 = DIRECTION ( 'NONE',  ( -1.101824276508909887E-16, 1.000000000000000000, -0.000000000000000000 ) ) ;
#26775 = AXIS2_PLACEMENT_3D ( 'NONE', #16532, #2088, #12116 ) ;
#26776 = ORIENTED_EDGE ( 'NONE', *, *, #19465, .T. ) ;
#26777 = CARTESIAN_POINT ( 'NONE',  ( -42.39006672483308336, 15.27003693862974032, 35.55750462089839203 ) ) ;
#26778 = CARTESIAN_POINT ( 'NONE',  ( -4.902144023942810236, 30.56454579224779522, 47.04930799450042400 ) ) ;
#26779 = DIRECTION ( 'NONE',  ( -1.224646799147353207E-16, -1.349345573449484691E-32, 1.000000000000000000 ) ) ;
#26780 = CARTESIAN_POINT ( 'NONE',  ( 45.28286642839709231, 24.98619643316632732, 47.97516931882780966 ) ) ;
#26781 = ORIENTED_EDGE ( 'NONE', *, *, #4819, .T. ) ;
#26782 = AXIS2_PLACEMENT_3D ( 'NONE', #29843, #2752, #8008 ) ;
#26783 = CARTESIAN_POINT ( 'NONE',  ( 47.09785597605719687, 15.77906836436399374, 47.04930799450078638 ) ) ;
#26784 = DIRECTION ( 'NONE',  ( 0.7141240004913198547, -0.3958453973320100738, 0.5773502691896283956 ) ) ;
#26785 = CIRCLE ( 'NONE', #24186, 1.100000000000001199 ) ;
#26786 = CARTESIAN_POINT ( 'NONE',  ( -40.60333149162104860, 7.557375771971046596, 60.08350751967648762 ) ) ;
#26787 = CIRCLE ( 'NONE', #24690, 55.96105416618080142 ) ;
#26788 = DIRECTION ( 'NONE',  ( -1.000000000000000000, -1.101824276508909887E-16, 0.000000000000000000 ) ) ;
#26789 = DIRECTION ( 'NONE',  ( -0.000000000000000000, -1.000000000000000000, -0.000000000000000000 ) ) ;
#26790 = ADVANCED_FACE ( 'NONE', ( #21793 ), #20309, .T. ) ;
#26791 = CYLINDRICAL_SURFACE ( 'NONE', #15798, 12.62506659569710266 ) ;
#26793 = EDGE_CURVE ( 'NONE', #1187, #26371, #2102, .T. ) ;
#26792 = DIRECTION ( 'NONE',  ( 0.000000000000000000, 0.000000000000000000, -1.000000000000000000 ) ) ;
#26794 = ADVANCED_FACE ( 'NONE', ( #17027 ), #21947, .F. ) ;
#26795 = EDGE_CURVE ( 'NONE', #25801, #20484, #26609, .T. ) ;
#26796 = DIRECTION ( 'NONE',  ( 0.000000000000000000, 1.000000000000000000, 0.000000000000000000 ) ) ;
#26797 = EDGE_CURVE ( 'NONE', #1790, #23695, #16109, .T. ) ;
#26798 = ORIENTED_EDGE ( 'NONE', *, *, #26658, .F. ) ;
#26799 = DIRECTION ( 'NONE',  ( -1.101824276508909887E-16, 1.000000000000000000, -0.000000000000000000 ) ) ;
#26800 = AXIS2_PLACEMENT_3D ( 'NONE', #15136, #20214, #5452 ) ;
#26801 = DIRECTION ( 'NONE',  ( 0.2756373558169954441, -0.9612616959383198934, 1.479773560108263204E-16 ) ) ;
#26802 = CARTESIAN_POINT ( 'NONE',  ( -29.67914774177176795, 11.17072198059736365, 22.77948424423242813 ) ) ;
#26803 = CARTESIAN_POINT ( 'NONE',  ( 47.09785597605719687, 30.56454579224779522, 47.04930799450078638 ) ) ;
#26804 = VERTEX_POINT ( 'NONE', #26561 ) ;
#26805 = CARTESIAN_POINT ( 'NONE',  ( -39.54153637835258905, -5.935542461338363829, 77.87913874700778649 ) ) ;
#26806 = CARTESIAN_POINT ( 'NONE',  ( 8.823509210239503631, 23.84164230456639544, 47.04930799450051637 ) ) ;
#26807 = DIRECTION ( 'NONE',  ( 2.779292025043186357E-18, -1.288349127009862211E-17, 1.000000000000000000 ) ) ;
#26808 = VERTEX_POINT ( 'NONE', #21630 ) ;
#26809 = ORIENTED_EDGE ( 'NONE', *, *, #20084, .T. ) ;
#26810 = CARTESIAN_POINT ( 'NONE',  ( -40.10975985016548151, 6.833710191006538537, 39.48304619656028791 ) ) ;
#26811 = CARTESIAN_POINT ( 'NONE',  ( 47.20547626766765603, 29.67451373492759004, 44.97710074790751378 ) ) ;
#26812 = CARTESIAN_POINT ( 'NONE',  ( -38.36853489569023168, 7.065850718397949315, 32.04930799450052348 ) ) ;
#26813 = DIRECTION ( 'NONE',  ( 0.000000000000000000, 1.000000000000000000, 0.000000000000000000 ) ) ;
#26814 = CIRCLE ( 'NONE', #5342, 0.1249999999999983763 ) ;
#26815 = ORIENTED_EDGE ( 'NONE', *, *, #20436, .F. ) ;
#26816 = CARTESIAN_POINT ( 'NONE',  ( 46.19123036519361136, 29.39672067899820362, 49.13362621058115565 ) ) ;
#26817 = AXIS2_PLACEMENT_3D ( 'NONE', #27334, #12569, #22558 ) ;
#26818 = ORIENTED_EDGE ( 'NONE', *, *, #7036, .T. ) ;
#26819 = VECTOR ( 'NONE', #14494, 1000.000000000000000 ) ;
#26820 = EDGE_LOOP ( 'NONE', ( #21297, #30879, #9588, #20559 ) ) ;
#26821 = CARTESIAN_POINT ( 'NONE',  ( -40.60497062835319326, 7.562013838793847142, 53.87859731638185679 ) ) ;
#26822 = ADVANCED_FACE ( 'NONE', ( #9498 ), #14551, .F. ) ;
#26823 = AXIS2_PLACEMENT_3D ( 'NONE', #12440, #7177, #22424 ) ;
#26824 = DIRECTION ( 'NONE',  ( -1.101824276508909887E-16, 1.000000000000000000, -0.000000000000000000 ) ) ;
#26825 = CARTESIAN_POINT ( 'NONE',  ( -29.94453746500173352, 11.54296414969715734, 70.26170135685566720 ) ) ;
#26826 = CARTESIAN_POINT ( 'NONE',  ( 33.50134396954518934, 32.09164230456639899, 47.04930799450051637 ) ) ;
#26827 = ORIENTED_EDGE ( 'NONE', *, *, #23204, .T. ) ;
#26828 = FACE_OUTER_BOUND ( 'NONE', #27353, .T. ) ;
#26829 = ORIENTED_EDGE ( 'NONE', *, *, #25492, .F. ) ;
#26830 = CIRCLE ( 'NONE', #24131, 0.1250000000000001110 ) ;
#26831 = CIRCLE ( 'NONE', #12714, 0.1250000000000001110 ) ;
#26832 = DIRECTION ( 'NONE',  ( -1.000000000000000000, 0.000000000000000000, 0.000000000000000000 ) ) ;
#26833 = AXIS2_PLACEMENT_3D ( 'NONE', #28307, #26962, #19409 ) ;
#26834 = CARTESIAN_POINT ( 'NONE',  ( -3.642799471247537113, 10.95964320463251163, 97.72816333341694417 ) ) ;
#26835 = ADVANCED_FACE ( 'NONE', ( #19162 ), #10362, .T. ) ;
#26836 = CARTESIAN_POINT ( 'NONE',  ( 72.68065935034339020, 11.88159288520708401, 68.55220373536670309 ) ) ;
#26837 = EDGE_LOOP ( 'NONE', ( #1917, #31525, #5886, #810 ) ) ;
#26838 = DIRECTION ( 'NONE',  ( -0.000000000000000000, -1.000000000000000000, 0.000000000000000000 ) ) ;
#26839 = CARTESIAN_POINT ( 'NONE',  ( 40.59785597605721108, 13.86454579224779948, 47.04930799450052348 ) ) ;
#26840 = SURFACE_STYLE_FILL_AREA ( #4515 ) ;
#26841 = CARTESIAN_POINT ( 'NONE',  ( 33.37634396954522487, 28.84164230456639544, 47.04930799450051637 ) ) ;
#26842 = CARTESIAN_POINT ( 'NONE',  ( -43.38408989745150990, 1.111547985471240008, 53.64930799450051779 ) ) ;
#26843 = DIRECTION ( 'NONE',  ( -1.000000000000000000, -1.101824276508909887E-16, 0.000000000000000000 ) ) ;
#26844 = CARTESIAN_POINT ( 'NONE',  ( 48.96093869543725674, 24.76454579224779806, 50.70155699761480861 ) ) ;
#26845 = ORIENTED_EDGE ( 'NONE', *, *, #30063, .F. ) ;
#26846 = CARTESIAN_POINT ( 'NONE',  ( -40.11036131418492090, 6.815955993705607341, 34.73729068726325409 ) ) ;
#26847 = LINE ( 'NONE', #29478, #13834 ) ;
#26848 = EDGE_LOOP ( 'NONE', ( #15717, #6031, #1041 ) ) ;
#26849 = CARTESIAN_POINT ( 'NONE',  ( -45.73385703294348303, -5.935454207752201228, 53.94857996627248298 ) ) ;
#26850 = DIRECTION ( 'NONE',  ( 0.000000000000000000, 1.000000000000000000, 9.698999007525318993E-17 ) ) ;
#26851 = CONICAL_SURFACE ( 'NONE', #3251, 1.003191532947548925, 0.7853981633974477239 ) ;
#26852 = EDGE_LOOP ( 'NONE', ( #12143, #5940, #1856, #6240 ) ) ;
#26853 = ADVANCED_FACE ( 'NONE', ( #6701 ), #29350, .T. ) ;
#26854 = ORIENTED_EDGE ( 'NONE', *, *, #14053, .T. ) ;
#26856 = EDGE_CURVE ( 'NONE', #16020, #5063, #25165, .T. ) ;
#26855 = TOROIDAL_SURFACE ( 'NONE', #27447, 0.9000000000000003553, 0.1000000000000000056 ) ;
#26857 = ORIENTED_EDGE ( 'NONE', *, *, #17149, .F. ) ;
#26858 = VECTOR ( 'NONE', #21632, 1000.000000000000114 ) ;
#26859 = CIRCLE ( 'NONE', #31067, 2.499999999999997335 ) ;
#26860 = ADVANCED_FACE ( 'NONE', ( #32148 ), #21460, .F. ) ;
#26861 = EDGE_CURVE ( 'NONE', #31117, #10313, #11512, .T. ) ;
#26862 = CARTESIAN_POINT ( 'NONE',  ( 33.72499318558949000, 38.56284415653841791, 47.04930799450051637 ) ) ;
#26863 = EDGE_LOOP ( 'NONE', ( #25709, #19789, #18349, #25089 ) ) ;
#26864 = ORIENTED_EDGE ( 'NONE', *, *, #29233, .F. ) ;
#26865 = FACE_OUTER_BOUND ( 'NONE', #31020, .T. ) ;
#26866 = CIRCLE ( 'NONE', #32109, 12.62506659569710443 ) ;
#26867 = CARTESIAN_POINT ( 'NONE',  ( 48.01680169312755453, 22.93807716476589675, 45.63279442905645311 ) ) ;
#26868 = CYLINDRICAL_SURFACE ( 'NONE', #6584, 12.62506659569710266 ) ;
#26869 = DIRECTION ( 'NONE',  ( 0.000000000000000000, -0.000000000000000000, -1.000000000000000000 ) ) ;
#26870 = CARTESIAN_POINT ( 'NONE',  ( 48.37829923888483563, 29.59452976649964384, 45.07556196625585443 ) ) ;
#26871 = EDGE_CURVE ( 'NONE', #23906, #22442, #20956, .T. ) ;
#26872 = EDGE_LOOP ( 'NONE', ( #32231, #5277, #25401 ) ) ;
#26873 = CARTESIAN_POINT ( 'NONE',  ( 33.50134396954519644, 31.59164230456639544, 47.04930799450051637 ) ) ;
#26874 = ORIENTED_EDGE ( 'NONE', *, *, #179, .T. ) ;
#26875 = CARTESIAN_POINT ( 'NONE',  ( -11.70578502262792320, 0.9814505390143252184, -5.472609761470430101 ) ) ;
#26876 = EDGE_LOOP ( 'NONE', ( #9604, #10249, #23308, #4409 ) ) ;
#26877 = CYLINDRICAL_SURFACE ( 'NONE', #18380, 0.1000000000000007272 ) ;
#26878 = DIRECTION ( 'NONE',  ( 0.000000000000000000, -0.000000000000000000, -1.000000000000000000 ) ) ;
#26879 = CARTESIAN_POINT ( 'NONE',  ( -40.59290754354907449, 7.518856927436782911, 60.12739743091343314 ) ) ;
#26880 = DIRECTION ( 'NONE',  ( -1.101824276508909887E-16, 1.000000000000000000, -0.000000000000000000 ) ) ;
#26881 = CARTESIAN_POINT ( 'NONE',  ( 45.73035263060504718, 27.23954579807170262, 44.36855633853329550 ) ) ;
#26882 = AXIS2_PLACEMENT_3D ( 'NONE', #22240, #29975, #410 ) ;
#26883 = CARTESIAN_POINT ( 'NONE',  ( 46.74326305241309853, 23.03451764446789696, 48.20531202744201238 ) ) ;
#26884 = CARTESIAN_POINT ( 'NONE',  ( -4.902144023942810236, 30.56454579224779522, 47.04930799450042400 ) ) ;
#26885 = ORIENTED_EDGE ( 'NONE', *, *, #2452, .F. ) ;
#26886 = DIRECTION ( 'NONE',  ( -0.000000000000000000, -1.000000000000000000, 0.000000000000000000 ) ) ;
#26887 = CYLINDRICAL_SURFACE ( 'NONE', #7247, 0.1000000000000020595 ) ;
#26888 = CARTESIAN_POINT ( 'NONE',  ( 8.698509210239588896, 32.59164230456639899, 47.04930799450051637 ) ) ;
#26889 = DIRECTION ( 'NONE',  ( -1.101824276508909887E-16, 1.000000000000000000, -0.000000000000000000 ) ) ;
#26890 = CARTESIAN_POINT ( 'NONE',  ( -38.57628410747783221, 2.267350949466874432, 14.79705809024468088 ) ) ;
#26891 = EDGE_LOOP ( 'NONE', ( #30109, #12562, #18525, #9818 ) ) ;
#26892 = CARTESIAN_POINT ( 'NONE',  ( 21.09785597605720753, 15.57592086119046826, 47.04930799450052348 ) ) ;
#26893 = EDGE_CURVE ( 'NONE', #11047, #13254, #27658, .T. ) ;
#26894 = ORIENTED_EDGE ( 'NONE', *, *, #14409, .T. ) ;
#26895 = DIRECTION ( 'NONE',  ( -1.101824276508909887E-16, 1.000000000000000000, -0.000000000000000000 ) ) ;
#26896 = DIRECTION ( 'NONE',  ( -1.000000000000000000, 0.000000000000000000, 0.000000000000000000 ) ) ;
#26897 = ADVANCED_FACE ( 'NONE', ( #886 ), #15188, .T. ) ;
#26898 = ORIENTED_EDGE ( 'NONE', *, *, #7192, .T. ) ;
#26899 = AXIS2_PLACEMENT_3D ( 'NONE', #23449, #11149, #21131 ) ;
#26900 = AXIS2_PLACEMENT_3D ( 'NONE', #15563, #30352, #23438 ) ;
#26901 = EDGE_CURVE ( 'NONE', #5223, #32221, #26723, .T. ) ;
#26902 = EDGE_CURVE ( 'NONE', #22757, #28878, #10762, .T. ) ;
#26903 = CONICAL_SURFACE ( 'NONE', #14327, 54.50502525316942126, 0.7853981633974552734 ) ;
#26904 =( BOUNDED_CURVE ( )  B_SPLINE_CURVE ( 3, ( #13210, #871, #23200, #18259 ),
 .UNSPECIFIED., .F., .F. ) 
 B_SPLINE_CURVE_WITH_KNOTS ( ( 4, 4 ),
 ( 1.575603059825828550E-14, 1.570796326794877462 ),
 .UNSPECIFIED. ) 
 CURVE ( )  GEOMETRIC_REPRESENTATION_ITEM ( )  RATIONAL_B_SPLINE_CURVE ( ( 1.000000000000000000, 0.8047378541243732641, 0.8047378541243732641, 1.000000000000000000 ) ) 
 REPRESENTATION_ITEM ( '' )  );
#26905 = VECTOR ( 'NONE', #31973, 1000.000000000000000 ) ;
#26906 = ORIENTED_EDGE ( 'NONE', *, *, #18618, .T. ) ;
#26907 = DIRECTION ( 'NONE',  ( 0.000000000000000000, 1.000000000000000000, -0.000000000000000000 ) ) ;
#26908 = CARTESIAN_POINT ( 'NONE',  ( 33.46699938050304013, 29.22145308207318237, 47.04930799450050927 ) ) ;
#26909 = CARTESIAN_POINT ( 'NONE',  ( 21.09992658989239089, 27.21664230456639899, 47.04930799450051637 ) ) ;
#26910 = ORIENTED_EDGE ( 'NONE', *, *, #30629, .T. ) ;
#26911 = LINE ( 'NONE', #31678, #2575 ) ;
#26912 = LINE ( 'NONE', #22627, #25950 ) ;
#26913 = CARTESIAN_POINT ( 'NONE',  ( 21.09785597605719332, 11.92558985988973497, 47.04930799450051637 ) ) ;
#26914 = ORIENTED_EDGE ( 'NONE', *, *, #2721, .F. ) ;
#26915 = ORIENTED_EDGE ( 'NONE', *, *, #5037, .F. ) ;
#26916 = ORIENTED_EDGE ( 'NONE', *, *, #1296, .T. ) ;
#26917 = CARTESIAN_POINT ( 'NONE',  ( 21.09785597605719332, 24.86454579224779948, 47.04930799450051637 ) ) ;
#26918 = CARTESIAN_POINT ( 'NONE',  ( 33.46699938050304013, 25.46183152705960140, 47.04930799450051637 ) ) ;
#26919 = CIRCLE ( 'NONE', #19029, 12.62506659569710266 ) ;
#26920 = CARTESIAN_POINT ( 'NONE',  ( 21.09785597605719332, 25.56454579224779877, 47.04930799450051637 ) ) ;
#26921 = DIRECTION ( 'NONE',  ( 0.000000000000000000, 0.000000000000000000, 1.000000000000000000 ) ) ;
#26922 = ORIENTED_EDGE ( 'NONE', *, *, #31795, .F. ) ;
#26923 = VERTEX_POINT ( 'NONE', #30936 ) ;
#26924 = DIRECTION ( 'NONE',  ( 0.9612616959383221138, 0.2756373558169876170, 0.000000000000000000 ) ) ;
#26925 = CYLINDRICAL_SURFACE ( 'NONE', #8329, 0.1000000000000014905 ) ;
#26926 = VECTOR ( 'NONE', #8129, 1000.000000000000114 ) ;
#26927 = CARTESIAN_POINT ( 'NONE',  ( 21.09785597605720397, -19.93545420775220123, -37.95069200549950494 ) ) ;
#26928 = ORIENTED_EDGE ( 'NONE', *, *, #4971, .F. ) ;
#26929 = CARTESIAN_POINT ( 'NONE',  ( -12.49256779602912459, -3.654479441960576835, -8.942264808892717909 ) ) ;
#26930 = FACE_OUTER_BOUND ( 'NONE', #23215, .T. ) ;
#26931 = EDGE_CURVE ( 'NONE', #12816, #12417, #27230, .T. ) ;
#26932 = EDGE_LOOP ( 'NONE', ( #19773, #11177, #26960, #22853 ) ) ;
#26933 = DIRECTION ( 'NONE',  ( -1.188208965918165239E-16, -1.880121038077813132E-16, -1.000000000000000000 ) ) ;
#26934 = CARTESIAN_POINT ( 'NONE',  ( 50.10320668408830613, 25.60621246473838042, 47.20539118556276037 ) ) ;
#26935 = DIRECTION ( 'NONE',  ( -1.101824276508909887E-16, 1.000000000000000000, -0.000000000000000000 ) ) ;
#26936 = VECTOR ( 'NONE', #4846, 1000.000000000000000 ) ;
#26937 = EDGE_CURVE ( 'NONE', #22536, #32221, #10483, .T. ) ;
#26938 = ORIENTED_EDGE ( 'NONE', *, *, #9543, .F. ) ;
#26939 = AXIS2_PLACEMENT_3D ( 'NONE', #3090, #7879, #15418 ) ;
#26940 = CARTESIAN_POINT ( 'NONE',  ( -16.40214402394279958, 14.86454579224779948, 47.04930799450052348 ) ) ;
#26941 = DIRECTION ( 'NONE',  ( -0.000000000000000000, 1.000000000000000000, -0.000000000000000000 ) ) ;
#26942 = DIRECTION ( 'NONE',  ( -0.000000000000000000, 1.000000000000000000, -0.000000000000000000 ) ) ;
#26943 = CARTESIAN_POINT ( 'NONE',  ( 46.00908685603034343, 27.63284706826092929, 44.91496614357595263 ) ) ;
#26944 = ORIENTED_EDGE ( 'NONE', *, *, #22205, .T. ) ;
#26945 = CARTESIAN_POINT ( 'NONE',  ( -40.52510752649232728, 7.677764709599123272, 39.54930799450052348 ) ) ;
#26946 = CARTESIAN_POINT ( 'NONE',  ( 21.09785597605719332, 30.56454579224779522, 47.04930799450051637 ) ) ;
#26947 = CARTESIAN_POINT ( 'NONE',  ( 50.76169387283900392, 6.453333540778361410, -3.825706102817799881 ) ) ;
#26948 = DIRECTION ( 'NONE',  ( 1.000000000000000000, 0.000000000000000000, 0.000000000000000000 ) ) ;
#26949 = DIRECTION ( 'NONE',  ( 0.4848096202463424431, 0.8746197071393927436, -2.220446049250312588E-16 ) ) ;
#26950 = DIRECTION ( 'NONE',  ( -1.188208965918165239E-16, -1.880121038077813132E-16, -1.000000000000000000 ) ) ;
#26951 = CARTESIAN_POINT ( 'NONE',  ( -29.43068460852080293, -13.74047052604243646, 76.22825493111784567 ) ) ;
#26952 = DIRECTION ( 'NONE',  ( -1.000000000000000000, 0.000000000000000000, 0.000000000000000000 ) ) ;
#26953 = CARTESIAN_POINT ( 'NONE',  ( -40.63181322188042088, 6.822514116776794424, 39.52939200191682545 ) ) ;
#26954 = ORIENTED_EDGE ( 'NONE', *, *, #30400, .F. ) ;
#26955 = CARTESIAN_POINT ( 'NONE',  ( 45.75738744548056758, 22.91413368675619111, 45.84342743610336868 ) ) ;
#26956 = CARTESIAN_POINT ( 'NONE',  ( -40.44670421500372015, 8.525092865626815453, 34.54930799450052348 ) ) ;
#26957 = CARTESIAN_POINT ( 'NONE',  ( -29.38155059246552625, 10.03279525182523813, 20.77577928944664265 ) ) ;
#26958 = CARTESIAN_POINT ( 'NONE',  ( 45.96182992765472619, 27.30087065737811969, 44.82232689504102296 ) ) ;
#26959 = TOROIDAL_SURFACE ( 'NONE', #2853, 13.98419020052803852, 1.000000000001014744 ) ;
#26960 = ORIENTED_EDGE ( 'NONE', *, *, #28144, .T. ) ;
#26961 = FACE_OUTER_BOUND ( 'NONE', #14859, .T. ) ;
#26962 = DIRECTION ( 'NONE',  ( 0.000000000000000000, -0.000000000000000000, -1.000000000000000000 ) ) ;
#26963 = DIRECTION ( 'NONE',  ( -1.000000000000000000, 0.000000000000000000, 0.000000000000000000 ) ) ;
#26964 = AXIS2_PLACEMENT_3D ( 'NONE', #32170, #17216, #26751 ) ;
#26965 = ORIENTED_EDGE ( 'NONE', *, *, #1293, .F. ) ;
#26966 = ORIENTED_EDGE ( 'NONE', *, *, #16149, .F. ) ;
#26968 = AXIS2_PLACEMENT_3D ( 'NONE', #2001, #11256, #12020 ) ;
#26967 = CARTESIAN_POINT ( 'NONE',  ( -40.11688989807090167, 6.803825020423238890, 39.45035836127284767 ) ) ;
#26969 = DIRECTION ( 'NONE',  ( -0.2756373558169932236, 0.9612616959383206705, -2.468067202294475228E-14 ) ) ;
#26970 = AXIS2_PLACEMENT_3D ( 'NONE', #17912, #26100, #13163 ) ;
#26971 = CIRCLE ( 'NONE', #1282, 0.1250000000000001110 ) ;
#26972 = DIRECTION ( 'NONE',  ( 1.000000000000000000, 0.000000000000000000, 0.000000000000000000 ) ) ;
#26973 = CARTESIAN_POINT ( 'NONE',  ( 52.07598125554711999, -5.935454207752202116, 97.45038561958638468 ) ) ;
#26974 = AXIS2_PLACEMENT_3D ( 'NONE', #15807, #13352, #4127 ) ;
#26975 = VERTEX_POINT ( 'NONE', #13228 ) ;
#26976 = CARTESIAN_POINT ( 'NONE',  ( 71.61633006602951923, 10.39302479005549884, 21.28398100033225404 ) ) ;
#26977 = ORIENTED_EDGE ( 'NONE', *, *, #9122, .T. ) ;
#26978 = EDGE_CURVE ( 'NONE', #2756, #2200, #11008, .T. ) ;
#26979 = ORIENTED_EDGE ( 'NONE', *, *, #6304, .F. ) ;
#26980 = ADVANCED_FACE ( 'NONE', ( #30619 ), #17804, .T. ) ;
#26981 = EDGE_CURVE ( 'NONE', #31427, #2267, #4175, .T. ) ;
#26982 = EDGE_CURVE ( 'NONE', #4576, #593, #30421, .T. ) ;
#26983 = CARTESIAN_POINT ( 'NONE',  ( -41.88090303775678080, 13.82677487427665497, 54.64930799450051779 ) ) ;
#26984 = EDGE_LOOP ( 'NONE', ( #14996, #1975, #24395, #25327 ) ) ;
#26985 = AXIS2_PLACEMENT_3D ( 'NONE', #23323, #25778, #8227 ) ;
#26986 = LINE ( 'NONE', #14520, #27590 ) ;
#26987 = CARTESIAN_POINT ( 'NONE',  ( -32.86366169284681860, -2.090386383962613781, 80.76226970107140346 ) ) ;
#26988 = AXIS2_PLACEMENT_3D ( 'NONE', #15776, #22993, #5449 ) ;
#26989 = CARTESIAN_POINT ( 'NONE',  ( 33.72499318558949710, 24.09184655352419213, 47.04930799450051637 ) ) ;
#26990 = AXIS2_PLACEMENT_3D ( 'NONE', #10369, #13644, #23160 ) ;
#26991 = CIRCLE ( 'NONE', #12867, 12.36707279061065101 ) ;
#26992 = VERTEX_POINT ( 'NONE', #10432 ) ;
#26993 = DIRECTION ( 'NONE',  ( -0.000000000000000000, 1.000000000000000000, -0.000000000000000000 ) ) ;
#26994 = ORIENTED_EDGE ( 'NONE', *, *, #13761, .F. ) ;
#26995 = CIRCLE ( 'NONE', #9711, 12.36707279061065101 ) ;
#26996 = CARTESIAN_POINT ( 'NONE',  ( 21.09992658989238734, 38.56284415653841791, 47.04930799450051637 ) ) ;
#26997 = CARTESIAN_POINT ( 'NONE',  ( 21.09785597605719332, 11.78014697381582643, 47.04930799450051637 ) ) ;
#26998 = CARTESIAN_POINT ( 'NONE',  ( -40.68740604810007966, 6.795923245628763709, 39.47252729750491795 ) ) ;
#26999 = EDGE_LOOP ( 'NONE', ( #934, #15253, #24965, #23101 ) ) ;
#27000 = DIRECTION ( 'NONE',  ( 0.5932111027100931411, 0.7071067811865471286, 0.3848383915638819985 ) ) ;
#27001 = DIRECTION ( 'NONE',  ( -1.101824276508909887E-16, 1.000000000000000000, -0.000000000000000000 ) ) ;
#27002 = DIRECTION ( 'NONE',  ( 1.234978253042719660E-16, -1.000000000000000000, -1.109335647967047851E-31 ) ) ;
#27003 = DIRECTION ( 'NONE',  ( 0.000000000000000000, -0.000000000000000000, 1.000000000000000000 ) ) ;
#27004 = CYLINDRICAL_SURFACE ( 'NONE', #27306, 43.00000000000000000 ) ;
#27005 = CARTESIAN_POINT ( 'NONE',  ( -40.19913497620437681, 7.013551051776422796, 34.87324101432411538 ) ) ;
#27006 = ORIENTED_EDGE ( 'NONE', *, *, #18887, .F. ) ;
#27007 = LINE ( 'NONE', #14057, #1789 ) ;
#27008 = ORIENTED_EDGE ( 'NONE', *, *, #27068, .F. ) ;
#27010 = EDGE_CURVE ( 'NONE', #17564, #18267, #10276, .T. ) ;
#27009 = DIRECTION ( 'NONE',  ( -0.000000000000000000, -1.000000000000000000, 0.000000000000000000 ) ) ;
#27011 = LINE ( 'NONE', #19120, #18993 ) ;
#27012 = VERTEX_POINT ( 'NONE', #10603 ) ;
#27013 = AXIS2_PLACEMENT_3D ( 'NONE', #30519, #23437, #12800 ) ;
#27014 = VERTEX_POINT ( 'NONE', #12905 ) ;
#27015 = VECTOR ( 'NONE', #16371, 1000.000000000000114 ) ;
#27016 = CIRCLE ( 'NONE', #25959, 12.62506659569710266 ) ;
#27017 =( GEOMETRIC_REPRESENTATION_CONTEXT ( 3 ) GLOBAL_UNCERTAINTY_ASSIGNED_CONTEXT ( ( #10811 ) ) GLOBAL_UNIT_ASSIGNED_CONTEXT ( ( #14172, #32051, #29252 ) ) REPRESENTATION_CONTEXT ( 'NONE', 'WORKASPACE' ) );
#27018 = AXIS2_PLACEMENT_3D ( 'NONE', #19099, #8943, #4507 ) ;
#27019 = ORIENTED_EDGE ( 'NONE', *, *, #16737, .T. ) ;
#27020 = EDGE_CURVE ( 'NONE', #32314, #27140, #20592, .T. ) ;
#27021 = ADVANCED_FACE ( 'NONE', ( #28311 ), #12745, .F. ) ;
#27022 = EDGE_CURVE ( 'NONE', #31909, #8721, #6639, .T. ) ;
#27023 = AXIS2_PLACEMENT_3D ( 'NONE', #16885, #12299, #24279 ) ;
#27024 = CARTESIAN_POINT ( 'NONE',  ( 33.72499318558949710, 28.59184655352419213, 47.04930799450051637 ) ) ;
#27025 = ORIENTED_EDGE ( 'NONE', *, *, #22662, .F. ) ;
#27026 = ORIENTED_EDGE ( 'NONE', *, *, #12683, .T. ) ;
#27027 = DIRECTION ( 'NONE',  ( 0.2756373558169956106, -0.9612616959383200044, -1.315048337272770743E-17 ) ) ;
#27028 = DIRECTION ( 'NONE',  ( -1.101824276508909887E-16, 1.000000000000000000, -0.000000000000000000 ) ) ;
#27029 = CARTESIAN_POINT ( 'NONE',  ( 21.09785597605720753, 13.86454579224779948, 47.04930799450052348 ) ) ;
#27030 = DIRECTION ( 'NONE',  ( 0.5442436726714897643, 1.289618226626749726E-16, -0.8389271868029121171 ) ) ;
#27031 = CARTESIAN_POINT ( 'NONE',  ( 21.09992658989239089, 24.59164230456639544, 47.04930799450051637 ) ) ;
#27032 = VERTEX_POINT ( 'NONE', #22892 ) ;
#27033 = CARTESIAN_POINT ( 'NONE',  ( -43.90780810587784089, -0.03953120679776574165, 32.04930799450052348 ) ) ;
#27034 = ORIENTED_EDGE ( 'NONE', *, *, #16802, .F. ) ;
#27036 = CARTESIAN_POINT ( 'NONE',  ( -10.78113380436533220, -5.738638231773887100, -10.34064955166817867 ) ) ;
#27035 = CIRCLE ( 'NONE', #31751, 0.1250000000000001110 ) ;
#27037 = VERTEX_POINT ( 'NONE', #7974 ) ;
#27038 = CARTESIAN_POINT ( 'NONE',  ( 21.09992658989239089, 24.09143805560860940, 47.04930799450051637 ) ) ;
#27039 = CARTESIAN_POINT ( 'NONE',  ( 21.09992658989239089, 28.96183152705961206, 47.04930799450051637 ) ) ;
#27040 = CARTESIAN_POINT ( 'NONE',  ( -40.60333149162104860, 7.557375771971046596, 60.08350751967648762 ) ) ;
#27041 = DIRECTION ( 'NONE',  ( 0.000000000000000000, 0.000000000000000000, -1.000000000000000000 ) ) ;
#27042 = CARTESIAN_POINT ( 'NONE',  ( 44.91142894931555674, 27.29787913140504330, 45.63089057098605394 ) ) ;
#27043 = CARTESIAN_POINT ( 'NONE',  ( 47.22573328838134188, 23.12036939723557083, 47.29998918090146987 ) ) ;
#27044 = CARTESIAN_POINT ( 'NONE',  ( 45.22719185251098395, 19.86454579224779948, 48.00356987515886686 ) ) ;
#27045 = EDGE_LOOP ( 'NONE', ( #22150, #11680, #29994, #147 ) ) ;
#27046 = CARTESIAN_POINT ( 'NONE',  ( 47.14149656544282863, 29.59378199361933781, 44.97899958470305393 ) ) ;
#27048 = EDGE_CURVE ( 'NONE', #16381, #25031, #497, .T. ) ;
#27047 = CARTESIAN_POINT ( 'NONE',  ( 21.09992658989239089, 28.97145308207318237, 47.04930799450051637 ) ) ;
#27049 = DIRECTION ( 'NONE',  ( -0.9612616959383206705, -0.2756373558169934457, 1.660411357259282938E-16 ) ) ;
#27050 = EDGE_CURVE ( 'NONE', #28202, #16423, #22528, .T. ) ;
#27051 = AXIS2_PLACEMENT_3D ( 'NONE', #19592, #29950, #29618 ) ;
#27052 = LINE ( 'NONE', #2272, #5902 ) ;
#27053 = CARTESIAN_POINT ( 'NONE',  ( -40.98031486389898248, 9.265261353013489298, 39.44930799450052206 ) ) ;
#27054 = ORIENTED_EDGE ( 'NONE', *, *, #2306, .T. ) ;
#27055 = ORIENTED_EDGE ( 'NONE', *, *, #5995, .F. ) ;
#27056 = EDGE_LOOP ( 'NONE', ( #28536, #27683, #30673, #16958, #29689, #24554, #19492, #11321, #7195, #29148, #27787, #14697, #21954, #18200, #23930, #29882 ) ) ;
#27057 = EDGE_CURVE ( 'NONE', #29530, #4744, #21377, .T. ) ;
#27058 = VECTOR ( 'NONE', #15943, 1000.000000000000000 ) ;
#27059 = VERTEX_POINT ( 'NONE', #16306 ) ;
#27060 = DIRECTION ( 'NONE',  ( -1.000000000000000000, 0.000000000000000000, 0.000000000000000000 ) ) ;
#27061 = CARTESIAN_POINT ( 'NONE',  ( 53.16981722132879185, -5.983766253076979069, -3.337848843846767721 ) ) ;
#27062 = CARTESIAN_POINT ( 'NONE',  ( 21.09785597605720753, 17.16474120167318418, 47.04930799450052348 ) ) ;
#27063 = AXIS2_PLACEMENT_3D ( 'NONE', #17707, #14612, #1963 ) ;
#27064 = ORIENTED_EDGE ( 'NONE', *, *, #1706, .F. ) ;
#27065 = LINE ( 'NONE', #1954, #20887 ) ;
#27066 = CARTESIAN_POINT ( 'NONE',  ( -39.67555847965937943, 2.645252416024337361, 45.74930799450051211 ) ) ;
#27067 = DIRECTION ( 'NONE',  ( 0.000000000000000000, 1.000000000000000000, 3.754529891495955404E-16 ) ) ;
#27068 = EDGE_CURVE ( 'NONE', #18631, #13067, #11385, .T. ) ;
#27069 = ORIENTED_EDGE ( 'NONE', *, *, #19045, .T. ) ;
#27070 = ORIENTED_EDGE ( 'NONE', *, *, #23066, .T. ) ;
#27071 = CARTESIAN_POINT ( 'NONE',  ( -43.38408989745150990, 1.111547985471239786, 60.44930799450051495 ) ) ;
#27072 = ORIENTED_EDGE ( 'NONE', *, *, #17675, .F. ) ;
#27073 = EDGE_CURVE ( 'NONE', #25738, #9355, #1042, .T. ) ;
#27074 = FACE_OUTER_BOUND ( 'NONE', #30545, .T. ) ;
#27075 = CARTESIAN_POINT ( 'NONE',  ( 21.09785597605720042, -13.59284023713420630, -8.674624342367264873 ) ) ;
#27076 = LINE ( 'NONE', #6412, #25813 ) ;
#27077 = CARTESIAN_POINT ( 'NONE',  ( 21.09992658989239089, 28.09184655352419213, 47.04930799450051637 ) ) ;
#27078 = ORIENTED_EDGE ( 'NONE', *, *, #15759, .T. ) ;
#27079 = ORIENTED_EDGE ( 'NONE', *, *, #11937, .T. ) ;
#27080 = DIRECTION ( 'NONE',  ( 1.000000000000000000, 0.000000000000000000, 0.000000000000000000 ) ) ;
#27081 = ADVANCED_FACE ( 'NONE', ( #13700 ), #5244, .T. ) ;
#27082 = CIRCLE ( 'NONE', #17120, 12.78419020052701960 ) ;
#27083 = DIRECTION ( 'NONE',  ( 0.4848096202463636484, 0.8746197071393810862, 0.000000000000000000 ) ) ;
#27084 = ADVANCED_FACE ( 'NONE', ( #6627 ), #4698, .T. ) ;
#27085 = EDGE_CURVE ( 'NONE', #14523, #11099, #13630, .T. ) ;
#27086 = DIRECTION ( 'NONE',  ( -1.101824276508909887E-16, 1.000000000000000000, -0.000000000000000000 ) ) ;
#27087 = EDGE_LOOP ( 'NONE', ( #1098, #1097, #11430, #26291 ) ) ;
#27088 = CARTESIAN_POINT ( 'NONE',  ( -12.24974552980923015, -4.258649047046816349, -9.476481744674682517 ) ) ;
#27089 = DIRECTION ( 'NONE',  ( 0.000000000000000000, -0.000000000000000000, -1.000000000000000000 ) ) ;
#27090 = ORIENTED_EDGE ( 'NONE', *, *, #8252, .F. ) ;
#27091 = FACE_OUTER_BOUND ( 'NONE', #11880, .T. ) ;
#27092 = DIRECTION ( 'NONE',  ( -1.000000000000000000, -1.101824276508909764E-16, 0.000000000000000000 ) ) ;
#27093 = AXIS2_PLACEMENT_3D ( 'NONE', #21974, #20174, #25107 ) ;
#27094 = LINE ( 'NONE', #24797, #6547 ) ;
#27095 =( BOUNDED_CURVE ( )  B_SPLINE_CURVE ( 2, ( #19873, #29906, #4953, #2483, #12512, #30068, #8223, #31033, #8380 ),
 .UNSPECIFIED., .F., .F. ) 
 B_SPLINE_CURVE_WITH_KNOTS ( ( 3, 2, 2, 2, 3 ),
 ( 0.3214285725898440860, 0.3333333333333333148, 0.3571428571428571508, 0.3809523809523809312, 0.3928571440184155938 ),
 .UNSPECIFIED. ) 
 CURVE ( )  GEOMETRIC_REPRESENTATION_ITEM ( )  RATIONAL_B_SPLINE_CURVE ( ( 0.9330127018922200755, 0.9330127084266228721, 1.000000000000000000, 0.8660254037844388186, 1.000000000000000000, 0.8660254037844388186, 1.000000000000000000, 0.9330126953578155025, 0.9330127018922200755 ) ) 
 REPRESENTATION_ITEM ( '' )  );
#27096 = EDGE_CURVE ( 'NONE', #9876, #16357, #20438, .T. ) ;
#27097 = ORIENTED_EDGE ( 'NONE', *, *, #19102, .F. ) ;
#27098 = EDGE_LOOP ( 'NONE', ( #19910, #19427, #3778, #17276 ) ) ;
#27099 = CARTESIAN_POINT ( 'NONE',  ( 21.09785597605719332, 7.264443105416139801, 47.04930799450051637 ) ) ;
#27100 = AXIS2_PLACEMENT_3D ( 'NONE', #32146, #27377, #22114 ) ;
#27101 = CARTESIAN_POINT ( 'NONE',  ( 0.5978559760572086379, 13.86454579224779948, 47.04930799450052348 ) ) ;
#27102 = CARTESIAN_POINT ( 'NONE',  ( 46.99023568444673060, 26.52451373492759856, 49.12151524109405898 ) ) ;
#27103 = VERTEX_POINT ( 'NONE', #28627 ) ;
#27104 = CARTESIAN_POINT ( 'NONE',  ( 21.09785597605719332, 15.43591091851532759, 61.03349819502855667 ) ) ;
#27105 = DIRECTION ( 'NONE',  ( -1.000000000000000000, 0.000000000000000000, 0.000000000000000000 ) ) ;
#27106 = EDGE_CURVE ( 'NONE', #1764, #28053, #31976, .T. ) ;
#27107 = APPLICATION_CONTEXT ( 'automotive_design' ) ;
#27108 = CARTESIAN_POINT ( 'NONE',  ( 47.79865503179234310, 9.702389020015065313, -3.412202488244239884 ) ) ;
#27109 = EDGE_CURVE ( 'NONE', #21091, #1796, #5760, .T. ) ;
#27110 = DIRECTION ( 'NONE',  ( 1.000000000000000000, 0.000000000000000000, 0.000000000000000000 ) ) ;
#27111 = DIRECTION ( 'NONE',  ( -1.000000000000000000, 0.000000000000000000, 0.000000000000000000 ) ) ;
#27112 = CARTESIAN_POINT ( 'NONE',  ( -41.23380787120766655, 11.23768311167744294, 36.00717268343339583 ) ) ;
#27113 = CARTESIAN_POINT ( 'NONE',  ( -37.12604442285837081, -13.74047052604243646, 50.86005336442920566 ) ) ;
#27114 = CARTESIAN_POINT ( 'NONE',  ( 106.0978559760575735, 11.92558985988973497, 26.63511333407112858 ) ) ;
#27115 = PRODUCT_DEFINITION_SHAPE ( 'NONE', 'NONE',  #18711 ) ;
#27116 = DIRECTION ( 'NONE',  ( 0.000000000000000000, -0.000000000000000000, -1.000000000000000000 ) ) ;
#27117 = CARTESIAN_POINT ( 'NONE',  ( -40.64500813507293486, 6.819128862114092193, 39.51928662074344345 ) ) ;
#27118 =( LENGTH_UNIT ( ) NAMED_UNIT ( * ) SI_UNIT ( .MILLI., .METRE. ) );
#27119 = ORIENTED_EDGE ( 'NONE', *, *, #17976, .T. ) ;
#27120 = CARTESIAN_POINT ( 'NONE',  ( -40.60333149162104860, 7.557375771971046596, 54.01510846932454513 ) ) ;
#27121 = CARTESIAN_POINT ( 'NONE',  ( -40.43096862161028326, 8.533258663572608427, 34.55282792453323992 ) ) ;
#27122 = EDGE_CURVE ( 'NONE', #4349, #8349, #21999, .T. ) ;
#27123 = CARTESIAN_POINT ( 'NONE',  ( -29.46345852492245854, 8.057491331218018971, 18.62581556740637367 ) ) ;
#27124 = CARTESIAN_POINT ( 'NONE',  ( 71.48501281440437083, -5.935454207752202116, 77.87546120947915540 ) ) ;
#27125 = ORIENTED_EDGE ( 'NONE', *, *, #24032, .F. ) ;
#27126 = DIRECTION ( 'NONE',  ( -1.000000000000000000, 0.000000000000000000, 0.000000000000000000 ) ) ;
#27127 = CARTESIAN_POINT ( 'NONE',  ( -43.64073206722599707, 1.267352857069778960, 34.64930799450052490 ) ) ;
#27128 = DIRECTION ( 'NONE',  ( -1.000000000000000000, -1.101824276508909887E-16, 0.000000000000000000 ) ) ;
#27129 = ORIENTED_EDGE ( 'NONE', *, *, #30304, .F. ) ;
#27130 = ORIENTED_EDGE ( 'NONE', *, *, #7981, .F. ) ;
#27131 = DIRECTION ( 'NONE',  ( -1.101824276508909887E-16, 1.000000000000000000, -0.000000000000000000 ) ) ;
#27132 = CARTESIAN_POINT ( 'NONE',  ( 44.70507715278255745, 29.84951373492758719, 46.92503878583764987 ) ) ;
#27133 = CIRCLE ( 'NONE', #6675, 12.27641737965281266 ) ;
#27134 = DIRECTION ( 'NONE',  ( -1.000000000000000000, 0.000000000000000000, 0.000000000000000000 ) ) ;
#27135 = AXIS2_PLACEMENT_3D ( 'NONE', #6065, #18517, #28699 ) ;
#27136 = DIRECTION ( 'NONE',  ( 0.2756373558169932236, -0.9612616959383206705, -2.438471731092320121E-14 ) ) ;
#27137 = CARTESIAN_POINT ( 'NONE',  ( 45.19905222922426447, 29.26819764828676895, 45.57955500106713487 ) ) ;
#27138 = AXIS2_PLACEMENT_3D ( 'NONE', #23044, #15656, #15504 ) ;
#27139 = ORIENTED_EDGE ( 'NONE', *, *, #29293, .T. ) ;
#27140 = VERTEX_POINT ( 'NONE', #23855 ) ;
#27141 = CARTESIAN_POINT ( 'NONE',  ( -41.88090303775678080, 13.82677487427666030, 54.63190069796055326 ) ) ;
#27142 = VERTEX_POINT ( 'NONE', #16618 ) ;
#27143 = CARTESIAN_POINT ( 'NONE',  ( 21.09785597605720753, 15.57592086119046826, 47.04930799450052348 ) ) ;
#27144 = CARTESIAN_POINT ( 'NONE',  ( -29.37118047130158871, 8.867344695471309990, 74.71416144101659995 ) ) ;
#27145 = CONICAL_SURFACE ( 'NONE', #11952, 13.81487396812510937, 1.187672012580059944 ) ;
#27146 = CIRCLE ( 'NONE', #30841, 2.000000000000001776 ) ;
#27147 = ORIENTED_EDGE ( 'NONE', *, *, #17151, .F. ) ;
#27148 = DIRECTION ( 'NONE',  ( -1.000000000000000000, 0.000000000000000000, 0.000000000000000000 ) ) ;
#27149 = ORIENTED_EDGE ( 'NONE', *, *, #13988, .T. ) ;
#27150 = CARTESIAN_POINT ( 'NONE',  ( 21.09785597605720042, -14.03534765547855656, 47.04930799450051637 ) ) ;
#27151 = AXIS2_PLACEMENT_3D ( 'NONE', #4244, #6544, #28871 ) ;
#27152 = CARTESIAN_POINT ( 'NONE',  ( -3.902144023942792028, 13.86454579224779948, 47.04930799450052348 ) ) ;
#27153 = CARTESIAN_POINT ( 'NONE',  ( -40.69088518708426960, 6.792375053915788108, 39.46636398561383174 ) ) ;
#27154 = ORIENTED_EDGE ( 'NONE', *, *, #15080, .F. ) ;
#27155 = DIRECTION ( 'NONE',  ( 1.000000000000000000, 0.000000000000000000, 0.000000000000000000 ) ) ;
#27156 = DIRECTION ( 'NONE',  ( 1.234978253042719660E-16, -1.000000000000000000, -1.109335647967047851E-31 ) ) ;
#27157 = FACE_OUTER_BOUND ( 'NONE', #15345, .T. ) ;
#27158 = EDGE_CURVE ( 'NONE', #32103, #27500, #6269, .T. ) ;
#27159 = DIRECTION ( 'NONE',  ( -1.101824276508909887E-16, 1.000000000000000000, -0.000000000000000000 ) ) ;
#27160 = CIRCLE ( 'NONE', #1474, 0.1249999999999983763 ) ;
#27161 = EDGE_CURVE ( 'NONE', #3559, #3723, #23038, .T. ) ;
#27162 = DIRECTION ( 'NONE',  ( 0.000000000000000000, -1.000000000000000000, 0.000000000000000000 ) ) ;
#27163 = ORIENTED_EDGE ( 'NONE', *, *, #2034, .F. ) ;
#27164 = DIRECTION ( 'NONE',  ( -1.224646799147353207E-16, -1.349345573449484691E-32, 1.000000000000000000 ) ) ;
#27165 = DIRECTION ( 'NONE',  ( 0.8746197071393926326, -0.4848096202463430537, -8.676864087101709653E-18 ) ) ;
#27166 = ORIENTED_EDGE ( 'NONE', *, *, #16737, .F. ) ;
#27167 = CARTESIAN_POINT ( 'NONE',  ( -45.63946073596905251, -5.900342692619398477, 53.66495926439285569 ) ) ;
#27168 = ORIENTED_EDGE ( 'NONE', *, *, #13286, .F. ) ;
#27169 = ORIENTED_EDGE ( 'NONE', *, *, #8490, .F. ) ;
#27170 = CONICAL_SURFACE ( 'NONE', #25077, 0.9999999999999731326, 0.4537856055185219284 ) ;
#27171 = AXIS2_PLACEMENT_3D ( 'NONE', #28805, #16319, #6480 ) ;
#27172 = CIRCLE ( 'NONE', #10959, 2.500000000000002220 ) ;
#27173 = ORIENTED_EDGE ( 'NONE', *, *, #23611, .T. ) ;
#27174 = VECTOR ( 'NONE', #31210, 1000.000000000000000 ) ;
#27175 = TOROIDAL_SURFACE ( 'NONE', #8297, 70.59901951359279337, 1.000000000000000444 ) ;
#27176 = CIRCLE ( 'NONE', #20902, 12.36707279061065101 ) ;
#27177 = CARTESIAN_POINT ( 'NONE',  ( -40.60251150970604073, 6.748447833883064462, 60.54930799450051637 ) ) ;
#27178 = ORIENTED_EDGE ( 'NONE', *, *, #5201, .T. ) ;
#27179 = ORIENTED_EDGE ( 'NONE', *, *, #14847, .F. ) ;
#27180 = CARTESIAN_POINT ( 'NONE',  ( 79.00022925220035575, -5.944439029104267469, 15.86926712089771918 ) ) ;
#27181 = DIRECTION ( 'NONE',  ( 0.000000000000000000, 0.000000000000000000, -1.000000000000000000 ) ) ;
#27182 = CARTESIAN_POINT ( 'NONE',  ( 8.482002859293427122, 26.96664230456639899, 47.04930799450051637 ) ) ;
#27183 = CARTESIAN_POINT ( 'NONE',  ( 47.09785597605719687, 25.56454579224779167, 49.54930799450078638 ) ) ;
#27184 = CYLINDRICAL_SURFACE ( 'NONE', #26770, 12.62506659569710266 ) ;
#27185 = ORIENTED_EDGE ( 'NONE', *, *, #21993, .T. ) ;
#27186 = CARTESIAN_POINT ( 'NONE',  ( 21.09785597605720753, 13.86454579224779948, 47.04930799450052348 ) ) ;
#27187 = EDGE_LOOP ( 'NONE', ( #13752, #24077 ) ) ;
#27188 = DIRECTION ( 'NONE',  ( -1.101824276508909887E-16, 1.000000000000000000, -0.000000000000000000 ) ) ;
#27189 = CARTESIAN_POINT ( 'NONE',  ( -41.04685960816998147, 9.497330455345890599, 35.54930799450052348 ) ) ;
#27190 = VECTOR ( 'NONE', #17002, 1000.000000000000114 ) ;
#27191 = EDGE_LOOP ( 'NONE', ( #12665, #6904, #3376, #13726 ) ) ;
#27192 = DIRECTION ( 'NONE',  ( 1.234978253042719660E-16, -1.000000000000000000, -1.109335647967047851E-31 ) ) ;
#27193 = CARTESIAN_POINT ( 'NONE',  ( 21.09785597605720042, -14.04221034894631615, 47.04930799450051637 ) ) ;
#27194 = CARTESIAN_POINT ( 'NONE',  ( 52.20506317732528601, -5.935651417315359168, 107.5660775608625954 ) ) ;
#27195 = CARTESIAN_POINT ( 'NONE',  ( 47.86511985000206693, 22.93807716476589320, 48.55339511290479493 ) ) ;
#27196 = CARTESIAN_POINT ( 'NONE',  ( 46.31454563678332903, 22.93807716476589675, 48.55381333958629142 ) ) ;
#27197 = CIRCLE ( 'NONE', #11400, 12.27641737965283042 ) ;
#27198 = EDGE_CURVE ( 'NONE', #13584, #12291, #7327, .T. ) ;
#27199 = ADVANCED_FACE ( 'NONE', ( #6300 ), #13856, .T. ) ;
#27200 = CARTESIAN_POINT ( 'NONE',  ( 45.24946171279598417, 26.32124452788248803, 47.99220971130007030 ) ) ;
#27201 = EDGE_CURVE ( 'NONE', #27623, #30099, #11079, .T. ) ;
#27202 = CARTESIAN_POINT ( 'NONE',  ( -41.02687597405218156, 7.220473278338834788, 53.64930799450051779 ) ) ;
#27203 = CARTESIAN_POINT ( 'NONE',  ( 21.09785597605719332, 17.16451738380053271, 47.04930799450051637 ) ) ;
#27204 = ADVANCED_FACE ( 'NONE', ( #26642 ), #18444, .T. ) ;
#27205 = VERTEX_POINT ( 'NONE', #2511 ) ;
#27206 = CARTESIAN_POINT ( 'NONE',  ( -42.28040081837337993, 14.75252016492556351, 58.96875521528360053 ) ) ;
#27207 = CARTESIAN_POINT ( 'NONE',  ( 21.09785597605720042, 15.06454579224778456, 102.0493079945005093 ) ) ;
#27208 = EDGE_LOOP ( 'NONE', ( #32388, #10016, #13820, #27555 ) ) ;
#27209 = VECTOR ( 'NONE', #1448, 1000.000000000000000 ) ;
#27210 = CARTESIAN_POINT ( 'NONE',  ( -38.57628410747783221, 5.786705267067572933, 16.84970013494222840 ) ) ;
#27211 = EDGE_LOOP ( 'NONE', ( #30038, #8559, #28266, #19510 ) ) ;
#27212 = ORIENTED_EDGE ( 'NONE', *, *, #29820, .F. ) ;
#27213 = CARTESIAN_POINT ( 'NONE',  ( 21.09785597605721463, -16.93545420775220123, 125.5493079945005093 ) ) ;
#27214 = EDGE_LOOP ( 'NONE', ( #15108, #30682, #31138, #15376 ) ) ;
#27215 = AXIS2_PLACEMENT_3D ( 'NONE', #13251, #30641, #28334 ) ;
#27216 = AXIS2_PLACEMENT_3D ( 'NONE', #15837, #3354, #405 ) ;
#27217 = ORIENTED_EDGE ( 'NONE', *, *, #23688, .F. ) ;
#27218 = CARTESIAN_POINT ( 'NONE',  ( 45.38329851326696485, 22.91413368675619111, 47.60724751575505564 ) ) ;
#27219 = ADVANCED_FACE ( 'NONE', ( #14508 ), #1577, .T. ) ;
#27220 = CARTESIAN_POINT ( 'NONE',  ( -42.37913764077812573, 15.23192269303852697, 38.54930799450052348 ) ) ;
#27221 = ADVANCED_FACE ( 'NONE', ( #9747 ), #2122, .T. ) ;
#27222 = AXIS2_PLACEMENT_3D ( 'NONE', #31856, #13980, #21832 ) ;
#27223 = CIRCLE ( 'NONE', #15710, 0.1250000000000001110 ) ;
#27224 = ORIENTED_EDGE ( 'NONE', *, *, #17213, .T. ) ;
#27225 = DIRECTION ( 'NONE',  ( -0.000000000000000000, -1.000000000000000000, 0.000000000000000000 ) ) ;
#27226 = CIRCLE ( 'NONE', #8375, 0.1000000000000007272 ) ;
#27227 = DIRECTION ( 'NONE',  ( 0.6184495258776511184, -0.3428121700606679978, -0.7071067811865504593 ) ) ;
#27228 = CARTESIAN_POINT ( 'NONE',  ( 49.98072202819530219, 26.36753733014356271, 47.19902993264913960 ) ) ;
#27229 = CARTESIAN_POINT ( 'NONE',  ( 48.40186567930498285, 26.72957786121581947, 45.03923535223908203 ) ) ;
#27230 = CIRCLE ( 'NONE', #13111, 12.36707279061065101 ) ;
#27231 = ORIENTED_EDGE ( 'NONE', *, *, #21792, .T. ) ;
#27232 = ORIENTED_EDGE ( 'NONE', *, *, #31273, .T. ) ;
#27233 = CYLINDRICAL_SURFACE ( 'NONE', #29599, 12.36707279061065101 ) ;
#27234 = ORIENTED_EDGE ( 'NONE', *, *, #14633, .T. ) ;
#27235 = DIRECTION ( 'NONE',  ( 0.000000000000000000, -1.000000000000000000, 0.000000000000000000 ) ) ;
#27236 = DIRECTION ( 'NONE',  ( -1.000000000000000000, -1.101824276508909887E-16, 0.000000000000000000 ) ) ;
#27237 = DIRECTION ( 'NONE',  ( -1.000000000000000000, -1.101824276508909764E-16, 0.000000000000000000 ) ) ;
#27238 = CARTESIAN_POINT ( 'NONE',  ( 44.70507715278255034, 26.26291119454915091, 46.92503878583765697 ) ) ;
#27239 = EDGE_CURVE ( 'NONE', #7227, #27529, #5272, .T. ) ;
#27240 = ORIENTED_EDGE ( 'NONE', *, *, #19461, .T. ) ;
#27241 = ORIENTED_EDGE ( 'NONE', *, *, #710, .F. ) ;
#27242 = CARTESIAN_POINT ( 'NONE',  ( 33.50134396954524618, 26.59164230456639899, 47.04930799450051637 ) ) ;
#27243 = CARTESIAN_POINT ( 'NONE',  ( 48.04075769285628894, 25.09624452788247950, 48.89770225776209855 ) ) ;
#27244 = CARTESIAN_POINT ( 'NONE',  ( 21.09992658989239089, 25.22145308207319303, 47.04930799450051637 ) ) ;
#27245 = ORIENTED_EDGE ( 'NONE', *, *, #1991, .F. ) ;
#27246 = CARTESIAN_POINT ( 'NONE',  ( 46.99023568444673060, 28.62451373492759643, 49.12151524109405898 ) ) ;
#27247 = CARTESIAN_POINT ( 'NONE',  ( 21.09992658989238734, 31.34143805560860585, 47.04930799450051637 ) ) ;
#27248 = ORIENTED_EDGE ( 'NONE', *, *, #6774, .T. ) ;
#27249 = FACE_OUTER_BOUND ( 'NONE', #14040, .T. ) ;
#27250 = DIRECTION ( 'NONE',  ( -1.000000000000000000, 0.000000000000000000, 0.000000000000000000 ) ) ;
#27251 = AXIS2_PLACEMENT_3D ( 'NONE', #21619, #24248, #13769 ) ;
#27252 = VECTOR ( 'NONE', #9906, 1000.000000000000000 ) ;
#27253 = DIRECTION ( 'NONE',  ( 0.000000000000000000, 9.698999007525574140E-17, 1.000000000000000000 ) ) ;
#27254 = AXIS2_PLACEMENT_3D ( 'NONE', #22719, #25662, #2851 ) ;
#27255 = EDGE_CURVE ( 'NONE', #8194, #23976, #12209, .T. ) ;
#27256 = VECTOR ( 'NONE', #24911, 1000.000000000000000 ) ;
#27257 = TOROIDAL_SURFACE ( 'NONE', #31464, 12.40141737965282687, 0.1250000000000004718 ) ;
#27258 = ADVANCED_FACE ( 'NONE', ( #24501 ), #4982, .T. ) ;
#27259 = ORIENTED_EDGE ( 'NONE', *, *, #5754, .F. ) ;
#27260 = ORIENTED_EDGE ( 'NONE', *, *, #26011, .T. ) ;
#27261 = CARTESIAN_POINT ( 'NONE',  ( -38.14261667679545553, -5.888571448818344933, 15.70117500735613447 ) ) ;
#27262 = EDGE_CURVE ( 'NONE', #9355, #6997, #9582, .T. ) ;
#27263 = DIRECTION ( 'NONE',  ( -1.000000000000000000, 0.000000000000000000, 0.000000000000000000 ) ) ;
#27264 = DIRECTION ( 'NONE',  ( -1.101824276508909887E-16, 1.000000000000000000, -0.000000000000000000 ) ) ;
#27265 = B_SPLINE_CURVE_WITH_KNOTS ( 'NONE', 3,
 ( #27195, #12610, #21939, #24745, #29840, #22601 ),
 .UNSPECIFIED., .F., .F.,
 ( 4, 2, 4 ),
 ( 0.000000000000000000, 0.5000000000000000000, 1.000000000000000000 ),
 .UNSPECIFIED. ) ;
#27266 = CONICAL_SURFACE ( 'NONE', #31468, 12.52247886585643499, 0.6248499269447925775 ) ;
#27267 = EDGE_CURVE ( 'NONE', #27795, #30194, #32389, .T. ) ;
#27268 = ORIENTED_EDGE ( 'NONE', *, *, #1202, .F. ) ;
#27269 = ADVANCED_FACE ( 'NONE', ( #22204 ), #9464, .T. ) ;
#27270 = CARTESIAN_POINT ( 'NONE',  ( 8.698509210239555145, 28.84164230456639544, 47.04930799450051637 ) ) ;
#27271 = FACE_OUTER_BOUND ( 'NONE', #14219, .T. ) ;
#27272 = DIRECTION ( 'NONE',  ( 0.4848096202463637039, 0.8746197071393810862, 0.000000000000000000 ) ) ;
#27273 = AXIS2_PLACEMENT_3D ( 'NONE', #7311, #24705, #9281 ) ;
#27274 = DIRECTION ( 'NONE',  ( -1.000000000000000000, 0.000000000000000000, 0.000000000000000000 ) ) ;
#27275 = DIRECTION ( 'NONE',  ( -1.101824276508909887E-16, 1.000000000000000000, -0.000000000000000000 ) ) ;
#27276 = DIRECTION ( 'NONE',  ( -0.000000000000000000, -1.000000000000000000, 0.000000000000000000 ) ) ;
#27277 = CARTESIAN_POINT ( 'NONE',  ( -37.12604442285837791, -13.74047052604243646, 43.23856262457184840 ) ) ;
#27278 = DIRECTION ( 'NONE',  ( -1.000000000000000000, 0.000000000000000000, 0.000000000000000000 ) ) ;
#27279 = CARTESIAN_POINT ( 'NONE',  ( -42.38687957179150345, 4.148162238788003719, 57.04930799450051637 ) ) ;
#27280 = SURFACE_STYLE_FILL_AREA ( #14330 ) ;
#27281 = CIRCLE ( 'NONE', #19398, 4.000000000000003553 ) ;
#27282 = EDGE_CURVE ( 'NONE', #7171, #17901, #8412, .T. ) ;
#27283 = PRESENTATION_STYLE_ASSIGNMENT (( #29098 ) ) ;
#27284 = EDGE_LOOP ( 'NONE', ( #431, #25640, #32011, #4692 ) ) ;
#27285 = ORIENTED_EDGE ( 'NONE', *, *, #14947, .F. ) ;
#27286 = CIRCLE ( 'NONE', #22490, 12.36707279061065279 ) ;
#27287 = DIRECTION ( 'NONE',  ( -1.000000000000000000, 0.000000000000000000, 0.000000000000000000 ) ) ;
#27288 = VECTOR ( 'NONE', #18481, 1000.000000000000000 ) ;
#27289 = CARTESIAN_POINT ( 'NONE',  ( 49.84415473660248352, 24.82319976284615137, 47.19193729663540893 ) ) ;
#27290 = CARTESIAN_POINT ( 'NONE',  ( -43.01732049266337299, 16.00634867709746700, 37.04930799450052348 ) ) ;
#27291 = CARTESIAN_POINT ( 'NONE',  ( 47.09785597605719687, 20.36454579224779948, 47.04930799450078638 ) ) ;
#27292 = ORIENTED_EDGE ( 'NONE', *, *, #4213, .F. ) ;
#27293 =( BOUNDED_CURVE ( )  B_SPLINE_CURVE ( 3, ( #23863, #26165, #29277, #8925 ),
 .UNSPECIFIED., .F., .F. ) 
 B_SPLINE_CURVE_WITH_KNOTS ( ( 4, 4 ),
 ( 1.575603059825828550E-14, 1.570796326794877462 ),
 .UNSPECIFIED. ) 
 CURVE ( )  GEOMETRIC_REPRESENTATION_ITEM ( )  RATIONAL_B_SPLINE_CURVE ( ( 1.000000000000000000, 0.8047378541243732641, 0.8047378541243732641, 1.000000000000000000 ) ) 
 REPRESENTATION_ITEM ( '' )  );
#27294 = LINE ( 'NONE', #4810, #14019 ) ;
#27295 = FACE_OUTER_BOUND ( 'NONE', #6325, .T. ) ;
#27296 = DIRECTION ( 'NONE',  ( -1.101824276508909887E-16, 1.000000000000000000, -0.000000000000000000 ) ) ;
#27297 = EDGE_LOOP ( 'NONE', ( #15303, #15314, #10173, #19874 ) ) ;
#27298 = EDGE_LOOP ( 'NONE', ( #22113, #31389, #15053, #11972 ) ) ;
#27299 = CARTESIAN_POINT ( 'NONE',  ( -39.58809650894544774, 2.596771453999702661, 47.04930799450051637 ) ) ;
#27300 = CARTESIAN_POINT ( 'NONE',  ( 46.00908685603034343, 29.03284706826092787, 44.91496614357595263 ) ) ;
#27301 = CARTESIAN_POINT ( 'NONE',  ( 8.732853799281732776, 23.72145308207319303, 47.04930799450051637 ) ) ;
#27302 = DIRECTION ( 'NONE',  ( 0.1949050434465252057, -0.6797146636928681485, -0.7071067811865469066 ) ) ;
#27303 = CARTESIAN_POINT ( 'NONE',  ( 71.77352134618342916, 10.95165879486606464, 22.29205552524197742 ) ) ;
#27304 = ORIENTED_EDGE ( 'NONE', *, *, #17256, .T. ) ;
#27305 = EDGE_CURVE ( 'NONE', #3234, #16288, #21504, .T. ) ;
#27306 = AXIS2_PLACEMENT_3D ( 'NONE', #29965, #19767, #16819 ) ;
#27307 = ADVANCED_FACE ( 'NONE', ( #24841 ), #7284, .T. ) ;
#27308 = ORIENTED_EDGE ( 'NONE', *, *, #3031, .T. ) ;
#27309 = VECTOR ( 'NONE', #11627, 1000.000000000000000 ) ;
#27310 = CIRCLE ( 'NONE', #18897, 2.000000000000001776 ) ;
#27311 = CIRCLE ( 'NONE', #24158, 0.1249999999999983763 ) ;
#27312 = DIRECTION ( 'NONE',  ( -0.9612616959383194493, -0.2756373558169974980, -8.795445018804946186E-19 ) ) ;
#27313 = AXIS2_PLACEMENT_3D ( 'NONE', #24537, #2055, #12077 ) ;
#27314 = EDGE_CURVE ( 'NONE', #8640, #17298, #8879, .T. ) ;
#27315 = EDGE_LOOP ( 'NONE', ( #25001, #6490, #24581, #15367 ) ) ;
#27316 = EDGE_CURVE ( 'NONE', #22063, #25801, #29441, .T. ) ;
#27317 = DIRECTION ( 'NONE',  ( -1.000000000000000000, 0.000000000000000000, 0.000000000000000000 ) ) ;
#27318 = DIRECTION ( 'NONE',  ( 1.000000000000000000, 0.000000000000000000, 0.000000000000000000 ) ) ;
#27319 = CIRCLE ( 'NONE', #28893, 1.000000000000000888 ) ;
#27320 = ORIENTED_EDGE ( 'NONE', *, *, #3110, .T. ) ;
#27321 = CARTESIAN_POINT ( 'NONE',  ( -40.86580004447909431, 8.503105189880379555, 34.64930799450051779 ) ) ;
#27322 = ORIENTED_EDGE ( 'NONE', *, *, #18011, .T. ) ;
#27323 = CARTESIAN_POINT ( 'NONE',  ( -41.89334324224038397, 13.85403361400641487, 59.48354556245477198 ) ) ;
#27324 = DIRECTION ( 'NONE',  ( -1.188208965918165239E-16, -1.880121038077813132E-16, -1.000000000000000000 ) ) ;
#27325 = ORIENTED_EDGE ( 'NONE', *, *, #8371, .F. ) ;
#27326 = CARTESIAN_POINT ( 'NONE',  ( 21.09992658989238734, 38.56284415653841791, 47.04930799450051637 ) ) ;
#27327 = DIRECTION ( 'NONE',  ( 0.9612616959383221138, 0.2756373558169876170, 0.000000000000000000 ) ) ;
#27328 = CARTESIAN_POINT ( 'NONE',  ( 33.50134396954524618, 26.84164230456639899, 47.04930799450051637 ) ) ;
#27329 = DIRECTION ( 'NONE',  ( 0.000000000000000000, 0.000000000000000000, -1.000000000000000000 ) ) ;
#27330 = DIRECTION ( 'NONE',  ( -1.101824276508909887E-16, 1.000000000000000000, -0.000000000000000000 ) ) ;
#27331 = CARTESIAN_POINT ( 'NONE',  ( 72.84780449950605430, 6.662067023026803092, 76.56641493775845220 ) ) ;
#27332 = EDGE_LOOP ( 'NONE', ( #16561, #7761, #15764, #17382 ) ) ;
#27333 = AXIS2_PLACEMENT_3D ( 'NONE', #20791, #8322, #30978 ) ;
#27334 = CARTESIAN_POINT ( 'NONE',  ( 21.09992658989239089, 25.71183152705960140, 47.04930799450051637 ) ) ;
#27335 = FACE_OUTER_BOUND ( 'NONE', #25736, .T. ) ;
#27336 = VERTEX_POINT ( 'NONE', #57 ) ;
#27337 = AXIS2_PLACEMENT_3D ( 'NONE', #5009, #19759, #32090 ) ;
#27338 = CARTESIAN_POINT ( 'NONE',  ( 21.09785597605720042, -16.03545420775220265, 47.04930799450051637 ) ) ;
#27339 = TOROIDAL_SURFACE ( 'NONE', #27853, 12.40141737965282509, 0.1249999999999980849 ) ;
#27340 = B_SPLINE_CURVE_WITH_KNOTS ( 'NONE', 3,
 ( #15097, #15738, #20979, #15906, #13452, #316, #476, #25271, #25752, #2783, #8044, #2937, #12808, #13130, #8518, #5733, #10982, #5900, #23447, #22952, #27897, #28219, #28382, #18511, #28541, #644, #18187, #25908, #6058, #10505, #22802, #3424, #23127, #18033, #10336, #960 ),
 .UNSPECIFIED., .F., .F.,
 ( 4, 2, 2, 2, 2, 2, 2, 2, 2, 2, 2, 2, 2, 2, 2, 2, 2, 4 ),
 ( 8.673617379884035472E-19, 0.001253900128824232598, 0.001880850193236362341, 0.002507800257648492518, 0.003134750322060622044, 0.003761700386472752872, 0.005015600515297014526, 0.005642550579709156196, 0.006269500644121296998, 0.007523400772945580336, 0.008777300901769865410, 0.01003120103059414875, 0.01253900128824272583, 0.01504680154589130639, 0.01630070167471558973, 0.01755460180353986960, 0.01880850193236414947, 0.02006240206118843281 ),
 .UNSPECIFIED. ) ;
#27341 = VECTOR ( 'NONE', #3872, 1000.000000000000000 ) ;
#27342 = DIRECTION ( 'NONE',  ( -0.6184495258776593340, 0.3428121700606657218, 0.7071067811865445751 ) ) ;
#27343 = VERTEX_POINT ( 'NONE', #215 ) ;
#27344 = VERTEX_POINT ( 'NONE', #20714 ) ;
#27345 = AXIS2_PLACEMENT_3D ( 'NONE', #25234, #2745, #20458 ) ;
#27346 = ORIENTED_EDGE ( 'NONE', *, *, #18868, .T. ) ;
#27347 = EDGE_CURVE ( 'NONE', #8513, #2319, #25329, .T. ) ;
#27348 = AXIS2_PLACEMENT_3D ( 'NONE', #26670, #14533, #31447 ) ;
#27349 = EDGE_CURVE ( 'NONE', #29185, #15519, #26222, .T. ) ;
#27350 = ADVANCED_FACE ( 'NONE', ( #10075 ), #15796, .T. ) ;
#27351 = VECTOR ( 'NONE', #9798, 1000.000000000000000 ) ;
#27352 = CARTESIAN_POINT ( 'NONE',  ( -9.880269301913145341, -5.935454207809699234, 107.5832060159989965 ) ) ;
#27353 = EDGE_LOOP ( 'NONE', ( #23121, #27139 ) ) ;
#27354 = EDGE_LOOP ( 'NONE', ( #30270, #30911, #30763, #9825 ) ) ;
#27355 = CARTESIAN_POINT ( 'NONE',  ( 78.88094405587852975, -5.913508961333113767, 15.68475707436527777 ) ) ;
#27356 = CARTESIAN_POINT ( 'NONE',  ( 45.84005119758191427, 10.95889540305195986, -4.518375277153177549 ) ) ;
#27357 = CARTESIAN_POINT ( 'NONE',  ( -44.28695544631906955, -5.935454207752198563, 54.04930799450053058 ) ) ;
#27358 = DIRECTION ( 'NONE',  ( 0.8746197071393926326, -0.4848096202463430537, -8.676864087101709653E-18 ) ) ;
#27359 = CARTESIAN_POINT ( 'NONE',  ( 21.09992658989239089, 24.59184655352419213, 47.04930799450051637 ) ) ;
#27360 = EDGE_LOOP ( 'NONE', ( #17785, #19175, #14762, #19368 ) ) ;
#27361 = CARTESIAN_POINT ( 'NONE',  ( -38.38918381122095980, -5.922340440260644101, 78.18162856751085599 ) ) ;
#27362 = ORIENTED_EDGE ( 'NONE', *, *, #8574, .F. ) ;
#27363 = DIRECTION ( 'NONE',  ( -1.000000000000000000, 0.000000000000000000, 0.000000000000000000 ) ) ;
#27364 = DIRECTION ( 'NONE',  ( 0.000000000000000000, 0.000000000000000000, -1.000000000000000000 ) ) ;
#27365 = AXIS2_PLACEMENT_3D ( 'NONE', #22390, #12240, #32422 ) ;
#27366 = ORIENTED_EDGE ( 'NONE', *, *, #5799, .T. ) ;
#27367 = CARTESIAN_POINT ( 'NONE',  ( 21.09992658989239089, 24.84143805560860940, 47.04930799450051637 ) ) ;
#27368 = FACE_OUTER_BOUND ( 'NONE', #16231, .T. ) ;
#27369 = CARTESIAN_POINT ( 'NONE',  ( 8.482002859293418240, 26.21664230456639899, 47.04930799450051637 ) ) ;
#27370 = CARTESIAN_POINT ( 'NONE',  ( 21.09992658989239089, 29.46664230456640254, 47.04930799450051637 ) ) ;
#27371 = DIRECTION ( 'NONE',  ( -1.101824276508909887E-16, 1.000000000000000000, -0.000000000000000000 ) ) ;
#27372 = AXIS2_PLACEMENT_3D ( 'NONE', #16012, #26789, #19719 ) ;
#27373 = CARTESIAN_POINT ( 'NONE',  ( 46.00908685603034343, 28.24624452788248163, 44.91496614357594552 ) ) ;
#27374 = DIRECTION ( 'NONE',  ( -0.000000000000000000, 1.000000000000000000, -0.000000000000000000 ) ) ;
#27375 = DIRECTION ( 'NONE',  ( 0.4544104193609900810, 0.000000000000000000, 0.8907924397839089847 ) ) ;
#27376 = ORIENTED_EDGE ( 'NONE', *, *, #13503, .F. ) ;
#27377 = DIRECTION ( 'NONE',  ( 0.000000000000000000, -1.000000000000000000, 0.000000000000000000 ) ) ;
#27378 = DIRECTION ( 'NONE',  ( -0.000000000000000000, -1.000000000000000000, 0.000000000000000000 ) ) ;
#27379 = ORIENTED_EDGE ( 'NONE', *, *, #20154, .T. ) ;
#27380 = AXIS2_PLACEMENT_3D ( 'NONE', #30039, #15414, #7552 ) ;
#27381 = DIRECTION ( 'NONE',  ( 0.000000000000000000, -0.000000000000000000, -1.000000000000000000 ) ) ;
#27382 = ORIENTED_EDGE ( 'NONE', *, *, #15866, .T. ) ;
#27383 = AXIS2_PLACEMENT_3D ( 'NONE', #451, #7528, #27874 ) ;
#27384 = ORIENTED_EDGE ( 'NONE', *, *, #18845, .F. ) ;
#27385 = DIRECTION ( 'NONE',  ( 0.6797146636928662611, 0.1949050434465333104, -0.7071067811865466846 ) ) ;
#27386 = VERTEX_POINT ( 'NONE', #25802 ) ;
#27387 = EDGE_CURVE ( 'NONE', #23768, #11676, #5622, .T. ) ;
#27388 = B_SPLINE_CURVE_WITH_KNOTS ( 'NONE', 3,
 ( #23482, #3291, #8231, #6087 ),
 .UNSPECIFIED., .F., .F.,
 ( 4, 4 ),
 ( 0.000000000000000000, 1.000000000000000000 ),
 .UNSPECIFIED. ) ;
#27389 = EDGE_CURVE ( 'NONE', #2185, #10889, #8096, .T. ) ;
#27390 = VECTOR ( 'NONE', #23487, 1000.000000000000000 ) ;
#27391 = EDGE_CURVE ( 'NONE', #28369, #15187, #25181, .T. ) ;
#27392 = ORIENTED_EDGE ( 'NONE', *, *, #14827, .T. ) ;
#27393 = EDGE_CURVE ( 'NONE', #11333, #22659, #10234, .T. ) ;
#27394 = CIRCLE ( 'NONE', #3812, 56.65825807113184709 ) ;
#27395 = EDGE_CURVE ( 'NONE', #2451, #25827, #697, .T. ) ;
#27396 = LINE ( 'NONE', #2921, #23848 ) ;
#27397 = DIRECTION ( 'NONE',  ( -1.101824276508909887E-16, 1.000000000000000000, -0.000000000000000000 ) ) ;
#27398 = TOROIDAL_SURFACE ( 'NONE', #22132, 4.099999999999999645, 0.1000000000000002554 ) ;
#27399 = EDGE_LOOP ( 'NONE', ( #9150, #24919, #1441, #19741 ) ) ;
#27400 = CIRCLE ( 'NONE', #18492, 12.36707279061065101 ) ;
#27401 = DIRECTION ( 'NONE',  ( 0.8746197071393858602, -0.4848096202463547666, 0.000000000000000000 ) ) ;
#27402 = CARTESIAN_POINT ( 'NONE',  ( -9.899862315945510360, -5.936215030417555383, -13.38459389407276134 ) ) ;
#27403 = CARTESIAN_POINT ( 'NONE',  ( 48.94625023931840957, 27.37124452788248874, 46.10640627770150246 ) ) ;
#27404 = EDGE_LOOP ( 'NONE', ( #26361, #23240, #11583, #23268 ) ) ;
#27405 = ORIENTED_EDGE ( 'NONE', *, *, #7947, .F. ) ;
#27406 = DIRECTION ( 'NONE',  ( -1.101824276508909887E-16, 1.000000000000000000, -0.000000000000000000 ) ) ;
#27407 = ORIENTED_EDGE ( 'NONE', *, *, #26387, .T. ) ;
#27408 = DIRECTION ( 'NONE',  ( -0.6184495258776542270, 0.3428121700606624467, -0.7071067811865504593 ) ) ;
#27409 = DIRECTION ( 'NONE',  ( -2.779292025043186357E-18, 1.288349127009862211E-17, -1.000000000000000000 ) ) ;
#27410 = DIRECTION ( 'NONE',  ( 1.000000000000000000, -3.759183808608825436E-15, 0.000000000000000000 ) ) ;
#27411 = PRODUCT_DEFINITION_SHAPE ( 'NONE', 'NONE',  #32498 ) ;
#27412 = LINE ( 'NONE', #30364, #10079 ) ;
#27413 = APPLICATION_PROTOCOL_DEFINITION ( 'draft international standard', 'automotive_design', 1998, #3625 ) ;
#27414 = ORIENTED_EDGE ( 'NONE', *, *, #10409, .F. ) ;
#27415 = ORIENTED_EDGE ( 'NONE', *, *, #2442, .F. ) ;
#27416 = DIRECTION ( 'NONE',  ( -1.000000000000000000, 0.000000000000000000, 0.000000000000000000 ) ) ;
#27417 = CARTESIAN_POINT ( 'NONE',  ( -40.70508238852949745, 9.491303552449114278, 38.64930799450052490 ) ) ;
#27418 = DIRECTION ( 'NONE',  ( 0.000000000000000000, 0.000000000000000000, -1.000000000000000000 ) ) ;
#27419 = AXIS2_PLACEMENT_3D ( 'NONE', #14741, #27693, #22764 ) ;
#27420 = EDGE_LOOP ( 'NONE', ( #27608, #6559, #12987, #6234 ) ) ;
#27421 = CARTESIAN_POINT ( 'NONE',  ( 44.70507715278255034, 27.74951373492759288, 46.92503878583765697 ) ) ;
#27422 = CIRCLE ( 'NONE', #7507, 12.62506659569710266 ) ;
#27423 = ORIENTED_EDGE ( 'NONE', *, *, #18843, .T. ) ;
#27424 = CARTESIAN_POINT ( 'NONE',  ( -42.36334586133936853, 13.70277685985800531, 59.47272913308562181 ) ) ;
#27425 = CARTESIAN_POINT ( 'NONE',  ( -40.57861772207635198, 7.624524047285948569, 53.95737344240558286 ) ) ;
#27426 = EDGE_CURVE ( 'NONE', #22918, #11299, #13124, .T. ) ;
#27427 = FACE_OUTER_BOUND ( 'NONE', #9407, .T. ) ;
#27428 = AXIS2_PLACEMENT_3D ( 'NONE', #11237, #18758, #30622 ) ;
#27429 = CIRCLE ( 'NONE', #7521, 0.1999999999999987899 ) ;
#27430 = ORIENTED_EDGE ( 'NONE', *, *, #3935, .T. ) ;
#27431 = EDGE_CURVE ( 'NONE', #11299, #22918, #6288, .T. ) ;
#27432 = ORIENTED_EDGE ( 'NONE', *, *, #31312, .T. ) ;
#27433 = ADVANCED_FACE ( 'NONE', ( #8250 ), #10498, .T. ) ;
#27434 = DIRECTION ( 'NONE',  ( 0.8746197071393926326, -0.4848096202463430537, -8.676864087101709653E-18 ) ) ;
#27435 = LINE ( 'NONE', #12511, #27613 ) ;
#27436 = CARTESIAN_POINT ( 'NONE',  ( 47.20547626766766314, 26.87451373492759643, 44.97710074790751378 ) ) ;
#27437 = ORIENTED_EDGE ( 'NONE', *, *, #24016, .F. ) ;
#27438 = VECTOR ( 'NONE', #28349, 1000.000000000000000 ) ;
#27439 = CYLINDRICAL_SURFACE ( 'NONE', #19645, 12.36707279061065101 ) ;
#27441 = CARTESIAN_POINT ( 'NONE',  ( -42.46007270772396680, 14.70100007970371792, 55.14582903391912083 ) ) ;
#27440 = CIRCLE ( 'NONE', #10612, 0.1000000000000011019 ) ;
#27442 = DIRECTION ( 'NONE',  ( -0.000000000000000000, 1.000000000000000000, -0.000000000000000000 ) ) ;
#27443 = DIRECTION ( 'NONE',  ( -1.000000000000000000, 0.000000000000000000, 0.000000000000000000 ) ) ;
#27444 = DIRECTION ( 'NONE',  ( 0.8746197071393858602, -0.4848096202463547666, 0.000000000000000000 ) ) ;
#27445 = AXIS2_PLACEMENT_3D ( 'NONE', #22236, #7647, #15186 ) ;
#27447 = AXIS2_PLACEMENT_3D ( 'NONE', #23443, #954, #3574 ) ;
#27446 = DIRECTION ( 'NONE',  ( -1.000000000000000000, 0.000000000000000000, 0.000000000000000000 ) ) ;
#27448 = CARTESIAN_POINT ( 'NONE',  ( 21.09785597605719332, -8.874820941924726370, 47.04930799450051637 ) ) ;
#27449 = VECTOR ( 'NONE', #3797, 1000.000000000000000 ) ;
#27450 = TOROIDAL_SURFACE ( 'NONE', #31640, 12.61792373059894778, 0.1249999999999986539 ) ;
#27451 = DIRECTION ( 'NONE',  ( -1.141485058121273361E-16, -2.056979540075764649E-16, -1.000000000000000000 ) ) ;
#27452 = DIRECTION ( 'NONE',  ( 0.000000000000000000, -1.000000000000000000, 0.000000000000000000 ) ) ;
#27453 =( NAMED_UNIT ( * ) PLANE_ANGLE_UNIT ( ) SI_UNIT ( $, .RADIAN. ) );
#27454 = ORIENTED_EDGE ( 'NONE', *, *, #4109, .F. ) ;
#27455 = ORIENTED_EDGE ( 'NONE', *, *, #12400, .F. ) ;
#27456 = CARTESIAN_POINT ( 'NONE',  ( -42.38687957179149635, 4.148162238788000167, 35.04930799450051637 ) ) ;
#27457 = CYLINDRICAL_SURFACE ( 'NONE', #13026, 12.36707279061065101 ) ;
#27458 = EDGE_CURVE ( 'NONE', #21709, #23463, #8909, .T. ) ;
#27459 = CARTESIAN_POINT ( 'NONE',  ( -63.90214402394282445, -3.935454207752190126, 42.04930799450051637 ) ) ;
#27460 = CARTESIAN_POINT ( 'NONE',  ( 49.98072202819530219, 27.06753733014356555, 47.19902993264913960 ) ) ;
#27461 = ORIENTED_EDGE ( 'NONE', *, *, #31668, .T. ) ;
#27462 = DIRECTION ( 'NONE',  ( -0.2756373558169956106, 0.9612616959383200044, 8.829587629302095151E-15 ) ) ;
#27463 = DIRECTION ( 'NONE',  ( 0.000000000000000000, -1.000000000000000000, 0.000000000000000000 ) ) ;
#27464 = CARTESIAN_POINT ( 'NONE',  ( 44.24821932555909854, 11.56063108660457495, -4.010480718324124005 ) ) ;
#27465 = ORIENTED_EDGE ( 'NONE', *, *, #30846, .F. ) ;
#27466 = ORIENTED_EDGE ( 'NONE', *, *, #21810, .T. ) ;
#27467 = CARTESIAN_POINT ( 'NONE',  ( -39.39739818181173803, -5.936352567920400780, 77.94940154167748858 ) ) ;
#27468 = EDGE_CURVE ( 'NONE', #3119, #1392, #19400, .T. ) ;
#27469 = ADVANCED_FACE ( 'NONE', ( #15154 ), #16775, .F. ) ;
#27470 = LINE ( 'NONE', #7615, #26737 ) ;
#27471 = DIRECTION ( 'NONE',  ( -1.101824276508909887E-16, 1.000000000000000000, -0.000000000000000000 ) ) ;
#27472 = VECTOR ( 'NONE', #27001, 1000.000000000000000 ) ;
#27473 = CARTESIAN_POINT ( 'NONE',  ( 45.50224332293416296, 29.25496114406801951, 45.23743444292109217 ) ) ;
#27474 = ORIENTED_EDGE ( 'NONE', *, *, #28798, .T. ) ;
#27475 = ORIENTED_EDGE ( 'NONE', *, *, #13601, .F. ) ;
#27476 = EDGE_CURVE ( 'NONE', #19635, #9965, #30743, .T. ) ;
#27477 = DIRECTION ( 'NONE',  ( -1.101824276508909887E-16, 1.000000000000000000, -0.000000000000000000 ) ) ;
#27478 = ORIENTED_EDGE ( 'NONE', *, *, #20971, .T. ) ;
#27479 = FACE_OUTER_BOUND ( 'NONE', #31353, .T. ) ;
#27480 = CARTESIAN_POINT ( 'NONE',  ( -9.831337038036075171, -5.937394935145314356, 107.4930705127871704 ) ) ;
#27481 = VERTEX_POINT ( 'NONE', #5141 ) ;
#27482 = PLANE ( 'NONE',  #5551 ) ;
#27483 = EDGE_LOOP ( 'NONE', ( #1386, #30970, #19159, #8987 ) ) ;
#27484 = DIRECTION ( 'NONE',  ( 1.000000000000000000, -3.759183808608825436E-15, 0.000000000000000000 ) ) ;
#27485 = FACE_OUTER_BOUND ( 'NONE', #24097, .T. ) ;
#27486 = AXIS2_PLACEMENT_3D ( 'NONE', #29741, #7584, #19548 ) ;
#27487 =( BOUNDED_CURVE ( )  B_SPLINE_CURVE ( 3, ( #27189, #22266, #27528, #2900 ),
 .UNSPECIFIED., .F., .F. ) 
 B_SPLINE_CURVE_WITH_KNOTS ( ( 4, 4 ),
 ( -8.881784197001252323E-16, 1.570796326794894338 ),
 .UNSPECIFIED. ) 
 CURVE ( )  GEOMETRIC_REPRESENTATION_ITEM ( )  RATIONAL_B_SPLINE_CURVE ( ( 1.000000000000000000, 0.8047378541243652705, 0.8047378541243652705, 1.000000000000000000 ) ) 
 REPRESENTATION_ITEM ( '' )  );
#27488 = EDGE_CURVE ( 'NONE', #31589, #27037, #23064, .T. ) ;
#27489 = DIRECTION ( 'NONE',  ( 0.000000000000000000, 0.000000000000000000, 1.000000000000000000 ) ) ;
#27490 = AXIS2_PLACEMENT_3D ( 'NONE', #6161, #21246, #13406 ) ;
#27491 = CARTESIAN_POINT ( 'NONE',  ( 21.09785597605720042, -13.37218737171702543, -8.638398481670979123 ) ) ;
#27492 = ORIENTED_EDGE ( 'NONE', *, *, #25091, .T. ) ;
#27493 = DIRECTION ( 'NONE',  ( -1.000000000000000000, 0.000000000000000000, 0.000000000000000000 ) ) ;
#27494 = FACE_OUTER_BOUND ( 'NONE', #3166, .T. ) ;
#27495 = AXIS2_PLACEMENT_3D ( 'NONE', #28936, #1676, #22012 ) ;
#27496 = DIRECTION ( 'NONE',  ( 0.000000000000000000, 0.000000000000000000, -1.000000000000000000 ) ) ;
#27497 = ADVANCED_FACE ( 'NONE', ( #11351 ), #21479, .T. ) ;
#27498 = DIRECTION ( 'NONE',  ( -1.000000000000000000, 0.000000000000000000, 0.000000000000000000 ) ) ;
#27499 = SPHERICAL_SURFACE ( 'NONE', #8968, 0.1000000000000000056 ) ;
#27500 = VERTEX_POINT ( 'NONE', #28920 ) ;
#27501 = DIRECTION ( 'NONE',  ( 0.000000000000000000, 0.000000000000000000, -1.000000000000000000 ) ) ;
#27502 = DIRECTION ( 'NONE',  ( -1.224646799147353207E-16, -1.349345573449484691E-32, 1.000000000000000000 ) ) ;
#27503 = ORIENTED_EDGE ( 'NONE', *, *, #1512, .T. ) ;
#27504 = CARTESIAN_POINT ( 'NONE',  ( -45.71589853820119487, -5.927381377935135198, 53.84747426841368423 ) ) ;
#27505 = EDGE_CURVE ( 'NONE', #17800, #19067, #26287, .T. ) ;
#27506 = CARTESIAN_POINT ( 'NONE',  ( 21.09785597605719332, 48.06454579224779877, 28.00041321616355461 ) ) ;
#27507 = EDGE_CURVE ( 'NONE', #9841, #16253, #10956, .T. ) ;
#27508 = ORIENTED_EDGE ( 'NONE', *, *, #15044, .T. ) ;
#27509 = LINE ( 'NONE', #30141, #32461 ) ;
#27510 = ORIENTED_EDGE ( 'NONE', *, *, #20528, .F. ) ;
#27511 = ORIENTED_EDGE ( 'NONE', *, *, #11315, .T. ) ;
#27512 = CIRCLE ( 'NONE', #13369, 2.000000000000001776 ) ;
#27513 = AXIS2_PLACEMENT_3D ( 'NONE', #24566, #4880, #32293 ) ;
#27514 = AXIS2_PLACEMENT_3D ( 'NONE', #17832, #7174, #27363 ) ;
#27515 = TOROIDAL_SURFACE ( 'NONE', #3918, 12.78419020052701960, 0.2000000000000000944 ) ;
#27516 = DIRECTION ( 'NONE',  ( 0.000000000000000000, -0.000000000000000000, -1.000000000000000000 ) ) ;
#27517 = ORIENTED_EDGE ( 'NONE', *, *, #29577, .T. ) ;
#27518 = ORIENTED_EDGE ( 'NONE', *, *, #20041, .T. ) ;
#27519 = CARTESIAN_POINT ( 'NONE',  ( -43.42682711710880739, 1.034448000281938285, 39.44930799450052916 ) ) ;
#27520 = CARTESIAN_POINT ( 'NONE',  ( -40.11286833322908052, 2.887657226147511302, 58.94930799450051495 ) ) ;
#27521 = DIRECTION ( 'NONE',  ( -1.000000000000000000, 0.000000000000000000, 0.000000000000000000 ) ) ;
#27522 = ADVANCED_FACE ( 'NONE', ( #13501 ), #5792, .T. ) ;
#27523 = CARTESIAN_POINT ( 'NONE',  ( 21.09992658989238734, 38.56284415653841791, 47.04930799450051637 ) ) ;
#27524 = VERTEX_POINT ( 'NONE', #13982 ) ;
#27525 = CARTESIAN_POINT ( 'NONE',  ( -9.949026574332460626, 4.272108154687138892, 98.50954949487454826 ) ) ;
#27526 = EDGE_LOOP ( 'NONE', ( #4601, #17383, #19249, #26592 ) ) ;
#27527 = CARTESIAN_POINT ( 'NONE',  ( -34.35572742831690363, -2.950474395469078637, 13.32293284703904135 ) ) ;
#27528 = CARTESIAN_POINT ( 'NONE',  ( -41.13825658839732569, 9.453274076459845077, 35.59072935073783128 ) ) ;
#27529 = VERTEX_POINT ( 'NONE', #31543 ) ;
#27530 = DIRECTION ( 'NONE',  ( -0.000000000000000000, -1.000000000000000000, 0.000000000000000000 ) ) ;
#27531 = DIRECTION ( 'NONE',  ( -1.101824276508909887E-16, 1.000000000000000000, -0.000000000000000000 ) ) ;
#27532 = ADVANCED_FACE ( 'NONE', ( #11039 ), #27257, .T. ) ;
#27533 = DIRECTION ( 'NONE',  ( -1.101824276508909887E-16, 1.000000000000000000, -0.000000000000000000 ) ) ;
#27534 = DIRECTION ( 'NONE',  ( -1.000000000000000000, 0.000000000000000000, 0.000000000000000000 ) ) ;
#27535 = DIRECTION ( 'NONE',  ( -0.4848096202463636484, -0.8746197071393810862, 0.000000000000000000 ) ) ;
#27536 = CARTESIAN_POINT ( 'NONE',  ( 45.79384627280941089, 29.17957786121581520, 49.05938063676249072 ) ) ;
#27537 = CIRCLE ( 'NONE', #26467, 59.44168675549763492 ) ;
#27538 = DIRECTION ( 'NONE',  ( -1.000000000000000000, 0.000000000000000000, 0.000000000000000000 ) ) ;
#27539 = CARTESIAN_POINT ( 'NONE',  ( -42.35594856044747303, 14.62682725489516145, 60.54930799450051637 ) ) ;
#27540 = AXIS2_PLACEMENT_3D ( 'NONE', #19521, #2461, #22314 ) ;
#27541 = VERTEX_POINT ( 'NONE', #16103 ) ;
#27542 = CARTESIAN_POINT ( 'NONE',  ( 21.09785597605719332, 30.56554579224779644, 73.04930799450052348 ) ) ;
#27543 = CARTESIAN_POINT ( 'NONE',  ( -36.45222641229887017, 9.925589859889724309, 52.04930799450051637 ) ) ;
#27544 = CIRCLE ( 'NONE', #11281, 70.59901951359279337 ) ;
#27545 = VERTEX_POINT ( 'NONE', #31059 ) ;
#27546 = CIRCLE ( 'NONE', #4478, 65.96844849472888939 ) ;
#27547 = ADVANCED_FACE ( 'NONE', ( #1168 ), #3147, .F. ) ;
#27548 = VECTOR ( 'NONE', #12555, 1000.000000000000114 ) ;
#27549 = DIRECTION ( 'NONE',  ( 0.4848096202463429982, 0.8746197071393925215, 9.920727850371700117E-18 ) ) ;
#27550 = VERTEX_POINT ( 'NONE', #26117 ) ;
#27551 = ORIENTED_EDGE ( 'NONE', *, *, #13537, .T. ) ;
#27552 = DIRECTION ( 'NONE',  ( -1.224646799147353207E-16, -1.349345573449484691E-32, 1.000000000000000000 ) ) ;
#27553 = EDGE_LOOP ( 'NONE', ( #14625, #13863, #24128, #15842 ) ) ;
#27554 =( REPRESENTATION_RELATIONSHIP ('NONE','NONE', #20382, #5723 ) REPRESENTATION_RELATIONSHIP_WITH_TRANSFORMATION ( #1276 )SHAPE_REPRESENTATION_RELATIONSHIP( ) );
#27555 = ORIENTED_EDGE ( 'NONE', *, *, #31935, .T. ) ;
#27556 = CARTESIAN_POINT ( 'NONE',  ( 45.53481149911499415, 22.92747281079970278, 47.84664715514688282 ) ) ;
#27557 =( GEOMETRIC_REPRESENTATION_CONTEXT ( 3 ) GLOBAL_UNCERTAINTY_ASSIGNED_CONTEXT ( ( #938 ) ) GLOBAL_UNIT_ASSIGNED_CONTEXT ( ( #1682, #6613, #16606 ) ) REPRESENTATION_CONTEXT ( 'NONE', 'WORKASPACE' ) );
#27558 = AXIS2_PLACEMENT_3D ( 'NONE', #25307, #9559, #20211 ) ;
#27559 = ORIENTED_EDGE ( 'NONE', *, *, #16373, .F. ) ;
#27560 = CARTESIAN_POINT ( 'NONE',  ( 21.09785597605720753, -5.098646251524523443, 47.04930799450052348 ) ) ;
#27561 = DIRECTION ( 'NONE',  ( -1.000000000000000000, 0.000000000000000000, 0.000000000000000000 ) ) ;
#27562 = DIRECTION ( 'NONE',  ( 0.000000000000000000, 0.000000000000000000, -1.000000000000000000 ) ) ;
#27563 = CARTESIAN_POINT ( 'NONE',  ( 45.38854177497844944, 29.02622849631042712, 45.94041160078741370 ) ) ;
#27564 = ORIENTED_EDGE ( 'NONE', *, *, #11607, .T. ) ;
#27565 = ORIENTED_EDGE ( 'NONE', *, *, #10195, .T. ) ;
#27566 = CARTESIAN_POINT ( 'NONE',  ( 21.09992658989239089, 29.34184655352418858, 47.04930799450051637 ) ) ;
#27567 = ORIENTED_EDGE ( 'NONE', *, *, #3782, .T. ) ;
#27568 = VECTOR ( 'NONE', #28162, 1000.000000000000000 ) ;
#27569 = DIRECTION ( 'NONE',  ( -0.000000000000000000, -1.000000000000000000, 0.000000000000000000 ) ) ;
#27570 = DIRECTION ( 'NONE',  ( -1.000000000000000000, -1.101824276508909887E-16, 0.000000000000000000 ) ) ;
#27571 = CARTESIAN_POINT ( 'NONE',  ( 46.82137942583813128, 14.98691807112498964, 46.50732389770341513 ) ) ;
#27572 = DIRECTION ( 'NONE',  ( -0.000000000000000000, -1.000000000000000000, 0.000000000000000000 ) ) ;
#27573 = FACE_OUTER_BOUND ( 'NONE', #10748, .T. ) ;
#27574 = PRODUCT_CONTEXT ( 'NONE', #705, 'mechanical' ) ;
#27575 = VERTEX_POINT ( 'NONE', #25956 ) ;
#27576 = ORIENTED_EDGE ( 'NONE', *, *, #10967, .T. ) ;
#27577 = CARTESIAN_POINT ( 'NONE',  ( 8.732853799281738105, 26.71183152705960495, 47.04930799450051637 ) ) ;
#27578 = CARTESIAN_POINT ( 'NONE',  ( 21.09992658989238734, 38.56284415653841791, 47.04930799450051637 ) ) ;
#27579 = EDGE_CURVE ( 'NONE', #665, #17919, #25697, .T. ) ;
#27580 = FACE_OUTER_BOUND ( 'NONE', #17715, .T. ) ;
#27581 = ADVANCED_FACE ( 'NONE', ( #11506, #21503 ), #9049, .F. ) ;
#27582 = EDGE_LOOP ( 'NONE', ( #12479, #31959, #7496, #13296 ) ) ;
#27583 = CARTESIAN_POINT ( 'NONE',  ( 45.79384627280941089, 29.26618040159426215, 49.05938063676249072 ) ) ;
#27584 = ORIENTED_EDGE ( 'NONE', *, *, #5746, .T. ) ;
#27585 = DIRECTION ( 'NONE',  ( 0.1949050434465283144, -0.6797146636928682595, -0.7071067811865461294 ) ) ;
#27586 = DIRECTION ( 'NONE',  ( -1.101824276508909887E-16, 1.000000000000000000, -0.000000000000000000 ) ) ;
#27587 = AXIS2_PLACEMENT_3D ( 'NONE', #14787, #32184, #30049 ) ;
#27588 = COLOUR_RGB ( '',0.7921568627450980005, 0.8196078431372548767, 0.9333333333333333481 ) ;
#27589 = DIRECTION ( 'NONE',  ( 0.000000000000000000, 1.000000000000000000, -9.698999007525574140E-17 ) ) ;
#27590 = VECTOR ( 'NONE', #31753, 1000.000000000000000 ) ;
#27591 = VERTEX_POINT ( 'NONE', #26601 ) ;
#27592 = ORIENTED_EDGE ( 'NONE', *, *, #14572, .F. ) ;
#27593 = DIRECTION ( 'NONE',  ( 0.4848096202463645921, 0.8746197071393805311, 0.000000000000000000 ) ) ;
#27594 = DIRECTION ( 'NONE',  ( 0.000000000000000000, 0.000000000000000000, -1.000000000000000000 ) ) ;
#27595 = CARTESIAN_POINT ( 'NONE',  ( 48.40186567930498285, 26.81618040159426641, 45.03923535223908203 ) ) ;
#27596 = ORIENTED_EDGE ( 'NONE', *, *, #26111, .F. ) ;
#27597 = CARTESIAN_POINT ( 'NONE',  ( -39.58809650894544774, 2.596771453999702661, 47.04930799450051637 ) ) ;
#27598 = CARTESIAN_POINT ( 'NONE',  ( 45.96182992765471909, 27.17822092656774302, 44.82232689504102296 ) ) ;
#27599 = EDGE_CURVE ( 'NONE', #19419, #31307, #3473, .T. ) ;
#27600 = LINE ( 'NONE', #12999, #20485 ) ;
#27601 = CARTESIAN_POINT ( 'NONE',  ( 44.21498992391908445, 27.41753733014355987, 46.89958605635242606 ) ) ;
#27602 = FACE_BOUND ( 'NONE', #18657, .T. ) ;
#27603 = CARTESIAN_POINT ( 'NONE',  ( -40.59710828457676968, 7.548125289910839975, 60.23404236618278418 ) ) ;
#27604 = PLANE ( 'NONE',  #26800 ) ;
#27605 = DIRECTION ( 'NONE',  ( -0.000000000000000000, -1.000000000000000000, -0.000000000000000000 ) ) ;
#27606 = CARTESIAN_POINT ( 'NONE',  ( -40.28779227465695811, 2.984619150196779813, 57.04930799450051637 ) ) ;
#27607 = DIRECTION ( 'NONE',  ( 0.4848096202463430537, 0.8746197071393926326, 1.323854077651070671E-16 ) ) ;
#27608 = ORIENTED_EDGE ( 'NONE', *, *, #9459, .T. ) ;
#27609 = VERTEX_POINT ( 'NONE', #23664 ) ;
#27610 = CARTESIAN_POINT ( 'NONE',  ( 21.09992658989239089, 30.09184655352422411, 47.04930799450051637 ) ) ;
#27611 = CARTESIAN_POINT ( 'NONE',  ( 48.80400426508809630, 25.05247065798242900, 45.18571335294186042 ) ) ;
#27612 = CARTESIAN_POINT ( 'NONE',  ( -33.97095292404057432, -3.671323332650886506, 13.46144832333910024 ) ) ;
#27613 = VECTOR ( 'NONE', #10042, 1000.000000000000000 ) ;
#27614 = ADVANCED_FACE ( 'NONE', ( #16267 ), #21026, .F. ) ;
#27615 = CARTESIAN_POINT ( 'NONE',  ( 54.55209231583086904, -4.032327822094588399, 102.4332369668683640 ) ) ;
#27616 = EDGE_CURVE ( 'NONE', #23429, #3682, #10145, .T. ) ;
#27617 = ADVANCED_FACE ( 'NONE', ( #6102 ), #19862, .T. ) ;
#27618 = ORIENTED_EDGE ( 'NONE', *, *, #18651, .T. ) ;
#27619 = DIRECTION ( 'NONE',  ( 0.000000000000000000, 0.000000000000000000, -1.000000000000000000 ) ) ;
#27620 = DIRECTION ( 'NONE',  ( 2.779292025043186357E-18, -1.288349127009862211E-17, 1.000000000000000000 ) ) ;
#27621 = DIRECTION ( 'NONE',  ( -1.101824276508909887E-16, 1.000000000000000000, -0.000000000000000000 ) ) ;
#27622 = VERTEX_POINT ( 'NONE', #17234 ) ;
#27623 = VERTEX_POINT ( 'NONE', #24630 ) ;
#27624 = CARTESIAN_POINT ( 'NONE',  ( 33.71785032049132269, 29.71664230456640254, 47.04930799450051637 ) ) ;
#27625 = ADVANCED_FACE ( 'NONE', ( #27249 ), #12332, .T. ) ;
#27626 = CARTESIAN_POINT ( 'NONE',  ( 47.20547626766766314, 26.17451373492760069, 44.97710074790751378 ) ) ;
#27627 = CARTESIAN_POINT ( 'NONE',  ( 44.86660686226233707, 22.74928388133296409, 45.96443597445600204 ) ) ;
#27628 = FACE_OUTER_BOUND ( 'NONE', #23074, .T. ) ;
#27629 = CARTESIAN_POINT ( 'NONE',  ( 8.474859994195282908, 38.56284415653841791, 47.04930799450051637 ) ) ;
#27630 = AXIS2_PLACEMENT_3D ( 'NONE', #10758, #8281, #18594 ) ;
#27631 = ORIENTED_EDGE ( 'NONE', *, *, #2349, .F. ) ;
#27632 = DIRECTION ( 'NONE',  ( -1.224646799147353207E-16, -1.349345573449484691E-32, 1.000000000000000000 ) ) ;
#27633 = ORIENTED_EDGE ( 'NONE', *, *, #14424, .T. ) ;
#27634 = DIRECTION ( 'NONE',  ( 0.000000000000000000, 0.000000000000000000, -1.000000000000000000 ) ) ;
#27635 = CARTESIAN_POINT ( 'NONE',  ( 41.51205063648687599, 11.92558985988973497, 99.04321908912902472 ) ) ;
#27636 = ADVANCED_FACE ( 'NONE', ( #21991 ), #26772, .T. ) ;
#27637 = EDGE_CURVE ( 'NONE', #13269, #4386, #29926, .T. ) ;
#27638 = ORIENTED_EDGE ( 'NONE', *, *, #19219, .F. ) ;
#27639 = CARTESIAN_POINT ( 'NONE',  ( 8.482002859293789498, 30.46664230456641675, 47.04930799450051637 ) ) ;
#27640 = ORIENTED_EDGE ( 'NONE', *, *, #8416, .T. ) ;
#27641 = AXIS2_PLACEMENT_3D ( 'NONE', #15930, #6407, #8708 ) ;
#27642 = CARTESIAN_POINT ( 'NONE',  ( 79.40776106085759523, -5.721341737285999152, 78.89649703355206611 ) ) ;
#27643 = CARTESIAN_POINT ( 'NONE',  ( 33.50134396954521065, 30.09164230456639544, 47.04930799450051637 ) ) ;
#27644 = AXIS2_PLACEMENT_3D ( 'NONE', #3802, #24147, #7083 ) ;
#27645 = DIRECTION ( 'NONE',  ( -0.000000000000000000, 1.000000000000000000, -0.000000000000000000 ) ) ;
#27646 = DIRECTION ( 'NONE',  ( -1.000000000000000000, 0.000000000000000000, 0.000000000000000000 ) ) ;
#27647 = VERTEX_POINT ( 'NONE', #4605 ) ;
#27648 = CARTESIAN_POINT ( 'NONE',  ( 78.57866796533406273, -5.769399297529532511, 78.79950972727095859 ) ) ;
#27650 = CARTESIAN_POINT ( 'NONE',  ( 8.823509210239548040, 28.09164230456639544, 47.04930799450051637 ) ) ;
#27649 = CIRCLE ( 'NONE', #7735, 84.21005050633887379 ) ;
#27651 = FACE_OUTER_BOUND ( 'NONE', #26852, .T. ) ;
#27652 = FACE_OUTER_BOUND ( 'NONE', #16217, .T. ) ;
#27653 = CARTESIAN_POINT ( 'NONE',  ( 75.28003531790183445, -0.7249253372052035793, 80.48926995870992585 ) ) ;
#27654 = ORIENTED_EDGE ( 'NONE', *, *, #19251, .T. ) ;
#27655 = FACE_OUTER_BOUND ( 'NONE', #23734, .T. ) ;
#27656 = DIRECTION ( 'NONE',  ( 0.000000000000000000, 0.000000000000000000, 1.000000000000000000 ) ) ;
#27657 = ORIENTED_EDGE ( 'NONE', *, *, #21747, .F. ) ;
#27658 = LINE ( 'NONE', #5180, #7873 ) ;
#27659 = EDGE_CURVE ( 'NONE', #27524, #27708, #15762, .T. ) ;
#27660 = FACE_OUTER_BOUND ( 'NONE', #8964, .T. ) ;
#27661 = CIRCLE ( 'NONE', #23988, 0.1000000000000006301 ) ;
#27662 = DIRECTION ( 'NONE',  ( -0.000000000000000000, -1.000000000000000000, -0.000000000000000000 ) ) ;
#27663 = ORIENTED_EDGE ( 'NONE', *, *, #14802, .T. ) ;
#27664 = B_SPLINE_SURFACE_WITH_KNOTS ( 'NONE', 3, 1, ( 
 ( #20243, #15167 ),
 ( #9920, #10091 ),
 ( #27969, #27480 ),
 ( #30268, #2526 ) ),
 .UNSPECIFIED., .F., .F., .F.,
 ( 4, 4 ),
 ( 2, 2 ),
 ( 0.1800733115436725096, 0.1889470565094412413 ),
 ( 0.000000000000000000, 1.000000000000000000 ),
 .UNSPECIFIED. ) ;
#27665 = DIRECTION ( 'NONE',  ( -1.101824276508909887E-16, 1.000000000000000000, -0.000000000000000000 ) ) ;
#27666 = ORIENTED_EDGE ( 'NONE', *, *, #24683, .F. ) ;
#27667 = ORIENTED_EDGE ( 'NONE', *, *, #16802, .T. ) ;
#27668 = EDGE_CURVE ( 'NONE', #663, #18077, #2316, .T. ) ;
#27669 = AXIS2_PLACEMENT_3D ( 'NONE', #30959, #5681, #18776 ) ;
#27670 = ADVANCED_FACE ( 'NONE', ( #4287 ), #16913, .F. ) ;
#27671 = AXIS2_PLACEMENT_3D ( 'NONE', #29683, #7188, #22434 ) ;
#27672 = FACE_OUTER_BOUND ( 'NONE', #764, .T. ) ;
#27673 = CARTESIAN_POINT ( 'NONE',  ( 44.87087493598345134, 25.95322093266652530, 48.18533415931919706 ) ) ;
#27674 = EDGE_CURVE ( 'NONE', #16169, #28880, #8356, .T. ) ;
#27675 = EDGE_CURVE ( 'NONE', #11329, #6385, #19869, .T. ) ;
#27676 = EDGE_LOOP ( 'NONE', ( #16951, #6720, #15554, #31839 ) ) ;
#27677 = AXIS2_PLACEMENT_3D ( 'NONE', #14811, #10209, #19714 ) ;
#27678 = EDGE_LOOP ( 'NONE', ( #8898, #19902 ) ) ;
#27679 = ADVANCED_FACE ( 'NONE', ( #32354 ), #2595, .F. ) ;
#27680 = CARTESIAN_POINT ( 'NONE',  ( -43.35833523721896654, -3.935454207752183020, 52.04930799450050927 ) ) ;
#27681 = CARTESIAN_POINT ( 'NONE',  ( 52.99971320245913375, -5.721341737285090545, 105.3293216028873616 ) ) ;
#27682 = DIRECTION ( 'NONE',  ( -1.101824276508909887E-16, 1.000000000000000000, -0.000000000000000000 ) ) ;
#27683 = ORIENTED_EDGE ( 'NONE', *, *, #13270, .T. ) ;
#27684 = DIRECTION ( 'NONE',  ( -1.000000000000000000, 0.000000000000000000, 0.000000000000000000 ) ) ;
#27685 = ORIENTED_EDGE ( 'NONE', *, *, #24278, .T. ) ;
#27686 = CARTESIAN_POINT ( 'NONE',  ( -33.89646034886494874, -2.243811656006899025, 13.32259206650234518 ) ) ;
#27687 = DIRECTION ( 'NONE',  ( 0.000000000000000000, 0.000000000000000000, 1.000000000000000000 ) ) ;
#27688 = ORIENTED_EDGE ( 'NONE', *, *, #26409, .F. ) ;
#27689 = DIRECTION ( 'NONE',  ( 0.000000000000000000, -0.000000000000000000, -1.000000000000000000 ) ) ;
#27690 = FACE_OUTER_BOUND ( 'NONE', #10500, .T. ) ;
#27691 = CARTESIAN_POINT ( 'NONE',  ( 21.09992658989239089, 29.46183152705961206, 47.04930799450051637 ) ) ;
#27692 = CARTESIAN_POINT ( 'NONE',  ( -42.21195563036362586, 4.051200314738734320, 59.04930799450051637 ) ) ;
#27693 = DIRECTION ( 'NONE',  ( -1.188208965918164993E-16, -1.880121038077812639E-16, -1.000000000000000000 ) ) ;
#27694 = CARTESIAN_POINT ( 'NONE',  ( 47.20547626766766314, 28.88791119454915091, 44.97710074790751378 ) ) ;
#27695 = LINE ( 'NONE', #14744, #7407 ) ;
#27696 = CARTESIAN_POINT ( 'NONE',  ( -39.50554051497144314, 7.696103224718195968, 61.94930799450052206 ) ) ;
#27697 = VERTEX_POINT ( 'NONE', #24306 ) ;
#27698 = EDGE_CURVE ( 'NONE', #7100, #9965, #4746, .T. ) ;
#27699 = CARTESIAN_POINT ( 'NONE',  ( 34.91272994418231690, 15.57592086119046826, 47.04930799450052348 ) ) ;
#27700 = AXIS2_PLACEMENT_3D ( 'NONE', #3803, #8577, #704 ) ;
#27701 = VERTEX_POINT ( 'NONE', #21677 ) ;
#27702 = VECTOR ( 'NONE', #22669, 1000.000000000000114 ) ;
#27703 = CIRCLE ( 'NONE', #19292, 12.36707279061065101 ) ;
#27704 = CARTESIAN_POINT ( 'NONE',  ( 21.09785597605720753, 13.86454579224779948, 47.04930799450052348 ) ) ;
#27705 = VECTOR ( 'NONE', #26801, 1000.000000000000227 ) ;
#27706 = ORIENTED_EDGE ( 'NONE', *, *, #2119, .F. ) ;
#27707 = VECTOR ( 'NONE', #24055, 1000.000000000000000 ) ;
#27708 = VERTEX_POINT ( 'NONE', #31700 ) ;
#27709 = CARTESIAN_POINT ( 'NONE',  ( -40.99628586177130529, 8.927770518203464789, 58.05249952744806308 ) ) ;
#27710 = TOROIDAL_SURFACE ( 'NONE', #13552, 12.40141737965283220, 0.1250000000000002498 ) ;
#27711 = ORIENTED_EDGE ( 'NONE', *, *, #4571, .F. ) ;
#27712 = ADVANCED_FACE ( 'NONE', ( #9545 ), #18883, .F. ) ;
#27713 = ADVANCED_FACE ( 'NONE', ( #21834 ), #12559, .T. ) ;
#27714 = EDGE_LOOP ( 'NONE', ( #28397, #25641, #10791, #708 ) ) ;
#27715 = LINE ( 'NONE', #4912, #21214 ) ;
#27716 = CIRCLE ( 'NONE', #18287, 21.50000000000000000 ) ;
#27717 = ADVANCED_FACE ( 'NONE', ( #4448 ), #12000, .F. ) ;
#27718 = CIRCLE ( 'NONE', #17238, 12.00000000000000355 ) ;
#27719 = ORIENTED_EDGE ( 'NONE', *, *, #19134, .F. ) ;
#27720 = ADVANCED_FACE ( 'NONE', ( #27091 ), #486, .T. ) ;
#27721 = TOROIDAL_SURFACE ( 'NONE', #24027, 55.78321279447762748, 0.1000000000000016986 ) ;
#27722 = FACE_OUTER_BOUND ( 'NONE', #8283, .T. ) ;
#27723 = CARTESIAN_POINT ( 'NONE',  ( 49.44967724995736091, 29.25019814131313822, 46.48227884171557633 ) ) ;
#27724 = CARTESIAN_POINT ( 'NONE',  ( 46.55854765242722948, 26.56960992152948364, 44.51792966461572831 ) ) ;
#27725 = CARTESIAN_POINT ( 'NONE',  ( 45.79384627280941089, 25.67957786121582231, 49.05938063676249072 ) ) ;
#27726 = ORIENTED_EDGE ( 'NONE', *, *, #22973, .T. ) ;
#27727 = VERTEX_POINT ( 'NONE', #12823 ) ;
#27728 = CARTESIAN_POINT ( 'NONE',  ( -42.47434154250544225, 4.196643200812637531, 57.04930799450051637 ) ) ;
#27729 = ORIENTED_EDGE ( 'NONE', *, *, #10584, .F. ) ;
#27730 = AXIS2_PLACEMENT_3D ( 'NONE', #29433, #14988, #17270 ) ;
#27731 = DIRECTION ( 'NONE',  ( -1.101824276508909887E-16, 1.000000000000000000, -0.000000000000000000 ) ) ;
#27732 = FACE_OUTER_BOUND ( 'NONE', #222, .T. ) ;
#27733 = DIRECTION ( 'NONE',  ( -1.000000000000000000, 0.000000000000000000, 0.000000000000000000 ) ) ;
#27734 = FACE_OUTER_BOUND ( 'NONE', #9502, .T. ) ;
#27735 = CARTESIAN_POINT ( 'NONE',  ( 47.20547626766764893, 25.38791119454915801, 44.97710074790751378 ) ) ;
#27736 = APPLICATION_PROTOCOL_DEFINITION ( 'draft international standard', 'automotive_design', 1998, #6357 ) ;
#27737 = EDGE_LOOP ( 'NONE', ( #29578, #8800, #10721, #23105 ) ) ;
#27738 = VERTEX_POINT ( 'NONE', #327 ) ;
#27739 = CARTESIAN_POINT ( 'NONE',  ( -4.902144023942810236, 30.56454579224779522, 49.54930799450042400 ) ) ;
#27740 = DIRECTION ( 'NONE',  ( -0.2756373558169954441, 0.9612616959383198934, -1.479773560108263204E-16 ) ) ;
#27741 = CARTESIAN_POINT ( 'NONE',  ( -9.833199634961228952, -5.936746300155038014, 107.4930292230181408 ) ) ;
#27742 = EDGE_LOOP ( 'NONE', ( #7786, #3434, #19751, #18366, #16644 ) ) ;
#27743 = CARTESIAN_POINT ( 'NONE',  ( 49.49063479933183629, 28.79951373492759359, 47.17357720316391578 ) ) ;
#27744 = ORIENTED_EDGE ( 'NONE', *, *, #29871, .T. ) ;
#27745 = CARTESIAN_POINT ( 'NONE',  ( 47.09785597605719687, 15.77906836436399374, 47.04930799450078638 ) ) ;
#27746 = DIRECTION ( 'NONE',  ( 0.6298853748009116682, 0.7071067811865470176, -0.3213166889719796249 ) ) ;
#27747 = AXIS2_PLACEMENT_3D ( 'NONE', #25221, #20124, #27181 ) ;
#27748 = CIRCLE ( 'NONE', #29321, 0.1250000000000018319 ) ;
#27749 = CARTESIAN_POINT ( 'NONE',  ( 21.09785597605720042, -16.03545420775220265, -23.54971151909227700 ) ) ;
#27750 = AXIS2_PLACEMENT_3D ( 'NONE', #28877, #26243, #6067 ) ;
#27751 = ORIENTED_EDGE ( 'NONE', *, *, #15247, .T. ) ;
#27752 = TOROIDAL_SURFACE ( 'NONE', #30380, 67.99999999999997158, 3.299999999999999822 ) ;
#27753 = EDGE_LOOP ( 'NONE', ( #23000, #12582 ) ) ;
#27754 = CARTESIAN_POINT ( 'NONE',  ( -40.28136326135769707, 8.248516754564388265, 59.50788663826320146 ) ) ;
#27755 = CARTESIAN_POINT ( 'NONE',  ( -44.62459984291964332, -4.794956837033497621, 52.23427270913660436 ) ) ;
#27756 = DIRECTION ( 'NONE',  ( -1.101824276508909887E-16, 1.000000000000000000, -0.000000000000000000 ) ) ;
#27757 = EDGE_CURVE ( 'NONE', #63, #12709, #4228, .T. ) ;
#27758 = ORIENTED_EDGE ( 'NONE', *, *, #998, .T. ) ;
#27759 = EDGE_CURVE ( 'NONE', #11910, #4901, #20920, .T. ) ;
#27760 = DIRECTION ( 'NONE',  ( 2.779292025043186357E-18, -1.288349127009862211E-17, 1.000000000000000000 ) ) ;
#27761 = DIRECTION ( 'NONE',  ( -1.224646799147353207E-16, -1.349345573449484691E-32, 1.000000000000000000 ) ) ;
#27762 = DIRECTION ( 'NONE',  ( 0.000000000000000000, -0.000000000000000000, -1.000000000000000000 ) ) ;
#27763 = CARTESIAN_POINT ( 'NONE',  ( 45.52675994804781112, 26.13420399681022843, 49.47108226228596806 ) ) ;
#27764 = VECTOR ( 'NONE', #12729, 1000.000000000000000 ) ;
#27765 = CYLINDRICAL_SURFACE ( 'NONE', #19153, 0.1000000000000007272 ) ;
#27766 = FACE_OUTER_BOUND ( 'NONE', #9302, .T. ) ;
#27767 = CYLINDRICAL_SURFACE ( 'NONE', #10638, 12.00000000000000355 ) ;
#27768 = CARTESIAN_POINT ( 'NONE',  ( -40.99628586177130529, 8.927770518203464789, 56.04611646155296256 ) ) ;
#27769 = DIRECTION ( 'NONE',  ( 0.000000000000000000, -1.000000000000000000, 0.000000000000000000 ) ) ;
#27770 = DIRECTION ( 'NONE',  ( -1.000000000000000000, 0.000000000000000000, 0.000000000000000000 ) ) ;
#27771 = CARTESIAN_POINT ( 'NONE',  ( 50.10320668408830613, 29.10621246473837331, 47.20539118556276037 ) ) ;
#27772 =( LENGTH_UNIT ( ) NAMED_UNIT ( * ) SI_UNIT ( .MILLI., .METRE. ) );
#27773 = VERTEX_POINT ( 'NONE', #30372 ) ;
#27774 = VERTEX_POINT ( 'NONE', #20512 ) ;
#27775 = DIRECTION ( 'NONE',  ( -0.000000000000000000, 1.000000000000000000, -0.000000000000000000 ) ) ;
#27776 = CARTESIAN_POINT ( 'NONE',  ( -43.84458661617622255, -0.1317431541793673277, 61.99930799450051921 ) ) ;
#27777 = DIRECTION ( 'NONE',  ( -1.224646799147353207E-16, -1.349345573449484691E-32, 1.000000000000000000 ) ) ;
#27778 = VECTOR ( 'NONE', #1694, 1000.000000000000000 ) ;
#27779 = AXIS2_PLACEMENT_3D ( 'NONE', #31260, #31419, #19244 ) ;
#27780 = CARTESIAN_POINT ( 'NONE',  ( 48.47771913120614329, 9.127627432390728046, 97.50908689856248657 ) ) ;
#27781 = ORIENTED_EDGE ( 'NONE', *, *, #15872, .F. ) ;
#27782 = CARTESIAN_POINT ( 'NONE',  ( -39.49588282908369763, -5.935567020298775809, 77.98014135999763141 ) ) ;
#27783 = VECTOR ( 'NONE', #20575, 1000.000000000000114 ) ;
#27784 = DIRECTION ( 'NONE',  ( -0.000000000000000000, -1.000000000000000000, 0.000000000000000000 ) ) ;
#27785 = FACE_OUTER_BOUND ( 'NONE', #22686, .T. ) ;
#27786 = ORIENTED_EDGE ( 'NONE', *, *, #19616, .F. ) ;
#27787 = ORIENTED_EDGE ( 'NONE', *, *, #15483, .F. ) ;
#27788 = DIRECTION ( 'NONE',  ( 0.000000000000000000, 0.000000000000000000, -1.000000000000000000 ) ) ;
#27789 = CARTESIAN_POINT ( 'NONE',  ( 44.70507715278255745, 27.04951373492760069, 46.92503878583765697 ) ) ;
#27790 = VECTOR ( 'NONE', #23701, 1000.000000000000114 ) ;
#27791 = CARTESIAN_POINT ( 'NONE',  ( -9.880269303432738681, -5.935454207752202116, -3.351769630585352377 ) ) ;
#27792 = DIRECTION ( 'NONE',  ( -1.000000000000000000, -1.101824276508910010E-16, 0.000000000000000000 ) ) ;
#27793 = DIRECTION ( 'NONE',  ( -1.000000000000000000, 0.000000000000000000, 0.000000000000000000 ) ) ;
#27794 = AXIS2_PLACEMENT_3D ( 'NONE', #6450, #19064, #29093 ) ;
#27795 = VERTEX_POINT ( 'NONE', #10688 ) ;
#27796 = B_SPLINE_CURVE_WITH_KNOTS ( 'NONE', 3,
 ( #2380, #14692, #24697, #30271, #72, #29955, #9767, #2696, #22220, #10095, #5004, #29784, #2848, #7299, #17299, #7470, #27812, #19756, #27321 ),
 .UNSPECIFIED., .F., .F.,
 ( 4, 3, 3, 3, 3, 3, 4 ),
 ( 0.000000000000000000, 2.676417781644011357E-05, 5.329639190753654004E-05, 9.120475318091182042E-05, 0.0001427884462350388043, 0.0001845748449448716228, 0.0001865811973795250859 ),
 .UNSPECIFIED. ) ;
#27797 = CARTESIAN_POINT ( 'NONE',  ( 56.59785597605721108, 14.86454579224779948, 47.04930799450051637 ) ) ;
#27798 = CIRCLE ( 'NONE', #6308, 12.36707279061065101 ) ;
#27799 = AXIS2_PLACEMENT_3D ( 'NONE', #2959, #10530, #5596 ) ;
#27800 = EDGE_LOOP ( 'NONE', ( #6621, #25200, #8086, #30089 ) ) ;
#27801 = ADVANCED_FACE ( 'NONE', ( #25122 ), #29854, .T. ) ;
#27802 = EDGE_CURVE ( 'NONE', #9593, #7848, #8211, .T. ) ;
#27803 = AXIS2_PLACEMENT_3D ( 'NONE', #3460, #26432, #13488 ) ;
#27804 = ADVANCED_FACE ( 'NONE', ( #10031 ), #15429, .T. ) ;
#27805 = CARTESIAN_POINT ( 'NONE',  ( 21.09785597605719332, -8.874820941924726370, 47.04930799450051637 ) ) ;
#27806 = DIRECTION ( 'NONE',  ( -0.2756373558170082672, 0.9612616959383162296, 0.000000000000000000 ) ) ;
#27807 = ADVANCED_FACE ( 'NONE', ( #8058 ), #8936, .T. ) ;
#27808 = CIRCLE ( 'NONE', #30435, 0.1250000000000001110 ) ;
#27809 = VECTOR ( 'NONE', #5471, 1000.000000000000114 ) ;
#27810 = VECTOR ( 'NONE', #28258, 1000.000000000000000 ) ;
#27811 = ORIENTED_EDGE ( 'NONE', *, *, #17618, .T. ) ;
#27812 = CARTESIAN_POINT ( 'NONE',  ( -40.86555073846352570, 8.502249289700491985, 34.64831079233957212 ) ) ;
#27813 = ORIENTED_EDGE ( 'NONE', *, *, #20161, .T. ) ;
#27814 = CYLINDRICAL_SURFACE ( 'NONE', #4725, 12.36707279061065279 ) ;
#27815 = CARTESIAN_POINT ( 'NONE',  ( -42.21195563036361875, 4.051200314738730768, 37.04930799450052348 ) ) ;
#27816 = DIRECTION ( 'NONE',  ( 0.4544104193609903586, 0.000000000000000000, 0.8907924397839087627 ) ) ;
#27817 = DIRECTION ( 'NONE',  ( -1.000000000000000000, 0.000000000000000000, 0.000000000000000000 ) ) ;
#27818 = ORIENTED_EDGE ( 'NONE', *, *, #18336, .T. ) ;
#27819 = DIRECTION ( 'NONE',  ( 0.000000000000000000, 0.000000000000000000, 1.000000000000000000 ) ) ;
#27820 = AXIS2_PLACEMENT_3D ( 'NONE', #7959, #13043, #20576 ) ;
#27821 = CARTESIAN_POINT ( 'NONE',  ( 81.55380775071134281, -5.936920032134864300, 77.94194987224879867 ) ) ;
#27822 = CARTESIAN_POINT ( 'NONE',  ( 33.37634396954522487, 28.59164230456639544, 47.04930799450051637 ) ) ;
#27823 = DIRECTION ( 'NONE',  ( 0.4848096202463673676, 0.8746197071393789768, 0.000000000000000000 ) ) ;
#27824 = ORIENTED_EDGE ( 'NONE', *, *, #9990, .F. ) ;
#27825 = DIRECTION ( 'NONE',  ( -1.000000000000000000, 0.000000000000000000, 0.000000000000000000 ) ) ;
#27826 = DIRECTION ( 'NONE',  ( 0.000000000000000000, 1.000000000000000000, -0.000000000000000000 ) ) ;
#27827 = ORIENTED_EDGE ( 'NONE', *, *, #29810, .T. ) ;
#27828 = CARTESIAN_POINT ( 'NONE',  ( 21.09992658989239089, 23.65414230456639544, 47.04930799450051637 ) ) ;
#27829 = CARTESIAN_POINT ( 'NONE',  ( 21.09992658989239089, 29.96664230456641675, 47.04930799450051637 ) ) ;
#27830 = CARTESIAN_POINT ( 'NONE',  ( -29.27337757263006424, -4.281489722201563985, 13.63563177263803894 ) ) ;
#27831 = AXIS2_PLACEMENT_3D ( 'NONE', #22068, #6981, #24215 ) ;
#27832 = CYLINDRICAL_SURFACE ( 'NONE', #24771, 2.500000000000002220 ) ;
#27833 = EDGE_LOOP ( 'NONE', ( #25711, #27881, #30582, #15378 ) ) ;
#27834 = DIRECTION ( 'NONE',  ( -0.9612616959383205595, -0.2756373558169932236, 1.660411357259282445E-16 ) ) ;
#27835 = AXIS2_PLACEMENT_3D ( 'NONE', #17677, #19809, #27538 ) ;
#27836 = ORIENTED_EDGE ( 'NONE', *, *, #26756, .F. ) ;
#27837 = AXIS2_PLACEMENT_3D ( 'NONE', #24734, #27682, #2249 ) ;
#27838 = EDGE_CURVE ( 'NONE', #21395, #4349, #28358, .T. ) ;
#27839 = CIRCLE ( 'NONE', #23631, 0.1999999999999918510 ) ;
#27840 = VERTEX_POINT ( 'NONE', #12979 ) ;
#27841 = CARTESIAN_POINT ( 'NONE',  ( -40.06561427811386267, 7.496110634155836117, 60.44930799450051495 ) ) ;
#27842 = DIRECTION ( 'NONE',  ( -1.000000000000000000, 0.000000000000000000, 0.000000000000000000 ) ) ;
#27843 = EDGE_CURVE ( 'NONE', #19672, #15022, #8428, .T. ) ;
#27844 = EDGE_LOOP ( 'NONE', ( #14711, #22075, #22881, #32377 ) ) ;
#27845 = ORIENTED_EDGE ( 'NONE', *, *, #5634, .F. ) ;
#27846 = DIRECTION ( 'NONE',  ( -1.101824276508909887E-16, 1.000000000000000000, -0.000000000000000000 ) ) ;
#27847 = CIRCLE ( 'NONE', #3714, 12.27641737965280555 ) ;
#27848 = DIRECTION ( 'NONE',  ( 0.1949050434465325055, -0.6797146636928671493, 0.7071067811865460184 ) ) ;
#27849 = LINE ( 'NONE', #30643, #703 ) ;
#27850 = CARTESIAN_POINT ( 'NONE',  ( 21.09992658989238734, 38.56284415653841791, 47.04930799450051637 ) ) ;
#27851 = AXIS2_PLACEMENT_3D ( 'NONE', #30121, #31923, #19598 ) ;
#27852 = ORIENTED_EDGE ( 'NONE', *, *, #20291, .F. ) ;
#27853 = AXIS2_PLACEMENT_3D ( 'NONE', #6015, #10458, #20454 ) ;
#27854 = DIRECTION ( 'NONE',  ( 0.000000000000000000, 0.000000000000000000, -1.000000000000000000 ) ) ;
#27855 = ORIENTED_EDGE ( 'NONE', *, *, #13107, .T. ) ;
#27856 = FACE_OUTER_BOUND ( 'NONE', #18850, .T. ) ;
#27857 = CARTESIAN_POINT ( 'NONE',  ( -42.37913764077812573, 15.23192269303852697, 38.44930799450052916 ) ) ;
#27858 = AXIS2_PLACEMENT_3D ( 'NONE', #3384, #23256, #5695 ) ;
#27859 = EDGE_LOOP ( 'NONE', ( #3535, #26697, #16549, #22480 ) ) ;
#27860 = CARTESIAN_POINT ( 'NONE',  ( 46.99031239021303463, 23.10527865767145173, 46.47233026104575515 ) ) ;
#27861 = DIRECTION ( 'NONE',  ( -0.000000000000000000, -1.000000000000000000, 0.000000000000000000 ) ) ;
#27862 = CARTESIAN_POINT ( 'NONE',  ( 8.732853799281734553, 38.56284415653841791, 47.04930799450051637 ) ) ;
#27863 = CARTESIAN_POINT ( 'NONE',  ( -42.59587854516874472, -0.7667456371672799476, 47.04930799450051637 ) ) ;
#27864 = CARTESIAN_POINT ( 'NONE',  ( 45.35708200440645044, 29.00457786121581805, 45.92000246470679770 ) ) ;
#27865 = DIRECTION ( 'NONE',  ( 0.000000000000000000, 0.000000000000000000, -1.000000000000000000 ) ) ;
#27866 = DIRECTION ( 'NONE',  ( -1.101824276508909887E-16, 1.000000000000000000, -0.000000000000000000 ) ) ;
#27867 = EDGE_CURVE ( 'NONE', #17879, #11837, #27286, .T. ) ;
#27868 = B_SPLINE_CURVE_WITH_KNOTS ( 'NONE', 3,
 ( #12154, #32175, #19684, #25272, #4925, #15419, #24950, #17222, #7711, #5251, #2297, #14780, #9690 ),
 .UNSPECIFIED., .F., .F.,
 ( 4, 3, 3, 3, 4 ),
 ( -1.894624554243639413E-05, 0.000000000000000000, 3.302537635573856920E-05, 7.371668740090159136E-05, 0.0001101628305730022953 ),
 .UNSPECIFIED. ) ;
#27869 = ORIENTED_EDGE ( 'NONE', *, *, #10614, .T. ) ;
#27870 = CARTESIAN_POINT ( 'NONE',  ( -40.60722745863126448, 9.415333058485023443, 38.60788663826321709 ) ) ;
#27871 = ORIENTED_EDGE ( 'NONE', *, *, #31104, .T. ) ;
#27872 = AXIS2_PLACEMENT_3D ( 'NONE', #3128, #26549, #21290 ) ;
#27873 = EDGE_CURVE ( 'NONE', #21830, #1880, #16833, .T. ) ;
#27874 = DIRECTION ( 'NONE',  ( -0.2756373558170018279, 0.9612616959383181170, 0.000000000000000000 ) ) ;
#27875 = EDGE_LOOP ( 'NONE', ( #5645, #27726, #1902, #15393 ) ) ;
#27876 = ORIENTED_EDGE ( 'NONE', *, *, #16959, .F. ) ;
#27877 = FACE_OUTER_BOUND ( 'NONE', #27888, .T. ) ;
#27878 = ADVANCED_FACE ( 'NONE', ( #14955 ), #16717, .T. ) ;
#27879 = ADVANCED_FACE ( 'NONE', ( #2475 ), #7302, .T. ) ;
#27880 = CIRCLE ( 'NONE', #29446, 0.4062389912925720714 ) ;
#27881 = ORIENTED_EDGE ( 'NONE', *, *, #12224, .T. ) ;
#27882 = AXIS2_PLACEMENT_3D ( 'NONE', #1733, #21749, #28826 ) ;
#27883 = AXIS2_PLACEMENT_3D ( 'NONE', #24488, #22349, #14821 ) ;
#27884 = ORIENTED_EDGE ( 'NONE', *, *, #15716, .T. ) ;
#27885 = DIRECTION ( 'NONE',  ( -0.000000000000000000, -1.000000000000000000, -0.000000000000000000 ) ) ;
#27886 = ADVANCED_FACE ( 'NONE', ( #30057 ), #22652, .T. ) ;
#27887 = CONICAL_SURFACE ( 'NONE', #8493, 72.00502525316939284, 0.7853981633974482790 ) ;
#27888 = EDGE_LOOP ( 'NONE', ( #19109, #9624, #26174, #1100 ) ) ;
#27889 = CARTESIAN_POINT ( 'NONE',  ( 47.94164539834608263, 29.49617064401329714, 45.04602341336960336 ) ) ;
#27890 = DIRECTION ( 'NONE',  ( -0.9612616959383207815, -0.2756373558169930016, 1.660411357259282199E-16 ) ) ;
#27891 = CARTESIAN_POINT ( 'NONE',  ( 48.94625023931840957, 25.27124452788249442, 46.10640627770150246 ) ) ;
#27892 = ORIENTED_EDGE ( 'NONE', *, *, #5163, .T. ) ;
#27893 = ORIENTED_EDGE ( 'NONE', *, *, #17153, .T. ) ;
#27894 = CARTESIAN_POINT ( 'NONE',  ( 21.09785597605719332, 16.33322284159648063, -0.3501356754177092911 ) ) ;
#27895 = EDGE_LOOP ( 'NONE', ( #6955, #29563, #21981 ) ) ;
#27896 = CARTESIAN_POINT ( 'NONE',  ( -40.11286833322907341, 2.887657226147507306, 37.04930799450052348 ) ) ;
#27897 = CARTESIAN_POINT ( 'NONE',  ( 54.13680899610202601, 0.4256545730735106781, 100.7294901468369233 ) ) ;
#27898 = CARTESIAN_POINT ( 'NONE',  ( 21.09785597605733187, -5.935454207752083988, 47.04930799450051637 ) ) ;
#27899 = DIRECTION ( 'NONE',  ( 0.9612616959383191162, 0.2756373558169986082, 8.795445018805098335E-19 ) ) ;
#27900 = CARTESIAN_POINT ( 'NONE',  ( 8.732853799281734553, 38.56284415653841791, 47.04930799450051637 ) ) ;
#27901 = EDGE_CURVE ( 'NONE', #19268, #27205, #5264, .T. ) ;
#27902 = APPLICATION_PROTOCOL_DEFINITION ( 'draft international standard', 'automotive_design', 1998, #25444 ) ;
#27903 = ORIENTED_EDGE ( 'NONE', *, *, #32080, .T. ) ;
#27904 = DIRECTION ( 'NONE',  ( -0.000000000000000000, 1.000000000000000000, -0.000000000000000000 ) ) ;
#27905 = DIRECTION ( 'NONE',  ( 1.344306794811909066E-16, -1.000000000000000000, 1.759793992609925531E-18 ) ) ;
#27906 = EDGE_CURVE ( 'NONE', #27774, #414, #6388, .T. ) ;
#27907 = DIRECTION ( 'NONE',  ( 0.9612616959383221138, 0.2756373558169876170, 0.000000000000000000 ) ) ;
#27908 = CARTESIAN_POINT ( 'NONE',  ( 46.00908685603033632, 28.33284706826092503, 44.91496614357595263 ) ) ;
#27909 = ORIENTED_EDGE ( 'NONE', *, *, #337, .F. ) ;
#27910 = DIRECTION ( 'NONE',  ( -1.000000000000000000, 0.000000000000000000, 0.000000000000000000 ) ) ;
#27911 = CARTESIAN_POINT ( 'NONE',  ( 21.09992658989239089, 26.84184655352419568, 47.04930799450051637 ) ) ;
#27912 = EDGE_CURVE ( 'NONE', #1878, #16844, #3092, .T. ) ;
#27913 = CARTESIAN_POINT ( 'NONE',  ( -30.49450530719115804, 11.01902901830102977, 22.43617484215558022 ) ) ;
#27914 = EDGE_CURVE ( 'NONE', #20784, #30017, #14715, .T. ) ;
#27915 = TOROIDAL_SURFACE ( 'NONE', #21077, 83.95481021798164534, 94.94530576803616384 ) ;
#27916 = VECTOR ( 'NONE', #434, 1000.000000000000000 ) ;
#27917 = EDGE_LOOP ( 'NONE', ( #16162, #12263, #11620, #23586 ) ) ;
#27918 = AXIS2_PLACEMENT_3D ( 'NONE', #18012, #4899, #5222 ) ;
#27919 = EDGE_LOOP ( 'NONE', ( #15428, #30627, #23079, #7724 ) ) ;
#27920 = CARTESIAN_POINT ( 'NONE',  ( -38.52112853513683888, -5.935454207752202116, 16.07118271501078510 ) ) ;
#27921 = CARTESIAN_POINT ( 'NONE',  ( -45.04500625625952637, -5.676766116611589474, 53.06055232190111326 ) ) ;
#27922 = CARTESIAN_POINT ( 'NONE',  ( 48.79245099466763946, 22.93807716476589675, 46.97542197481624271 ) ) ;
#27923 = VERTEX_POINT ( 'NONE', #18362 ) ;
#27924 = DIRECTION ( 'NONE',  ( -1.000000000000000000, 0.000000000000000000, 0.000000000000000000 ) ) ;
#27925 = LINE ( 'NONE', #25462, #2880 ) ;
#27926 = CARTESIAN_POINT ( 'NONE',  ( 34.09963999142011204, -5.098646251524523443, 47.04930799450052348 ) ) ;
#27927 = LINE ( 'NONE', #8075, #17337 ) ;
#27928 = CARTESIAN_POINT ( 'NONE',  ( -42.30123736278718383, 13.66041317296246937, 54.56265170360538264 ) ) ;
#27929 = CARTESIAN_POINT ( 'NONE',  ( 21.09992658989239089, 24.46664230456639899, 47.04930799450051637 ) ) ;
#27930 = DIRECTION ( 'NONE',  ( 1.000000000000000000, 0.000000000000000000, 2.775557561562892534E-15 ) ) ;
#27931 = CARTESIAN_POINT ( 'NONE',  ( 21.09785597605719332, -5.935454207752083988, 47.04930799449963530 ) ) ;
#27932 = CARTESIAN_POINT ( 'NONE',  ( -40.64500813507293486, 6.819128862114091305, 34.57932936825760351 ) ) ;
#27933 = VECTOR ( 'NONE', #21294, 1000.000000000000000 ) ;
#27934 = DIRECTION ( 'NONE',  ( -0.8746197071393858602, 0.4848096202463547666, 0.000000000000000000 ) ) ;
#27935 = AXIS2_PLACEMENT_3D ( 'NONE', #20166, #30192, #7703 ) ;
#27936 = EDGE_CURVE ( 'NONE', #6910, #27923, #21507, .T. ) ;
#27937 = CARTESIAN_POINT ( 'NONE',  ( 44.77625694075214824, 28.81454579807170546, 48.23360063142255427 ) ) ;
#27938 = ORIENTED_EDGE ( 'NONE', *, *, #28464, .T. ) ;
#27939 = ORIENTED_EDGE ( 'NONE', *, *, #18617, .T. ) ;
#27940 = CARTESIAN_POINT ( 'NONE',  ( 21.09992658989239089, 27.34164230456639544, 47.04930799450051637 ) ) ;
#27941 = CARTESIAN_POINT ( 'NONE',  ( 21.09992658989238734, 31.22145308207317171, 47.04930799450051637 ) ) ;
#27942 = CARTESIAN_POINT ( 'NONE',  ( -35.49409842342767263, -5.179470286602130713, 14.38986137883322769 ) ) ;
#27943 = CARTESIAN_POINT ( 'NONE',  ( 21.09992658989239089, 25.96183152705960140, 47.04930799450051637 ) ) ;
#27944 = ORIENTED_EDGE ( 'NONE', *, *, #6002, .T. ) ;
#27945 = VECTOR ( 'NONE', #8494, 1000.000000000000114 ) ;
#27946 = DIRECTION ( 'NONE',  ( -0.000000000000000000, -1.000000000000000000, 0.000000000000000000 ) ) ;
#27947 = CARTESIAN_POINT ( 'NONE',  ( 33.72499318558949000, 38.56284415653841791, 47.04930799450051637 ) ) ;
#27948 = CARTESIAN_POINT ( 'NONE',  ( -40.01678386995657632, 7.136726190597403985, 38.88517396861320918 ) ) ;
#27949 = VERTEX_POINT ( 'NONE', #28232 ) ;
#27950 = EDGE_LOOP ( 'NONE', ( #14618, #17340, #4094 ) ) ;
#27951 = DIRECTION ( 'NONE',  ( -0.4848096202463429982, -0.8746197071393925215, -9.920727850371698576E-18 ) ) ;
#27952 = CARTESIAN_POINT ( 'NONE',  ( 45.79384627280941089, 28.56618040159425931, 49.05938063676249072 ) ) ;
#27953 = FACE_OUTER_BOUND ( 'NONE', #31280, .T. ) ;
#27954 = ADVANCED_FACE ( 'NONE', ( #11319 ), #28394, .T. ) ;
#27955 = CARTESIAN_POINT ( 'NONE',  ( -39.41955952844167399, -5.936037113805915588, 77.90964267221822581 ) ) ;
#27956 = DIRECTION ( 'NONE',  ( -1.101824276508909887E-16, 1.000000000000000000, -0.000000000000000000 ) ) ;
#27957 = EDGE_LOOP ( 'NONE', ( #31501, #27551, #1909, #6275 ) ) ;
#27958 = AXIS2_PLACEMENT_3D ( 'NONE', #4031, #29146, #18951 ) ;
#27959 = TOROIDAL_SURFACE ( 'NONE', #15889, 41.50000000000000000, 1.499999999999997780 ) ;
#27960 = DIRECTION ( 'NONE',  ( -0.000000000000000000, -1.000000000000000000, 0.000000000000000000 ) ) ;
#27961 = FACE_OUTER_BOUND ( 'NONE', #12939, .T. ) ;
#27962 = VERTEX_POINT ( 'NONE', #23464 ) ;
#27963 = AXIS2_PLACEMENT_3D ( 'NONE', #30134, #32427, #20422 ) ;
#27964 = AXIS2_PLACEMENT_3D ( 'NONE', #22532, #27471, #5146 ) ;
#27965 =( BOUNDED_SURFACE ( )  B_SPLINE_SURFACE ( 3, 2, ( 
 ( #4521, #12079, #21585 ),
 ( #16504, #19278, #24376 ),
 ( #26680, #21414, #26358 ),
 ( #14221, #14540, #1565 ),
 ( #31456, #22073, #29305 ),
 ( #26846, #8793, #11751 ),
 ( #19452, #6825, #1895 ),
 ( #18791, #3876, #16824 ) ),
 .UNSPECIFIED., .F., .F., .F. ) 
 B_SPLINE_SURFACE_WITH_KNOTS ( ( 4, 2, 2, 4 ),
 ( 3, 3 ),
 ( -1.490777987167568597E-18, 0.0005623261017282611598, 0.0008434891525923924986, 0.001124652203456523837 ),
 ( 0.000000000000000000, 1.000000000000000000 ),
 .UNSPECIFIED. ) 
 GEOMETRIC_REPRESENTATION_ITEM ( )  RATIONAL_B_SPLINE_SURFACE ( (
 ( 1.000000000000000000, 0.7071067811865558994, 1.000000000000000000),
 ( 1.000000000000000000, 0.6846567335762145934, 1.000000000000000000),
 ( 1.000000000000000000, 0.6190846722317443485, 1.000000000000000000),
 ( 1.000000000000000000, 0.5161161862683902868, 1.000000000000000000),
 ( 1.000000000000000000, 0.4814351115860299180, 1.000000000000000000),
 ( 1.000000000000000000, 0.4264341115149925532, 1.000000000000000000),
 ( 1.000000000000000000, 0.4080770041851934926, 1.000000000000000000),
 ( 1.000000000000000000, 0.4082482904638556342, 1.000000000000000000) ) ) 
 REPRESENTATION_ITEM ( '' )  SURFACE ( )  );
#27966 = TOROIDAL_SURFACE ( 'NONE', #25849, 46.53489018157424084, 0.7000000000000002887 ) ;
#27967 = DIRECTION ( 'NONE',  ( -0.000000000000000000, -1.000000000000000000, -0.000000000000000000 ) ) ;
#27968 = PRODUCT_DEFINITION ( 'UNKNOWN', '', #31785, #7156 ) ;
#27969 = CARTESIAN_POINT ( 'NONE',  ( -9.831337038036075171, -5.937394935145314356, 107.7511683020618563 ) ) ;
#27970 = ORIENTED_EDGE ( 'NONE', *, *, #22162, .T. ) ;
#27971 = FACE_OUTER_BOUND ( 'NONE', #2128, .T. ) ;
#27972 = FACE_OUTER_BOUND ( 'NONE', #10475, .T. ) ;
#27973 = CARTESIAN_POINT ( 'NONE',  ( 21.09785597605719332, 30.56554579224779644, 75.54930799450052348 ) ) ;
#27974 = DIRECTION ( 'NONE',  ( 0.000000000000000000, 0.000000000000000000, -1.000000000000000000 ) ) ;
#27975 = DIRECTION ( 'NONE',  ( 0.000000000000000000, -0.2756373558165849391, -0.9612616959384376880 ) ) ;
#27976 = ORIENTED_EDGE ( 'NONE', *, *, #30631, .F. ) ;
#27977 = CARTESIAN_POINT ( 'NONE',  ( 74.12754556829368369, -0.2653311271195410437, 80.34416813279683822 ) ) ;
#27978 = DIRECTION ( 'NONE',  ( -0.4848096202463673121, -0.8746197071393789768, 0.000000000000000000 ) ) ;
#27979 = CARTESIAN_POINT ( 'NONE',  ( 7.596071960694297687, 15.70210863493540288, 47.04930799450052348 ) ) ;
#27980 = CARTESIAN_POINT ( 'NONE',  ( -38.21956313268621130, 5.305746783394874377, 42.04930799450051637 ) ) ;
#27981 = AXIS2_PLACEMENT_3D ( 'NONE', #31771, #6335, #16337 ) ;
#27982 = DIRECTION ( 'NONE',  ( -0.000000000000000000, -1.000000000000000000, -0.000000000000000000 ) ) ;
#27983 = VERTEX_POINT ( 'NONE', #21466 ) ;
#27984 = FACE_OUTER_BOUND ( 'NONE', #6475, .T. ) ;
#27985 = DIRECTION ( 'NONE',  ( -1.101824276508909887E-16, 1.000000000000000000, -0.000000000000000000 ) ) ;
#27986 = ORIENTED_EDGE ( 'NONE', *, *, #32402, .T. ) ;
#27987 = DIRECTION ( 'NONE',  ( 0.4544104193609913023, 0.000000000000000000, 0.8907924397839084296 ) ) ;
#27988 = CARTESIAN_POINT ( 'NONE',  ( 8.698509210239580014, 31.59164230456639544, 47.04930799450051637 ) ) ;
#27989 = FACE_OUTER_BOUND ( 'NONE', #28318, .T. ) ;
#27990 = EDGE_CURVE ( 'NONE', #4649, #4406, #31504, .T. ) ;
#27991 = CARTESIAN_POINT ( 'NONE',  ( -40.02540636251514172, 2.839176264122877047, 57.04930799450051637 ) ) ;
#27992 = AXIS2_PLACEMENT_3D ( 'NONE', #24377, #24540, #12080 ) ;
#27993 = EDGE_CURVE ( 'NONE', #13215, #9599, #31314, .T. ) ;
#27994 = EDGE_CURVE ( 'NONE', #7860, #15433, #1594, .T. ) ;
#27995 = VERTEX_POINT ( 'NONE', #11160 ) ;
#27996 = ADVANCED_FACE ( 'NONE', ( #18841 ), #24142, .T. ) ;
#27997 = FACE_OUTER_BOUND ( 'NONE', #6532, .T. ) ;
#27998 = ORIENTED_EDGE ( 'NONE', *, *, #19291, .F. ) ;
#27999 = EDGE_CURVE ( 'NONE', #30811, #11408, #17790, .T. ) ;
#28000 = ORIENTED_EDGE ( 'NONE', *, *, #28710, .T. ) ;
#28001 = CIRCLE ( 'NONE', #13348, 1.899999999999999023 ) ;
#28002 = CARTESIAN_POINT ( 'NONE',  ( 21.09992658989239089, 30.34164230456639544, 47.04930799450051637 ) ) ;
#28003 = DIRECTION ( 'NONE',  ( 0.000000000000000000, -1.000000000000000000, 0.000000000000000000 ) ) ;
#28004 = CARTESIAN_POINT ( 'NONE',  ( 81.72575882806418690, -5.937394852768786535, 15.98100540722295015 ) ) ;
#28005 = ORIENTED_EDGE ( 'NONE', *, *, #29203, .T. ) ;
#28006 = ORIENTED_EDGE ( 'NONE', *, *, #5360, .F. ) ;
#28007 = CIRCLE ( 'NONE', #28553, 0.09999999999999939493 ) ;
#28008 = CARTESIAN_POINT ( 'NONE',  ( -9.474781401982005136, 5.388785998227653806, 106.8025418868326284 ) ) ;
#28009 = DIRECTION ( 'NONE',  ( -1.101824276508909887E-16, 1.000000000000000000, -0.000000000000000000 ) ) ;
#28010 = CARTESIAN_POINT ( 'NONE',  ( -31.40817747290099859, 3.832457305373850875, 78.38424341102378889 ) ) ;
#28011 = DIRECTION ( 'NONE',  ( -0.000000000000000000, 1.000000000000000000, -0.000000000000000000 ) ) ;
#28012 = EDGE_CURVE ( 'NONE', #28041, #8773, #25920, .T. ) ;
#28013 = VERTEX_POINT ( 'NONE', #13310 ) ;
#28014 = CARTESIAN_POINT ( 'NONE',  ( -41.91739890389096956, 13.90674392281399818, 54.59993297551692848 ) ) ;
#28015 = ORIENTED_EDGE ( 'NONE', *, *, #18727, .T. ) ;
#28016 = LINE ( 'NONE', #11109, #9685 ) ;
#28017 = LINE ( 'NONE', #21093, #21616 ) ;
#28018 = ORIENTED_EDGE ( 'NONE', *, *, #13182, .F. ) ;
#28019 = CARTESIAN_POINT ( 'NONE',  ( 46.96997866373305186, 23.12036939723557083, 46.79862680810013131 ) ) ;
#28020 = CARTESIAN_POINT ( 'NONE',  ( 81.71662875395456638, -5.936382080411370055, 16.04580235805854471 ) ) ;
#28021 = DIRECTION ( 'NONE',  ( -1.188208965918165239E-16, -1.880121038077813132E-16, -1.000000000000000000 ) ) ;
#28022 = CARTESIAN_POINT ( 'NONE',  ( 21.09992658989239089, 25.59184655352419213, 47.04930799450051637 ) ) ;
#28023 = CYLINDRICAL_SURFACE ( 'NONE', #8937, 12.62506659569710266 ) ;
#28024 = CARTESIAN_POINT ( 'NONE',  ( 44.21498992391907024, 28.69488759933318178, 46.89958605635244027 ) ) ;
#28025 = CYLINDRICAL_SURFACE ( 'NONE', #7540, 0.1000000000000007272 ) ;
#28026 = VERTEX_POINT ( 'NONE', #8694 ) ;
#28027 = DIRECTION ( 'NONE',  ( -0.2756373558169932236, 0.9612616959383204485, -1.479773560108267395E-16 ) ) ;
#28028 = DIRECTION ( 'NONE',  ( 8.659560562355053653E-17, -0.7071067811865378028, 0.7071067811865573427 ) ) ;
#28029 = EDGE_CURVE ( 'NONE', #7677, #11017, #20410, .T. ) ;
#28030 = EDGE_CURVE ( 'NONE', #2441, #13945, #24606, .T. ) ;
#28031 = ORIENTED_EDGE ( 'NONE', *, *, #1207, .F. ) ;
#28032 = AXIS2_PLACEMENT_3D ( 'NONE', #10366, #11015, #18064 ) ;
#28033 = ADVANCED_FACE ( 'NONE', ( #3435 ), #28558, .T. ) ;
#28034 = COLOUR_RGB ( '',0.7921568627450980005, 0.8196078431372548767, 0.9333333333333333481 ) ;
#28035 = ORIENTED_EDGE ( 'NONE', *, *, #16334, .T. ) ;
#28036 = CYLINDRICAL_SURFACE ( 'NONE', #2068, 2.500000000000002220 ) ;
#28037 = AXIS2_PLACEMENT_3D ( 'NONE', #17988, #27848, #7993 ) ;
#28038 = EDGE_CURVE ( 'NONE', #24958, #10579, #3641, .T. ) ;
#28039 = CIRCLE ( 'NONE', #14934, 0.09999999999999795164 ) ;
#28040 = CIRCLE ( 'NONE', #23822, 0.2999999999999947153 ) ;
#28041 = VERTEX_POINT ( 'NONE', #31185 ) ;
#28042 = VERTEX_POINT ( 'NONE', #16227 ) ;
#28043 = CARTESIAN_POINT ( 'NONE',  ( 8.732853799281729223, 24.22145308207319303, 47.04930799450051637 ) ) ;
#28044 = ORIENTED_EDGE ( 'NONE', *, *, #27389, .F. ) ;
#28045 = CIRCLE ( 'NONE', #1324, 12.36707279061065279 ) ;
#28046 = LINE ( 'NONE', #23116, #12002 ) ;
#28047 = FACE_OUTER_BOUND ( 'NONE', #6182, .T. ) ;
#28048 = CARTESIAN_POINT ( 'NONE',  ( 52.36191254139992424, -5.922252862938464979, 106.4668663603234933 ) ) ;
#28049 = AXIS2_PLACEMENT_3D ( 'NONE', #23648, #1153, #20857 ) ;
#28050 = CARTESIAN_POINT ( 'NONE',  ( 48.16694854572211426, 27.91789516297709284, 49.14507740233662503 ) ) ;
#28051 = EDGE_CURVE ( 'NONE', #272, #9936, #26247, .T. ) ;
#28052 = ORIENTED_EDGE ( 'NONE', *, *, #6814, .F. ) ;
#28053 = VERTEX_POINT ( 'NONE', #19332 ) ;
#28055 = CARTESIAN_POINT ( 'NONE',  ( -40.06561427811386267, 7.496110634155836117, 56.04611646155296256 ) ) ;
#28054 = CIRCLE ( 'NONE', #15475, 37.00000000000000711 ) ;
#28056 = ADVANCED_FACE ( 'NONE', ( #1619 ), #9177, .F. ) ;
#28057 = CIRCLE ( 'NONE', #801, 37.00000000000000711 ) ;
#28058 = EDGE_LOOP ( 'NONE', ( #4759, #2416, #12420, #31189 ) ) ;
#28059 = CARTESIAN_POINT ( 'NONE',  ( 45.32414328224286493, 11.18784031540631752, 98.72179417164551296 ) ) ;
#28060 = CIRCLE ( 'NONE', #22801, 0.1250000000000001110 ) ;
#28061 = FACE_OUTER_BOUND ( 'NONE', #23850, .T. ) ;
#28062 = DIRECTION ( 'NONE',  ( 0.9612616959383221138, 0.2756373558169876170, 0.000000000000000000 ) ) ;
#28063 = FACE_OUTER_BOUND ( 'NONE', #3041, .T. ) ;
#28064 = CARTESIAN_POINT ( 'NONE',  ( 46.00908685603032922, 25.44624452788248448, 44.91496614357595263 ) ) ;
#28065 = EDGE_LOOP ( 'NONE', ( #26097, #493, #18326, #22352 ) ) ;
#28066 = DIRECTION ( 'NONE',  ( -1.000000000000000000, -1.101824276508909887E-16, 0.000000000000000000 ) ) ;
#28067 = FACE_OUTER_BOUND ( 'NONE', #7051, .T. ) ;
#28068 = B_SPLINE_CURVE_WITH_KNOTS ( 'NONE', 3,
 ( #24005, #1195, #11223, #3346, #21213, #23372, #28947, #30929, #31250, #18746, #6292, #16299, #879, #20901, #7273, #22026, #4317, #12368, #14828 ),
 .UNSPECIFIED., .F., .F.,
 ( 4, 3, 3, 3, 3, 3, 4 ),
 ( -2.120612755851273058E-06, 0.000000000000000000, 4.415954867017419676E-05, 9.459217447090470185E-05, 0.0001331301346428089677, 0.0001600668633085419994, 0.0001872567722942432159 ),
 .UNSPECIFIED. ) ;
#28069 = DIRECTION ( 'NONE',  ( -1.000000000000000000, 0.000000000000000000, 0.000000000000000000 ) ) ;
#28070 = CARTESIAN_POINT ( 'NONE',  ( 45.24946171279598417, 26.40784706826093498, 47.99220971130008451 ) ) ;
#28071 = EDGE_LOOP ( 'NONE', ( #5477, #29528, #4668, #19627 ) ) ;
#28072 = DIRECTION ( 'NONE',  ( -0.7141240004913222972, 0.3958453973320028019, -0.5773502691896303940 ) ) ;
#28073 = DIRECTION ( 'NONE',  ( 0.000000000000000000, -1.000000000000000000, 0.000000000000000000 ) ) ;
#28074 = EDGE_CURVE ( 'NONE', #665, #31921, #7852, .T. ) ;
#28075 = CARTESIAN_POINT ( 'NONE',  ( 8.482002859293411134, 25.46664230456640254, 47.04930799450051637 ) ) ;
#28076 = ORIENTED_EDGE ( 'NONE', *, *, #11776, .F. ) ;
#28077 = AXIS2_PLACEMENT_3D ( 'NONE', #29010, #16522, #14077 ) ;
#28078 = AXIS2_PLACEMENT_3D ( 'NONE', #14291, #20012, #5250 ) ;
#28079 = TOROIDAL_SURFACE ( 'NONE', #23869, 23.50000000000000000, 2.000000000000001776 ) ;
#28080 = MECHANICAL_DESIGN_GEOMETRIC_PRESENTATION_REPRESENTATION (  '', ( #14473 ), #13926 ) ;
#28081 = AXIS2_PLACEMENT_3D ( 'NONE', #9437, #6970, #1387 ) ;
#28082 = ORIENTED_EDGE ( 'NONE', *, *, #10040, .T. ) ;
#28083 = VERTEX_POINT ( 'NONE', #31819 ) ;
#28084 = EDGE_CURVE ( 'NONE', #18405, #9796, #17898, .T. ) ;
#28085 = FACE_OUTER_BOUND ( 'NONE', #11277, .T. ) ;
#28086 = DIRECTION ( 'NONE',  ( 0.000000000000000000, 0.000000000000000000, -1.000000000000000000 ) ) ;
#28087 = DIRECTION ( 'NONE',  ( -2.779292025043186357E-18, 1.288349127009862211E-17, -1.000000000000000000 ) ) ;
#28088 = EDGE_CURVE ( 'NONE', #22382, #3968, #1541, .T. ) ;
#28089 = AXIS2_PLACEMENT_3D ( 'NONE', #29206, #21000, #19177 ) ;
#28090 = ORIENTED_EDGE ( 'NONE', *, *, #22252, .T. ) ;
#28091 = CARTESIAN_POINT ( 'NONE',  ( -38.65545646816406133, -5.472247659560185440, 79.55937378679692529 ) ) ;
#28092 = CARTESIAN_POINT ( 'NONE',  ( -40.70508238852950456, 9.491303552449116054, 39.44930799450052206 ) ) ;
#28093 = DIRECTION ( 'NONE',  ( -0.8746197071393790878, 0.4848096202463673676, 1.277302113040196197E-17 ) ) ;
#28094 = ADVANCED_FACE ( 'NONE', ( #4079 ), #4171, .T. ) ;
#28095 = DIRECTION ( 'NONE',  ( -0.9612616959383194493, -0.2756373558169972759, -8.795445018804905742E-19 ) ) ;
#28096 = ADVANCED_FACE ( 'NONE', ( #24426 ), #10480, .T. ) ;
#28097 = DIRECTION ( 'NONE',  ( -1.000000000000000000, 0.000000000000000000, 0.000000000000000000 ) ) ;
#28098 = EDGE_CURVE ( 'NONE', #25493, #9681, #28802, .T. ) ;
#28099 = CARTESIAN_POINT ( 'NONE',  ( -39.67555847965937943, 2.645252416024337361, 47.04930799450051637 ) ) ;
#28100 = DIRECTION ( 'NONE',  ( -0.4848096202463645921, -0.8746197071393805311, 0.000000000000000000 ) ) ;
#28101 = CYLINDRICAL_SURFACE ( 'NONE', #2158, 12.98419020052702599 ) ;
#28102 = CARTESIAN_POINT ( 'NONE',  ( 41.51205063648688309, 1.925589859889728972, 132.0493079945005377 ) ) ;
#28103 = CARTESIAN_POINT ( 'NONE',  ( 44.25133798441032695, 11.55977609614116020, 98.10820709097123427 ) ) ;
#28104 = CARTESIAN_POINT ( 'NONE',  ( -43.42682711710880739, 1.034448000281937396, 34.64930799450052490 ) ) ;
#28105 =( NAMED_UNIT ( * ) SI_UNIT ( $, .STERADIAN. ) SOLID_ANGLE_UNIT ( ) );
#28106 = ORIENTED_EDGE ( 'NONE', *, *, #9263, .F. ) ;
#28107 = ORIENTED_EDGE ( 'NONE', *, *, #30104, .T. ) ;
#28108 = CARTESIAN_POINT ( 'NONE',  ( -41.24971778908466291, 11.62557032131817181, 57.04930799450051637 ) ) ;
#28109 = AXIS2_PLACEMENT_3D ( 'NONE', #15104, #24786, #22474 ) ;
#28110 =( GEOMETRIC_REPRESENTATION_CONTEXT ( 3 ) GLOBAL_UNCERTAINTY_ASSIGNED_CONTEXT ( ( #20643 ) ) GLOBAL_UNIT_ASSIGNED_CONTEXT ( ( #5776, #8870, #13807 ) ) REPRESENTATION_CONTEXT ( 'NONE', 'WORKASPACE' ) );
#28111 = CARTESIAN_POINT ( 'NONE',  ( 21.09785597605719332, 25.56454579224779877, 75.54930799450052348 ) ) ;
#28112 = CARTESIAN_POINT ( 'NONE',  ( 52.11424208273423631, 4.323180411458207750, 98.49488265617655713 ) ) ;
#28113 = ORIENTED_EDGE ( 'NONE', *, *, #32030, .T. ) ;
#28114 = DIRECTION ( 'NONE',  ( -1.101824276508909887E-16, 1.000000000000000000, -0.000000000000000000 ) ) ;
#28115 = ORIENTED_EDGE ( 'NONE', *, *, #17860, .F. ) ;
#28116 = ORIENTED_EDGE ( 'NONE', *, *, #13241, .F. ) ;
#28117 = CARTESIAN_POINT ( 'NONE',  ( 21.09992658989239089, 26.34143805560860940, 47.04930799450051637 ) ) ;
#28118 = CARTESIAN_POINT ( 'NONE',  ( 48.18662509608405031, 25.18284706826093355, 49.18364984542562013 ) ) ;
#28119 = EDGE_CURVE ( 'NONE', #31932, #28443, #15175, .T. ) ;
#28120 = CARTESIAN_POINT ( 'NONE',  ( 48.94625023931840246, 28.77124452788248377, 46.10640627770150246 ) ) ;
#28121 = AXIS2_PLACEMENT_3D ( 'NONE', #7295, #32247, #25178 ) ;
#28122 = CARTESIAN_POINT ( 'NONE',  ( -39.51359738027355206, -5.935454207752198563, 77.87546120947918382 ) ) ;
#28123 = ORIENTED_EDGE ( 'NONE', *, *, #16340, .T. ) ;
#28124 = EDGE_CURVE ( 'NONE', #28042, #29498, #14106, .T. ) ;
#28125 = FACE_OUTER_BOUND ( 'NONE', #18418, .T. ) ;
#28126 = TOROIDAL_SURFACE ( 'NONE', #1418, 12.40141737965286595, 0.1249999999999979183 ) ;
#28127 = DIRECTION ( 'NONE',  ( -0.000000000000000000, -1.000000000000000000, 0.000000000000000000 ) ) ;
#28128 = ADVANCED_FACE ( 'NONE', ( #16876 ), #11961, .F. ) ;
#28129 = VERTEX_POINT ( 'NONE', #14589 ) ;
#28130 = CARTESIAN_POINT ( 'NONE',  ( 45.96182992765471909, 26.60087065737812040, 44.82232689504102296 ) ) ;
#28131 = CARTESIAN_POINT ( 'NONE',  ( 45.39969523643555505, 22.86454579224779948, 45.99212200068701861 ) ) ;
#28132 = DIRECTION ( 'NONE',  ( -1.101824276508909887E-16, 1.000000000000000000, -0.000000000000000000 ) ) ;
#28133 = ADVANCED_FACE ( 'NONE', ( #9504 ), #31948, .T. ) ;
#28134 = CIRCLE ( 'NONE', #13984, 12.36707279061065101 ) ;
#28135 = VERTEX_POINT ( 'NONE', #14755 ) ;
#28136 = DIRECTION ( 'NONE',  ( 0.000000000000000000, -1.000000000000000000, 0.000000000000000000 ) ) ;
#28137 = EDGE_CURVE ( 'NONE', #2041, #17732, #12033, .T. ) ;
#28138 = CARTESIAN_POINT ( 'NONE',  ( -42.59587854516874472, -0.7667456371672812798, 32.14930799450051779 ) ) ;
#28139 = CARTESIAN_POINT ( 'NONE',  ( 41.59785597605720397, 13.86454579224779948, 47.04930799450052348 ) ) ;
#28140 = LINE ( 'NONE', #15337, #20513 ) ;
#28141 = DIRECTION ( 'NONE',  ( -0.000000000000000000, -1.000000000000000000, -0.000000000000000000 ) ) ;
#28142 = ORIENTED_EDGE ( 'NONE', *, *, #8535, .T. ) ;
#28143 = CYLINDRICAL_SURFACE ( 'NONE', #19147, 12.62506659569710266 ) ;
#28144 = EDGE_CURVE ( 'NONE', #11753, #25296, #19347, .T. ) ;
#28145 = FACE_OUTER_BOUND ( 'NONE', #26156, .T. ) ;
#28146 = DIRECTION ( 'NONE',  ( -0.000000000000000000, -1.000000000000000000, 0.000000000000000000 ) ) ;
#28147 = CARTESIAN_POINT ( 'NONE',  ( 21.09785597605720753, 13.86454579224779948, 47.04930799450052348 ) ) ;
#28148 = CARTESIAN_POINT ( 'NONE',  ( 78.88609142827000653, -5.395280703882846751, 79.46745756311666753 ) ) ;
#28149 = ORIENTED_EDGE ( 'NONE', *, *, #8447, .F. ) ;
#28150 = DIRECTION ( 'NONE',  ( -4.163336342344333082E-15, 0.000000000000000000, 1.000000000000000000 ) ) ;
#28151 = CARTESIAN_POINT ( 'NONE',  ( -40.65065394966018175, 6.870367549600012502, 39.15777990219699944 ) ) ;
#28152 = CARTESIAN_POINT ( 'NONE',  ( 21.09785597605720753, 14.61319044934410627, 47.04930799450052348 ) ) ;
#28153 = ORIENTED_EDGE ( 'NONE', *, *, #23785, .F. ) ;
#28154 = CARTESIAN_POINT ( 'NONE',  ( -10.70116484021380643, -5.771419034597320419, -11.48608978375909651 ) ) ;
#28155 = CYLINDRICAL_SURFACE ( 'NONE', #31426, 84.30000000000001137 ) ;
#28156 = DIRECTION ( 'NONE',  ( 1.234978253042719660E-16, -1.000000000000000000, -1.109335647967047851E-31 ) ) ;
#28157 = ORIENTED_EDGE ( 'NONE', *, *, #11434, .T. ) ;
#28158 = CARTESIAN_POINT ( 'NONE',  ( -40.46271621608484281, 3.081581074246047436, 47.04930799450051637 ) ) ;
#28159 = ORIENTED_EDGE ( 'NONE', *, *, #29500, .T. ) ;
#28160 = ORIENTED_EDGE ( 'NONE', *, *, #26124, .T. ) ;
#28161 = SHAPE_REPRESENTATION ( 'Terminals', ( #8172 ), #12388 ) ;
#28162 = DIRECTION ( 'NONE',  ( -1.101824276508909887E-16, 1.000000000000000000, -0.000000000000000000 ) ) ;
#28163 = DIRECTION ( 'NONE',  ( 0.000000000000000000, 0.000000000000000000, -1.000000000000000000 ) ) ;
#28164 = DIRECTION ( 'NONE',  ( 0.000000000000000000, -1.000000000000000000, -0.000000000000000000 ) ) ;
#28165 = CIRCLE ( 'NONE', #4581, 0.1250000000000001110 ) ;
#28166 = EDGE_CURVE ( 'NONE', #25278, #1884, #27226, .T. ) ;
#28167 = ORIENTED_EDGE ( 'NONE', *, *, #27668, .T. ) ;
#28168 = DIRECTION ( 'NONE',  ( -1.000000000000000000, 0.000000000000000000, 0.000000000000000000 ) ) ;
#28169 = ORIENTED_EDGE ( 'NONE', *, *, #23977, .T. ) ;
#28170 = CARTESIAN_POINT ( 'NONE',  ( 21.09992658989239089, 29.96183152705961206, 47.04930799450051637 ) ) ;
#28171 = CARTESIAN_POINT ( 'NONE',  ( 21.09992658989238734, 31.09143805560860585, 47.04930799450051637 ) ) ;
#28172 = CARTESIAN_POINT ( 'NONE',  ( -36.49977054276610033, -5.245772846439738402, 79.63610610625367769 ) ) ;
#28173 = AXIS2_PLACEMENT_3D ( 'NONE', #6776, #19728, #16778 ) ;
#28174 = CARTESIAN_POINT ( 'NONE',  ( -40.61463551858322063, 9.441168033762318501, 35.47959690138647204 ) ) ;
#28175 = ORIENTED_EDGE ( 'NONE', *, *, #22438, .T. ) ;
#28176 = CARTESIAN_POINT ( 'NONE',  ( 21.09992658989239089, 26.84164230456639899, 47.04930799450051637 ) ) ;
#28177 = VERTEX_POINT ( 'NONE', #27213 ) ;
#28178 = DIRECTION ( 'NONE',  ( 0.000000000000000000, 0.000000000000000000, 1.000000000000000000 ) ) ;
#28179 = CARTESIAN_POINT ( 'NONE',  ( -41.94956971822180947, 3.905757428664830222, 45.04930799450051637 ) ) ;
#28180 = ORIENTED_EDGE ( 'NONE', *, *, #24442, .F. ) ;
#28181 = CARTESIAN_POINT ( 'NONE',  ( 33.46699938050303302, 38.56284415653841791, 47.04930799450051637 ) ) ;
#28182 = DIRECTION ( 'NONE',  ( 0.000000000000000000, 1.000000000000000000, -0.000000000000000000 ) ) ;
#28183 = DIRECTION ( 'NONE',  ( -1.101824276508909887E-16, 1.000000000000000000, -0.000000000000000000 ) ) ;
#28184 = DIRECTION ( 'NONE',  ( 0.000000000000000000, -1.000000000000000000, 0.000000000000000000 ) ) ;
#28185 = SURFACE_STYLE_USAGE ( .BOTH. , #26030 ) ;
#28186 = CARTESIAN_POINT ( 'NONE',  ( 46.96819297411687444, 28.86988759933318249, 49.54594323136014822 ) ) ;
#28187 = DIRECTION ( 'NONE',  ( -0.2756373558170082672, 0.9612616959383162296, 0.000000000000000000 ) ) ;
#28188 = ORIENTED_EDGE ( 'NONE', *, *, #32281, .F. ) ;
#28189 = DIRECTION ( 'NONE',  ( 0.000000000000000000, 0.000000000000000000, -1.000000000000000000 ) ) ;
#28190 = CARTESIAN_POINT ( 'NONE',  ( 21.09992658989238734, 38.56284415653841791, 47.04930799450051637 ) ) ;
#28191 = ORIENTED_EDGE ( 'NONE', *, *, #9717, .T. ) ;
#28192 = VERTEX_POINT ( 'NONE', #29037 ) ;
#28193 = CARTESIAN_POINT ( 'NONE',  ( -42.28651568955962858, 14.71554561121750559, 55.11195069825311776 ) ) ;
#28194 = CIRCLE ( 'NONE', #7243, 12.62506659569710266 ) ;
#28195 = TOROIDAL_SURFACE ( 'NONE', #17240, 12.40141737965283042, 0.1249999999999995420 ) ;
#28196 = ORIENTED_EDGE ( 'NONE', *, *, #4168, .T. ) ;
#28197 = VECTOR ( 'NONE', #29523, 999.9999999999998863 ) ;
#28198 = CIRCLE ( 'NONE', #16651, 0.1000000000000014905 ) ;
#28199 = ORIENTED_EDGE ( 'NONE', *, *, #1745, .F. ) ;
#28200 = B_SPLINE_CURVE_WITH_KNOTS ( 'NONE', 3,
 ( #18390, #28420, #3458, #13647, #23649, #13486, #11181, #21166, #31205, #3780 ),
 .UNSPECIFIED., .F., .F.,
 ( 4, 2, 2, 2, 4 ),
 ( 0.01122971665427002254, 0.01185769113519980454, 0.01248566561612958481, 0.01311364009705936681, 0.01374161457798914882 ),
 .UNSPECIFIED. ) ;
#28201 = CYLINDRICAL_SURFACE ( 'NONE', #1829, 0.1000000000000028644 ) ;
#28202 = VERTEX_POINT ( 'NONE', #4737 ) ;
#28203 = ADVANCED_FACE ( 'NONE', ( #6554 ), #18327, .T. ) ;
#28204 = ADVANCED_FACE ( 'NONE', ( #22443 ), #27752, .F. ) ;
#28205 = CARTESIAN_POINT ( 'NONE',  ( 47.65130514356931002, 23.10527865767145173, 47.24466138387320768 ) ) ;
#28206 = ADVANCED_FACE ( 'NONE', ( #17687 ), #28036, .F. ) ;
#28207 = CARTESIAN_POINT ( 'NONE',  ( -39.64148344771002286, 7.657122216028890982, 61.94930799450052206 ) ) ;
#28208 = CARTESIAN_POINT ( 'NONE',  ( 52.14324879758525100, -5.938447472589719389, 106.6451039912369225 ) ) ;
#28209 = EDGE_CURVE ( 'NONE', #19002, #24759, #29867, .T. ) ;
#28210 = ADVANCED_FACE ( 'NONE', ( #7854 ), #29856, .T. ) ;
#28211 = CARTESIAN_POINT ( 'NONE',  ( 48.80717017713595141, 26.57622849631043138, 48.15820438821415195 ) ) ;
#28212 = ORIENTED_EDGE ( 'NONE', *, *, #5422, .T. ) ;
#28213 = TOROIDAL_SURFACE ( 'NONE', #28746, 12.61792373059891048, 0.1250000000000026368 ) ;
#28214 = VERTEX_POINT ( 'NONE', #15238 ) ;
#28215 = FACE_OUTER_BOUND ( 'NONE', #27859, .T. ) ;
#28216 = AXIS2_PLACEMENT_3D ( 'NONE', #10969, #14395, #1421 ) ;
#28217 = ORIENTED_EDGE ( 'NONE', *, *, #31509, .T. ) ;
#28218 = DIRECTION ( 'NONE',  ( -1.224646799147353207E-16, -1.349345573449484691E-32, 1.000000000000000000 ) ) ;
#28219 = CARTESIAN_POINT ( 'NONE',  ( 53.82666426033320306, 1.147918989839220805, 100.4501361902863010 ) ) ;
#28220 = CARTESIAN_POINT ( 'NONE',  ( 47.09785597605719687, 20.36454579224779948, 47.04930799450078638 ) ) ;
#28221 = CIRCLE ( 'NONE', #20330, 0.1250000000000001110 ) ;
#28222 = TOROIDAL_SURFACE ( 'NONE', #15120, 12.40141737965281976, 0.1249999999999999722 ) ;
#28223 = LINE ( 'NONE', #3583, #10029 ) ;
#28224 = CARTESIAN_POINT ( 'NONE',  ( 33.72499318558949000, 38.56284415653841791, 47.04930799450051637 ) ) ;
#28225 = EDGE_LOOP ( 'NONE', ( #5098, #7463, #1258, #18052 ) ) ;
#28226 = CARTESIAN_POINT ( 'NONE',  ( 21.09785597605719332, -19.93545420775220123, 47.04930799450051637 ) ) ;
#28227 = DIRECTION ( 'NONE',  ( -1.000000000000000000, 0.000000000000000000, 0.000000000000000000 ) ) ;
#28228 = CIRCLE ( 'NONE', #3042, 0.1000000000000028644 ) ;
#28229 = DIRECTION ( 'NONE',  ( 0.000000000000000000, 0.000000000000000000, -1.000000000000000000 ) ) ;
#28230 = CARTESIAN_POINT ( 'NONE',  ( 47.20547626766764893, 26.17451373492760069, 44.97710074790751378 ) ) ;
#28231 = ORIENTED_EDGE ( 'NONE', *, *, #26049, .F. ) ;
#28232 = CARTESIAN_POINT ( 'NONE',  ( 21.09785597605719332, 15.43591091851533115, 60.03349819502753348 ) ) ;
#28233 = DIRECTION ( 'NONE',  ( 0.000000000000000000, -1.000000000000000000, -0.000000000000000000 ) ) ;
#28234 = ORIENTED_EDGE ( 'NONE', *, *, #31531, .F. ) ;
#28235 = EDGE_CURVE ( 'NONE', #13775, #22338, #30018, .T. ) ;
#28236 = ADVANCED_FACE ( 'NONE', ( #27877 ), #5394, .T. ) ;
#28237 = CIRCLE ( 'NONE', #7270, 12.36707279061065101 ) ;
#28238 = AXIS2_PLACEMENT_3D ( 'NONE', #29195, #29359, #24101 ) ;
#28239 = ORIENTED_EDGE ( 'NONE', *, *, #8573, .T. ) ;
#28240 = AXIS2_PLACEMENT_3D ( 'NONE', #2470, #12819, #7719 ) ;
#28241 = CIRCLE ( 'NONE', #18264, 12.62506659569710266 ) ;
#28242 = ORIENTED_EDGE ( 'NONE', *, *, #28288, .F. ) ;
#28243 = DIRECTION ( 'NONE',  ( -0.2756373558170082672, 0.9612616959383162296, 0.000000000000000000 ) ) ;
#28244 = CARTESIAN_POINT ( 'NONE',  ( 21.09785597605719332, -16.63545420775219696, 47.04930799450051637 ) ) ;
#28245 = CARTESIAN_POINT ( 'NONE',  ( 48.78406556707242459, 22.93807716476589675, 47.13688154746046166 ) ) ;
#28246 = TOROIDAL_SURFACE ( 'NONE', #24551, 12.40141737965288193, 0.1250000000000005829 ) ;
#28247 = ORIENTED_EDGE ( 'NONE', *, *, #23881, .T. ) ;
#28248 = FACE_OUTER_BOUND ( 'NONE', #32495, .T. ) ;
#28249 = CARTESIAN_POINT ( 'NONE',  ( -41.23380787120766655, 11.23768311167744294, 38.19144330556764544 ) ) ;
#28250 = DIRECTION ( 'NONE',  ( 1.000000000000000000, 0.000000000000000000, 0.000000000000000000 ) ) ;
#28251 = ADVANCED_FACE ( 'NONE', ( #12946 ), #28296, .T. ) ;
#28252 = DIRECTION ( 'NONE',  ( -0.000000000000000000, -1.000000000000000000, -0.000000000000000000 ) ) ;
#28253 = DIRECTION ( 'NONE',  ( -1.000000000000000000, 0.000000000000000000, 0.000000000000000000 ) ) ;
#28254 = DIRECTION ( 'NONE',  ( -1.000000000000000000, 0.000000000000000000, 0.000000000000000000 ) ) ;
#28255 = CYLINDRICAL_SURFACE ( 'NONE', #12190, 1.500000000000001332 ) ;
#28256 = DIRECTION ( 'NONE',  ( 1.101824276508909887E-16, -1.000000000000000000, 0.000000000000000000 ) ) ;
#28257 = DIRECTION ( 'NONE',  ( -0.000000000000000000, -1.000000000000000000, -0.000000000000000000 ) ) ;
#28258 = DIRECTION ( 'NONE',  ( -0.000000000000000000, 1.000000000000000000, 0.000000000000000000 ) ) ;
#28259 = ORIENTED_EDGE ( 'NONE', *, *, #26421, .F. ) ;
#28260 = ORIENTED_EDGE ( 'NONE', *, *, #21589, .T. ) ;
#28261 = DIRECTION ( 'NONE',  ( 0.000000000000000000, 0.000000000000000000, 1.000000000000000000 ) ) ;
#28262 = MECHANICAL_DESIGN_GEOMETRIC_PRESENTATION_REPRESENTATION (  '', ( #19864 ), #5719 ) ;
#28263 = DIRECTION ( 'NONE',  ( -0.8746197071393926326, 0.4848096202463430537, 8.676864087101709653E-18 ) ) ;
#28264 = CIRCLE ( 'NONE', #14110, 0.5000000000000004441 ) ;
#28265 = DIRECTION ( 'NONE',  ( 1.000000000000000000, -0.000000000000000000, 1.224646799147353207E-16 ) ) ;
#28266 = ORIENTED_EDGE ( 'NONE', *, *, #18119, .F. ) ;
#28267 = CYLINDRICAL_SURFACE ( 'NONE', #5647, 12.62506659569710266 ) ;
#28268 = CARTESIAN_POINT ( 'NONE',  ( -40.12089184044746304, 6.795442064577189356, 39.45353434682061078 ) ) ;
#28269 = EDGE_CURVE ( 'NONE', #9505, #24311, #12587, .T. ) ;
#28270 = EDGE_LOOP ( 'NONE', ( #31184, #11152, #2209 ) ) ;
#28271 = DIRECTION ( 'NONE',  ( -1.000000000000000000, 0.000000000000000000, 0.000000000000000000 ) ) ;
#28272 = CARTESIAN_POINT ( 'NONE',  ( 48.83862994770794330, 28.74118040159426002, 48.17861352429476796 ) ) ;
#28273 = CARTESIAN_POINT ( 'NONE',  ( 44.70507715278255745, 28.36291119454914877, 46.92503878583765697 ) ) ;
#28274 = ADVANCED_FACE ( 'NONE', ( #12625 ), #15551, .F. ) ;
#28275 = AXIS2_PLACEMENT_3D ( 'NONE', #8841, #21139, #3757 ) ;
#28276 = CARTESIAN_POINT ( 'NONE',  ( -39.41422314775386582, -5.935690916112652538, 77.97410326138991365 ) ) ;
#28277 = AXIS2_PLACEMENT_3D ( 'NONE', #14626, #19698, #7409 ) ;
#28278 = ADVANCED_FACE ( 'NONE', ( #25561 ), #6268, .T. ) ;
#28279 = EDGE_CURVE ( 'NONE', #12476, #8369, #18826, .T. ) ;
#28280 = ORIENTED_EDGE ( 'NONE', *, *, #1422, .F. ) ;
#28281 = CARTESIAN_POINT ( 'NONE',  ( 21.09992658989239089, 25.59143805560860940, 47.04930799450051637 ) ) ;
#28282 = DIRECTION ( 'NONE',  ( 0.000000000000000000, 0.000000000000000000, -1.000000000000000000 ) ) ;
#28283 = CIRCLE ( 'NONE', #27747, 55.85791022362053582 ) ;
#28284 = TOROIDAL_SURFACE ( 'NONE', #1536, 12.61792373059860850, 0.1249999999999999445 ) ;
#28285 = EDGE_LOOP ( 'NONE', ( #27304, #10972 ) ) ;
#28286 = DIRECTION ( 'NONE',  ( -0.000000000000000000, -1.000000000000000000, -0.000000000000000000 ) ) ;
#28287 = DIRECTION ( 'NONE',  ( -0.8746197071394243849, 0.4848096202462855997, 0.000000000000000000 ) ) ;
#28288 = EDGE_CURVE ( 'NONE', #27336, #17105, #12458, .T. ) ;
#28289 = DIRECTION ( 'NONE',  ( 0.4848096202463365034, 0.8746197071393960742, -2.220446049250302481E-16 ) ) ;
#28290 = VECTOR ( 'NONE', #16426, 1000.000000000000227 ) ;
#28291 = ORIENTED_EDGE ( 'NONE', *, *, #22572, .F. ) ;
#28292 = CIRCLE ( 'NONE', #17813, 31.30000000000002913 ) ;
#28293 = DIRECTION ( 'NONE',  ( -1.224646799147353207E-16, -1.349345573449484691E-32, 1.000000000000000000 ) ) ;
#28294 = CARTESIAN_POINT ( 'NONE',  ( 21.09785597605720042, -13.88867167006704939, 47.04930799450051637 ) ) ;
#28295 = CYLINDRICAL_SURFACE ( 'NONE', #28330, 12.00000000000000355 ) ;
#28296 = TOROIDAL_SURFACE ( 'NONE', #14146, 12.40141737965287128, 0.1249999999999993477 ) ;
#28297 = CARTESIAN_POINT ( 'NONE',  ( 8.732853799281734553, 38.56284415653841791, 47.04930799450051637 ) ) ;
#28298 = PRESENTATION_STYLE_ASSIGNMENT (( #26471 ) ) ;
#28299 = ORIENTED_EDGE ( 'NONE', *, *, #15168, .T. ) ;
#28300 = DIRECTION ( 'NONE',  ( -0.000000000000000000, 1.000000000000000000, -0.000000000000000000 ) ) ;
#28301 = DIRECTION ( 'NONE',  ( -1.000000000000000000, 0.000000000000000000, 0.000000000000000000 ) ) ;
#28302 = DIRECTION ( 'NONE',  ( 1.000000000000000000, 0.000000000000000000, 0.000000000000000000 ) ) ;
#28303 = CARTESIAN_POINT ( 'NONE',  ( 8.577447724035948795, 32.54735957529758394, 47.04930799450051637 ) ) ;
#28304 = DIRECTION ( 'NONE',  ( 1.000000000000000000, 0.000000000000000000, -1.224646799147353207E-16 ) ) ;
#28305 = ORIENTED_EDGE ( 'NONE', *, *, #17896, .F. ) ;
#28306 = CARTESIAN_POINT ( 'NONE',  ( 47.62584127360276653, 29.61482468817860436, 45.06378368935094869 ) ) ;
#28307 = CARTESIAN_POINT ( 'NONE',  ( 8.698509210239532052, 26.59164230456639899, 47.04930799450051637 ) ) ;
#28308 = CARTESIAN_POINT ( 'NONE',  ( -40.15599670534037102, 7.478908884098772525, 35.64930799450052490 ) ) ;
#28309 = ADVANCED_FACE ( 'NONE', ( #4902 ), #11005, .T. ) ;
#28310 = EDGE_LOOP ( 'NONE', ( #691, #21960, #2879, #18548 ) ) ;
#28311 = FACE_OUTER_BOUND ( 'NONE', #15466, .T. ) ;
#28312 = CARTESIAN_POINT ( 'NONE',  ( 21.09785597605718976, 6.717634499306958773, 67.32574359352868498 ) ) ;
#28313 = AXIS2_PLACEMENT_3D ( 'NONE', #24859, #25019, #2382 ) ;
#28314 = VECTOR ( 'NONE', #10893, 1000.000000000000000 ) ;
#28315 = DIRECTION ( 'NONE',  ( -1.000000000000000000, 0.000000000000000000, 0.000000000000000000 ) ) ;
#28316 = EDGE_CURVE ( 'NONE', #155, #9876, #8888, .T. ) ;
#28317 = DIRECTION ( 'NONE',  ( -0.000000000000000000, -1.000000000000000000, -0.000000000000000000 ) ) ;
#28318 = EDGE_LOOP ( 'NONE', ( #3834, #19996, #20766, #471 ) ) ;
#28319 = EDGE_LOOP ( 'NONE', ( #9863, #28581, #30040, #7708 ) ) ;
#28320 = EDGE_CURVE ( 'NONE', #25934, #15549, #18084, .T. ) ;
#28321 = CIRCLE ( 'NONE', #18848, 12.36707279061065101 ) ;
#28322 = VECTOR ( 'NONE', #28719, 999.9999999999998863 ) ;
#28323 = ORIENTED_EDGE ( 'NONE', *, *, #9064, .F. ) ;
#28324 = ADVANCED_FACE ( 'NONE', ( #26042 ), #13431, .F. ) ;
#28325 = CIRCLE ( 'NONE', #20967, 65.75844861871132707 ) ;
#28326 = CIRCLE ( 'NONE', #20973, 0.1250000000000001110 ) ;
#28327 = AXIS2_PLACEMENT_3D ( 'NONE', #3794, #8569, #854 ) ;
#28328 = DIRECTION ( 'NONE',  ( -1.000000000000000000, 0.000000000000000000, 0.000000000000000000 ) ) ;
#28329 = DIRECTION ( 'NONE',  ( 0.000000000000000000, 0.000000000000000000, 1.000000000000000000 ) ) ;
#28330 = AXIS2_PLACEMENT_3D ( 'NONE', #3168, #15818, #14165 ) ;
#28331 = ORIENTED_EDGE ( 'NONE', *, *, #21691, .T. ) ;
#28332 = DIRECTION ( 'NONE',  ( -1.000000000000000000, 0.000000000000000000, 0.000000000000000000 ) ) ;
#28333 = VERTEX_POINT ( 'NONE', #6034 ) ;
#28334 = DIRECTION ( 'NONE',  ( -1.000000000000000000, 0.000000000000000000, 0.000000000000000000 ) ) ;
#28335 = FACE_OUTER_BOUND ( 'NONE', #30477, .T. ) ;
#28336 = CARTESIAN_POINT ( 'NONE',  ( -31.70221225902718842, 2.889067130208885725, 78.90943617797866239 ) ) ;
#28337 = DIRECTION ( 'NONE',  ( -1.101824276508909887E-16, 1.000000000000000000, -0.000000000000000000 ) ) ;
#28338 = EDGE_LOOP ( 'NONE', ( #20457, #2923, #19253, #19532 ) ) ;
#28339 = CARTESIAN_POINT ( 'NONE',  ( 21.09785597605719332, -5.721341737285094098, 47.04930799450051637 ) ) ;
#28340 = ORIENTED_EDGE ( 'NONE', *, *, #2006, .T. ) ;
#28341 = CYLINDRICAL_SURFACE ( 'NONE', #11282, 32.50000000000000711 ) ;
#28342 = CARTESIAN_POINT ( 'NONE',  ( 106.0978559760576161, -5.935454207751966749, 16.07118271501087747 ) ) ;
#28343 = AXIS2_PLACEMENT_3D ( 'NONE', #10021, #12485, #25591 ) ;
#28344 = ORIENTED_EDGE ( 'NONE', *, *, #2395, .F. ) ;
#28345 = CARTESIAN_POINT ( 'NONE',  ( 47.73247023833965130, 22.99884124225578930, 45.78378261437761410 ) ) ;
#28346 = AXIS2_PLACEMENT_3D ( 'NONE', #14702, #1889, #14865 ) ;
#28347 = CARTESIAN_POINT ( 'NONE',  ( 75.19785597605721250, 14.56454579224780055, 47.04930799450051637 ) ) ;
#28348 = DIRECTION ( 'NONE',  ( -1.313185983435984691E-29, 1.000000000000000000, 3.761114140369702165E-15 ) ) ;
#28349 = DIRECTION ( 'NONE',  ( -0.1949050434465251780, 0.6797146636928681485, 0.7071067811865470176 ) ) ;
#28350 =( LENGTH_UNIT ( ) NAMED_UNIT ( * ) SI_UNIT ( .MILLI., .METRE. ) );
#28351 = VERTEX_POINT ( 'NONE', #23587 ) ;
#28352 = TOROIDAL_SURFACE ( 'NONE', #3683, 12.40141737965285529, 0.1250000000000000555 ) ;
#28353 = DIRECTION ( 'NONE',  ( -1.101824276508909887E-16, 1.000000000000000000, -0.000000000000000000 ) ) ;
#28354 = DIRECTION ( 'NONE',  ( 0.9612616959383221138, 0.2756373558169876170, 0.000000000000000000 ) ) ;
#28355 = EDGE_CURVE ( 'NONE', #9654, #16844, #31632, .T. ) ;
#28356 = ORIENTED_EDGE ( 'NONE', *, *, #28124, .F. ) ;
#28357 = VECTOR ( 'NONE', #17338, 1000.000000000000000 ) ;
#28358 = CIRCLE ( 'NONE', #18369, 0.1000000000000004774 ) ;
#28359 = DIRECTION ( 'NONE',  ( -1.101824276508909887E-16, 1.000000000000000000, -0.000000000000000000 ) ) ;
#28360 = DIRECTION ( 'NONE',  ( -0.8746197071393925215, 0.4848096202463429982, 8.676864087101709653E-18 ) ) ;
#28361 = VERTEX_POINT ( 'NONE', #7790 ) ;
#28362 = ORIENTED_EDGE ( 'NONE', *, *, #12849, .F. ) ;
#28363 = CARTESIAN_POINT ( 'NONE',  ( -12.56040783456439414, -3.386628651588886818, 102.8267921593860450 ) ) ;
#28364 = B_SPLINE_CURVE_WITH_KNOTS ( 'NONE', 3,
 ( #18570, #31385, #3480, #18891, #28927, #16437, #23510, #8259, #8420, #5960, #28596, #3154 ),
 .UNSPECIFIED., .F., .F.,
 ( 4, 2, 2, 2, 2, 4 ),
 ( 0.0003195369756188888837, 0.0003994212195236132188, 0.0004793054634283375540, 0.0005192475853806903432, 0.0005591897073330432408, 0.0006390739512377632391 ),
 .UNSPECIFIED. ) ;
#28365 = AXIS2_PLACEMENT_3D ( 'NONE', #27038, #1921, #22106 ) ;
#28366 = EDGE_CURVE ( 'NONE', #27012, #7822, #3845, .T. ) ;
#28367 = ORIENTED_EDGE ( 'NONE', *, *, #16076, .T. ) ;
#28368 = AXIS2_PLACEMENT_3D ( 'NONE', #15741, #25754, #8357 ) ;
#28369 = VERTEX_POINT ( 'NONE', #7633 ) ;
#28370 = MECHANICAL_DESIGN_GEOMETRIC_PRESENTATION_REPRESENTATION (  '', ( #23140 ), #8457 ) ;
#28371 = DIRECTION ( 'NONE',  ( -0.9612616959383205595, -0.2756373558169932236, 1.660411357259282445E-16 ) ) ;
#28372 = ORIENTED_EDGE ( 'NONE', *, *, #10985, .F. ) ;
#28373 = CARTESIAN_POINT ( 'NONE',  ( 48.77568013947721681, 22.93807716476589675, 47.29834112010470903 ) ) ;
#28374 = CARTESIAN_POINT ( 'NONE',  ( 47.17209261226641104, 29.58954579224849368, 44.97563639035409011 ) ) ;
#28375 = CARTESIAN_POINT ( 'NONE',  ( 52.99971320245913375, -5.721341737285090545, 105.3293216028873616 ) ) ;
#28376 = CARTESIAN_POINT ( 'NONE',  ( 45.28286642839709231, 26.34289516297710065, 47.97516931882780966 ) ) ;
#28377 = ORIENTED_EDGE ( 'NONE', *, *, #6998, .T. ) ;
#28378 = ORIENTED_EDGE ( 'NONE', *, *, #28861, .T. ) ;
#28379 = AXIS2_PLACEMENT_3D ( 'NONE', #22346, #30397, #10215 ) ;
#28380 = ORIENTED_EDGE ( 'NONE', *, *, #26413, .T. ) ;
#28381 = DIRECTION ( 'NONE',  ( 0.000000000000000000, 0.000000000000000000, -1.000000000000000000 ) ) ;
#28382 = CARTESIAN_POINT ( 'NONE',  ( 53.65899080383296393, 1.504766047489273451, 100.3208885721442698 ) ) ;
#28383 = CARTESIAN_POINT ( 'NONE',  ( 33.46699938050304013, 31.21183152705961206, 47.04930799450051637 ) ) ;
#28384 = LINE ( 'NONE', #5903, #24687 ) ;
#28385 = DIRECTION ( 'NONE',  ( -0.6797146636928670382, -0.1949050434465290915, -0.7071067811865470176 ) ) ;
#28386 = ORIENTED_EDGE ( 'NONE', *, *, #27020, .T. ) ;
#28387 = DIRECTION ( 'NONE',  ( 0.000000000000000000, -0.000000000000000000, -1.000000000000000000 ) ) ;
#28388 = PLANE ( 'NONE',  #27135 ) ;
#28389 = AXIS2_PLACEMENT_3D ( 'NONE', #7308, #7795, #79 ) ;
#28390 = CARTESIAN_POINT ( 'NONE',  ( 68.16890023319646730, 14.86454579224779948, 47.04930799450052348 ) ) ;
#28391 = CARTESIAN_POINT ( 'NONE',  ( 45.24946171279598417, 25.70784706826093569, 47.99220971130007740 ) ) ;
#28392 = AXIS2_PLACEMENT_3D ( 'NONE', #3547, #13572, #13099 ) ;
#28393 = ORIENTED_EDGE ( 'NONE', *, *, #5029, .T. ) ;
#28394 = CYLINDRICAL_SURFACE ( 'NONE', #11562, 40.00000000000000711 ) ;
#28395 = CARTESIAN_POINT ( 'NONE',  ( 21.09785597605719332, 30.56454579224779522, 47.04930799450051637 ) ) ;
#28396 = ADVANCED_FACE ( 'NONE', ( #554 ), #29957, .T. ) ;
#28397 = ORIENTED_EDGE ( 'NONE', *, *, #15042, .F. ) ;
#28398 = EDGE_CURVE ( 'NONE', #2267, #1400, #21475, .T. ) ;
#28399 = EDGE_CURVE ( 'NONE', #6416, #2451, #5164, .T. ) ;
#28400 = EDGE_CURVE ( 'NONE', #13414, #22288, #5484, .T. ) ;
#28401 = EDGE_CURVE ( 'NONE', #30896, #15810, #5786, .T. ) ;
#28402 = EDGE_CURVE ( 'NONE', #17364, #5196, #14167, .T. ) ;
#28403 = CIRCLE ( 'NONE', #7955, 0.1000000000000028644 ) ;
#28404 = ORIENTED_EDGE ( 'NONE', *, *, #16478, .T. ) ;
#28405 = ORIENTED_EDGE ( 'NONE', *, *, #31390, .F. ) ;
#28406 = CARTESIAN_POINT ( 'NONE',  ( 46.55854765242722237, 25.86960992152948435, 44.51792966461572831 ) ) ;
#28407 = DIRECTION ( 'NONE',  ( -1.101824276508909887E-16, 1.000000000000000000, -0.000000000000000000 ) ) ;
#28408 = CYLINDRICAL_SURFACE ( 'NONE', #17289, 43.00000000000000000 ) ;
#28409 = ORIENTED_EDGE ( 'NONE', *, *, #12036, .T. ) ;
#28410 = CIRCLE ( 'NONE', #15320, 0.09999999999999795164 ) ;
#28411 = CARTESIAN_POINT ( 'NONE',  ( -6.872792942851601694, -13.30632128221581034, 95.48546547976137333 ) ) ;
#28412 = CIRCLE ( 'NONE', #28925, 0.09999999999999815981 ) ;
#28413 = DIRECTION ( 'NONE',  ( 0.000000000000000000, 0.000000000000000000, -1.000000000000000000 ) ) ;
#28414 = DIRECTION ( 'NONE',  ( 0.000000000000000000, 0.000000000000000000, 1.000000000000000000 ) ) ;
#28415 = ORIENTED_EDGE ( 'NONE', *, *, #6149, .F. ) ;
#28416 = CARTESIAN_POINT ( 'NONE',  ( -43.64647580959332629, 1.256990871545142774, 53.64930799450051779 ) ) ;
#28417 = ORIENTED_EDGE ( 'NONE', *, *, #894, .T. ) ;
#28418 = CARTESIAN_POINT ( 'NONE',  ( 8.698509210239508960, 24.34164230456639544, 47.04930799450051637 ) ) ;
#28419 = FACE_OUTER_BOUND ( 'NONE', #27582, .T. ) ;
#28420 = CARTESIAN_POINT ( 'NONE',  ( 46.18024325840006838, 29.23016326080685445, 44.78457194432868960 ) ) ;
#28421 = CARTESIAN_POINT ( 'NONE',  ( 21.09785597605719332, -13.49020584019834601, 47.04930799450051637 ) ) ;
#28422 = CARTESIAN_POINT ( 'NONE',  ( 33.46699938050304013, 29.46183152705961206, 47.04930799450051637 ) ) ;
#28423 = APPLICATION_PROTOCOL_DEFINITION ( 'draft international standard', 'automotive_design', 1998, #10786 ) ;
#28424 = ORIENTED_EDGE ( 'NONE', *, *, #32216, .T. ) ;
#28425 = ORIENTED_EDGE ( 'NONE', *, *, #11807, .F. ) ;
#28426 = EDGE_CURVE ( 'NONE', #30888, #30637, #13211, .T. ) ;
#28427 = CARTESIAN_POINT ( 'NONE',  ( 39.08163115802605603, -13.30632128221581212, 100.0115811999271358 ) ) ;
#28428 = AXIS2_PLACEMENT_3D ( 'NONE', #17309, #12074, #27329 ) ;
#28429 = CARTESIAN_POINT ( 'NONE',  ( 21.09992658989239089, 24.34164230456639544, 47.04930799450051637 ) ) ;
#28430 = AXIS2_PLACEMENT_3D ( 'NONE', #6609, #19062, #13557 ) ;
#28431 = ORIENTED_EDGE ( 'NONE', *, *, #12198, .T. ) ;
#28432 = DIRECTION ( 'NONE',  ( 0.000000000000000000, 0.000000000000000000, 1.000000000000000000 ) ) ;
#28433 = CARTESIAN_POINT ( 'NONE',  ( 21.09785597605720042, 12.11061942510878886, 102.5807244896116401 ) ) ;
#28434 = VERTEX_POINT ( 'NONE', #17950 ) ;
#28435 = CARTESIAN_POINT ( 'NONE',  ( -40.60722745863126448, 9.415333058485023443, 34.69072935073783270 ) ) ;
#28436 = CARTESIAN_POINT ( 'NONE',  ( 45.79384627280941089, 25.06618040159426641, 49.05938063676249072 ) ) ;
#28437 = TOROIDAL_SURFACE ( 'NONE', #16888, 64.50000000000000000, 5.499019513592785735 ) ;
#28438 = CARTESIAN_POINT ( 'NONE',  ( -39.44085990154519550, -5.935843268867586175, 77.89403126197323957 ) ) ;
#28439 = EDGE_CURVE ( 'NONE', #8660, #23633, #5007, .T. ) ;
#28440 = CIRCLE ( 'NONE', #21599, 2.000000000000001776 ) ;
#28441 = EDGE_CURVE ( 'NONE', #31321, #18804, #17292, .T. ) ;
#28442 = CIRCLE ( 'NONE', #730, 0.09999999999998898659 ) ;
#28443 = VERTEX_POINT ( 'NONE', #3167 ) ;
#28444 = DIRECTION ( 'NONE',  ( 0.000000000000000000, -0.7071067811865474617, -0.7071067811865474617 ) ) ;
#28445 = DIRECTION ( 'NONE',  ( -0.2756373558169959437, 0.9612616959383197823, 0.000000000000000000 ) ) ;
#28446 = EDGE_LOOP ( 'NONE', ( #2910, #21083, #15863, #22730 ) ) ;
#28447 = AXIS2_PLACEMENT_3D ( 'NONE', #20329, #14939, #10019 ) ;
#28448 = CARTESIAN_POINT ( 'NONE',  ( -37.58300281841709989, 16.01180101885526597, 38.09144330556765112 ) ) ;
#28450 = DIRECTION ( 'NONE',  ( 0.000000000000000000, 1.000000000000000000, -0.000000000000000000 ) ) ;
#28449 = AXIS2_PLACEMENT_3D ( 'NONE', #26424, #4267, #23795 ) ;
#28451 = FACE_BOUND ( 'NONE', #4548, .T. ) ;
#28452 = ADVANCED_FACE ( 'NONE', ( #10098 ), #19397, .T. ) ;
#28453 = ORIENTED_EDGE ( 'NONE', *, *, #15558, .T. ) ;
#28454 = CARTESIAN_POINT ( 'NONE',  ( 21.09992658989238734, 38.56284415653841791, 47.04930799450051637 ) ) ;
#28455 = CARTESIAN_POINT ( 'NONE',  ( 45.85510844531590635, 10.95165879486606642, 97.72497336462666340 ) ) ;
#28456 = CARTESIAN_POINT ( 'NONE',  ( 33.50134396954518223, 32.59164230456639899, 47.04930799450051637 ) ) ;
#28457 = CIRCLE ( 'NONE', #21110, 0.1250000000000001110 ) ;
#28458 = DIRECTION ( 'NONE',  ( -1.101824276508909887E-16, 1.000000000000000000, -0.000000000000000000 ) ) ;
#28459 = B_SPLINE_CURVE_WITH_KNOTS ( 'NONE', 3,
 ( #2196, #25332, #32239, #700, #21030, #536, #10882, #28276, #13504, #10567, #23017, #17935, #20557, #30587, #5796, #5957, #7940, #15951, #15800, #13666, #25807, #3317, #8100, #25961, #27955, #13347, #28438, #18094, #23348, #2991, #20874, #859, #11044, #28122 ),
 .UNSPECIFIED., .F., .F.,
 ( 4, 3, 3, 3, 3, 3, 3, 3, 3, 3, 3, 4 ),
 ( 0.0002238713945714089102, 0.0002443349429672130708, 0.0002647477377446432801, 0.0002776748598345243793, 0.0002880592449434732339, 0.0002985192223745329241, 0.0003079983821794234989, 0.0003223271915421464210, 0.0003453054321472419971, 0.0003848690401466044967, 0.0004381801683341408253, 0.0004477427891427999311 ),
 .UNSPECIFIED. ) ;
#28460 = ORIENTED_EDGE ( 'NONE', *, *, #24432, .T. ) ;
#28461 = EDGE_CURVE ( 'NONE', #16025, #23957, #25694, .T. ) ;
#28462 = FACE_OUTER_BOUND ( 'NONE', #20, .T. ) ;
#28463 = DIRECTION ( 'NONE',  ( 1.000000000000000000, 0.000000000000000000, 0.000000000000000000 ) ) ;
#28464 = EDGE_CURVE ( 'NONE', #17233, #29191, #28325, .T. ) ;
#28465 = CARTESIAN_POINT ( 'NONE',  ( -40.38504631157857006, 8.640495317104287309, 34.64880948087299117 ) ) ;
#28466 = DIRECTION ( 'NONE',  ( -1.000000000000000000, 0.000000000000000000, 0.000000000000000000 ) ) ;
#28467 = CARTESIAN_POINT ( 'NONE',  ( 76.38709588317641419, -2.706209967030163366, 80.78504949309299832 ) ) ;
#28468 = ORIENTED_EDGE ( 'NONE', *, *, #14026, .T. ) ;
#28469 = DIRECTION ( 'NONE',  ( 0.000000000000000000, 0.000000000000000000, -1.000000000000000000 ) ) ;
#28470 = CARTESIAN_POINT ( 'NONE',  ( 21.09785597605720753, -14.54791319078308653, 105.5132833334411515 ) ) ;
#28471 = DIRECTION ( 'NONE',  ( -0.2756373558169954441, 0.9612616959383198934, -1.479773560108263451E-16 ) ) ;
#28472 = EDGE_LOOP ( 'NONE', ( #13534, #10611, #25497, #24794 ) ) ;
#28473 = CARTESIAN_POINT ( 'NONE',  ( 21.09992658989238734, 38.56284415653841791, 47.04930799450051637 ) ) ;
#28474 = DIRECTION ( 'NONE',  ( -1.101824276508909887E-16, 1.000000000000000000, -0.000000000000000000 ) ) ;
#28475 = DIRECTION ( 'NONE',  ( -0.4848096202463424431, -0.8746197071393927436, 2.220446049250312588E-16 ) ) ;
#28476 = CARTESIAN_POINT ( 'NONE',  ( -39.67555847965937943, 2.645252416024336028, 45.04930799450051637 ) ) ;
#28477 = ORIENTED_EDGE ( 'NONE', *, *, #7576, .T. ) ;
#28478 = DIRECTION ( 'NONE',  ( 0.4848096202463429427, 0.8746197071393925215, -2.352477780477436294E-16 ) ) ;
#28479 = ORIENTED_EDGE ( 'NONE', *, *, #23439, .T. ) ;
#28480 = AXIS2_PLACEMENT_3D ( 'NONE', #25057, #17004, #10131 ) ;
#28481 = ADVANCED_FACE ( 'NONE', ( #15018 ), #25018, .T. ) ;
#28482 = EDGE_LOOP ( 'NONE', ( #25678, #18348, #11034, #7803 ) ) ;
#28483 = AXIS2_PLACEMENT_3D ( 'NONE', #15002, #2363, #27792 ) ;
#28484 = CIRCLE ( 'NONE', #21644, 0.2000000000000057288 ) ;
#28485 = ADVANCED_FACE ( 'NONE', ( #27972 ), #27814, .F. ) ;
#28486 = FACE_OUTER_BOUND ( 'NONE', #17466, .T. ) ;
#28487 = CARTESIAN_POINT ( 'NONE',  ( -34.62367702067368924, -4.391527280237080610, 80.32849845693385760 ) ) ;
#28488 = DIRECTION ( 'NONE',  ( -0.000000000000000000, -1.000000000000000000, 0.000000000000000000 ) ) ;
#28489 = ADVANCED_FACE ( 'NONE', ( #12890 ), #21231, .T. ) ;
#28490 = ORIENTED_EDGE ( 'NONE', *, *, #21653, .F. ) ;
#28491 = FACE_OUTER_BOUND ( 'NONE', #12505, .T. ) ;
#28492 = VERTEX_POINT ( 'NONE', #15817 ) ;
#28493 = AXIS2_PLACEMENT_3D ( 'NONE', #3385, #10795, #20944 ) ;
#28494 = DIRECTION ( 'NONE',  ( 0.000000000000000000, -1.000000000000000000, 0.000000000000000000 ) ) ;
#28495 = DIRECTION ( 'NONE',  ( -1.000000000000000000, 0.000000000000000000, 0.000000000000000000 ) ) ;
#28496 = CARTESIAN_POINT ( 'NONE',  ( -33.33845461267002008, -1.245420574899409383, 80.62684019938389213 ) ) ;
#28497 = LINE ( 'NONE', #8474, #3719 ) ;
#28498 = ORIENTED_EDGE ( 'NONE', *, *, #12586, .F. ) ;
#28499 = EDGE_CURVE ( 'NONE', #32221, #6908, #18343, .T. ) ;
#28500 = CARTESIAN_POINT ( 'NONE',  ( -43.82034613516389498, -0.08801216882239978889, 32.04930799450052348 ) ) ;
#28501 = LINE ( 'NONE', #31605, #22078 ) ;
#28502 = DIRECTION ( 'NONE',  ( 0.000000000000000000, 0.000000000000000000, 1.000000000000000000 ) ) ;
#28503 = CARTESIAN_POINT ( 'NONE',  ( 21.09785597605719332, 48.06454579224779877, 47.04930799450051637 ) ) ;
#28504 = EDGE_CURVE ( 'NONE', #3840, #1375, #21200, .T. ) ;
#28505 = VERTEX_POINT ( 'NONE', #8741 ) ;
#28506 = DIRECTION ( 'NONE',  ( -0.000000000000000000, 1.000000000000000000, -0.000000000000000000 ) ) ;
#28507 = DIRECTION ( 'NONE',  ( -0.2756373558169932236, 0.9612616959383205595, 2.536267806945839542E-31 ) ) ;
#28508 = LINE ( 'NONE', #3226, #15911 ) ;
#28509 = ADVANCED_FACE ( 'NONE', ( #18736 ), #25823, .T. ) ;
#28510 = CIRCLE ( 'NONE', #2816, 19.25826962553310295 ) ;
#28511 = FILL_AREA_STYLE ('',( #30654 ) ) ;
#28512 = AXIS2_PLACEMENT_3D ( 'NONE', #31227, #26935, #31547 ) ;
#28513 = ORIENTED_EDGE ( 'NONE', *, *, #6527, .T. ) ;
#28514 = AXIS2_PLACEMENT_3D ( 'NONE', #10148, #20467, #7844 ) ;
#28515 = DIRECTION ( 'NONE',  ( -1.000000000000000000, 0.000000000000000000, 0.000000000000000000 ) ) ;
#28516 = DIRECTION ( 'NONE',  ( 0.000000000000000000, 0.000000000000000000, -1.000000000000000000 ) ) ;
#28517 = ORIENTED_EDGE ( 'NONE', *, *, #3442, .F. ) ;
#28518 = CARTESIAN_POINT ( 'NONE',  ( -39.85048242108726413, 2.742214340073605872, 47.04930799450051637 ) ) ;
#28519 = CARTESIAN_POINT ( 'NONE',  ( -10.01616728275229740, -5.935340315990530691, -13.57859485750651629 ) ) ;
#28520 = ORIENTED_EDGE ( 'NONE', *, *, #8193, .F. ) ;
#28521 = AXIS2_PLACEMENT_3D ( 'NONE', #6652, #16646, #27327 ) ;
#28522 = ORIENTED_EDGE ( 'NONE', *, *, #5634, .T. ) ;
#28523 = CARTESIAN_POINT ( 'NONE',  ( -12.63788552253510211, -2.706209967029991503, 102.3385479016197479 ) ) ;
#28524 = UNCERTAINTY_MEASURE_WITH_UNIT (LENGTH_MEASURE( 1.000000000000000082E-05 ), #1810, 'distance_accuracy_value', 'NONE');
#28525 = VERTEX_POINT ( 'NONE', #8271 ) ;
#28526 = VERTEX_POINT ( 'NONE', #3490 ) ;
#28527 = EDGE_CURVE ( 'NONE', #13059, #13215, #16124, .T. ) ;
#28528 = DIRECTION ( 'NONE',  ( -0.4848096202463405002, -0.8746197071393938538, 0.000000000000000000 ) ) ;
#28529 = ADVANCED_FACE ( 'NONE', ( #10896 ), #16235, .F. ) ;
#28530 = VERTEX_POINT ( 'NONE', #13519 ) ;
#28531 = CARTESIAN_POINT ( 'NONE',  ( 47.65993751833249092, 23.10527845304106620, 47.07849978535075053 ) ) ;
#28532 = DIRECTION ( 'NONE',  ( -1.000000000000000000, -1.101824276508909887E-16, 0.000000000000000000 ) ) ;
#28533 = FACE_OUTER_BOUND ( 'NONE', #19358, .T. ) ;
#28534 = CARTESIAN_POINT ( 'NONE',  ( 45.38854177497844944, 28.32622849631042783, 45.94041160078741370 ) ) ;
#28535 = ORIENTED_EDGE ( 'NONE', *, *, #7159, .F. ) ;
#28536 = ORIENTED_EDGE ( 'NONE', *, *, #12094, .T. ) ;
#28537 = CARTESIAN_POINT ( 'NONE',  ( -40.11286833322908052, 2.887657226147511302, 58.34930799450052064 ) ) ;
#28538 = ADVANCED_FACE ( 'NONE', ( #13841 ), #6449, .T. ) ;
#28539 = EDGE_LOOP ( 'NONE', ( #17264, #18507, #21058, #31575 ) ) ;
#28540 = CARTESIAN_POINT ( 'NONE',  ( 21.09992658989239089, 25.21183152705960140, 47.04930799450051637 ) ) ;
#28541 = CARTESIAN_POINT ( 'NONE',  ( 52.73954714899677754, 3.260977705924045011, 99.74023595452713664 ) ) ;
#28542 = CARTESIAN_POINT ( 'NONE',  ( 49.20081590711968289, 22.84434098701873594, 47.48251420876358964 ) ) ;
#28543 = VECTOR ( 'NONE', #1028, 1000.000000000000000 ) ;
#28544 =( BOUNDED_CURVE ( )  B_SPLINE_CURVE ( 3, ( #6247, #28732, #23958, #6411 ),
 .UNSPECIFIED., .F., .F. ) 
 B_SPLINE_CURVE_WITH_KNOTS ( ( 4, 4 ),
 ( 5.010168875603692840, 6.432075254789125118 ),
 .UNSPECIFIED. ) 
 CURVE ( )  GEOMETRIC_REPRESENTATION_ITEM ( )  RATIONAL_B_SPLINE_CURVE ( ( 1.000000000000000000, 0.8384934736035498659, 0.8384934736035498659, 1.000000000000000000 ) ) 
 REPRESENTATION_ITEM ( '' )  );
#28545 = DIRECTION ( 'NONE',  ( -1.101824276508909887E-16, 1.000000000000000000, -0.000000000000000000 ) ) ;
#28546 = FACE_OUTER_BOUND ( 'NONE', #3758, .T. ) ;
#28547 = TOROIDAL_SURFACE ( 'NONE', #3366, 58.86319174311611846, 0.1999999999999984290 ) ;
#28548 = EDGE_LOOP ( 'NONE', ( #16544, #2391, #14430, #30010 ) ) ;
#28549 = FACE_OUTER_BOUND ( 'NONE', #2439, .T. ) ;
#28550 = CARTESIAN_POINT ( 'NONE',  ( 21.09992658989239089, 24.09143805560860940, 47.04930799450051637 ) ) ;
#28551 = TOROIDAL_SURFACE ( 'NONE', #27558, 1.299999999999999822, 0.1000000000000000056 ) ;
#28552 = FACE_OUTER_BOUND ( 'NONE', #73, .T. ) ;
#28553 = AXIS2_PLACEMENT_3D ( 'NONE', #5106, #22982, #22335 ) ;
#28554 = CARTESIAN_POINT ( 'NONE',  ( 48.27628129728358886, 23.03451764446789696, 46.77839245790816847 ) ) ;
#28555 = DIRECTION ( 'NONE',  ( -0.000000000000000000, -1.000000000000000000, -0.000000000000000000 ) ) ;
#28556 = CARTESIAN_POINT ( 'NONE',  ( 45.35708200440645044, 25.59118040159426855, 45.92000246470680480 ) ) ;
#28557 = ORIENTED_EDGE ( 'NONE', *, *, #24855, .T. ) ;
#28558 = PLANE ( 'NONE',  #19899 ) ;
#28559 = CARTESIAN_POINT ( 'NONE',  ( 21.09992658989239089, 24.22145308207319303, 47.04930799450051637 ) ) ;
#28560 = VERTEX_POINT ( 'NONE', #21047 ) ;
#28561 = VECTOR ( 'NONE', #6570, 1000.000000000000000 ) ;
#28562 = EDGE_LOOP ( 'NONE', ( #26041, #16352, #14525, #23037 ) ) ;
#28563 = CIRCLE ( 'NONE', #29620, 71.99999999999998579 ) ;
#28564 = CARTESIAN_POINT ( 'NONE',  ( 47.22751897799751220, 25.84253733014356413, 44.55267275764142454 ) ) ;
#28565 = FACE_OUTER_BOUND ( 'NONE', #19638, .T. ) ;
#28567 = DIRECTION ( 'NONE',  ( -0.000000000000000000, 1.000000000000000000, -0.000000000000000000 ) ) ;
#28566 = CIRCLE ( 'NONE', #24888, 0.1250000000000001110 ) ;
#28568 = AXIS2_PLACEMENT_3D ( 'NONE', #30059, #27589, #27253 ) ;
#28569 = ORIENTED_EDGE ( 'NONE', *, *, #11811, .T. ) ;
#28570 = CARTESIAN_POINT ( 'NONE',  ( -3.635677172050070460, -13.30632128221581567, -3.117123918615727352 ) ) ;
#28571 = DIRECTION ( 'NONE',  ( -0.000000000000000000, -1.000000000000000000, 0.000000000000000000 ) ) ;
#28572 = ORIENTED_EDGE ( 'NONE', *, *, #31908, .T. ) ;
#28573 = DIRECTION ( 'NONE',  ( -0.3958453973319808195, -0.7141240004913296247, 0.5773502691896363892 ) ) ;
#28574 = EDGE_CURVE ( 'NONE', #294, #26091, #16, .T. ) ;
#28575 = ORIENTED_EDGE ( 'NONE', *, *, #711, .F. ) ;
#28576 = CARTESIAN_POINT ( 'NONE',  ( 106.0978559760576161, -5.935454207752202116, 16.07118271501088458 ) ) ;
#28577 = LINE ( 'NONE', #10863, #26469 ) ;
#28578 = EDGE_CURVE ( 'NONE', #13978, #1940, #20435, .T. ) ;
#28579 = EDGE_CURVE ( 'NONE', #24883, #20484, #13684, .T. ) ;
#28580 = CARTESIAN_POINT ( 'NONE',  ( 45.96182992765471909, 25.20087065737812182, 44.82232689504102296 ) ) ;
#28581 = ORIENTED_EDGE ( 'NONE', *, *, #29864, .T. ) ;
#28582 = EDGE_LOOP ( 'NONE', ( #13008, #8179, #32365, #9733 ) ) ;
#28583 = DIRECTION ( 'NONE',  ( -1.000000000000000000, 0.000000000000000000, 0.000000000000000000 ) ) ;
#28584 = DIRECTION ( 'NONE',  ( 7.588956326749211550E-18, -4.206627182996912454E-18, 1.000000000000000000 ) ) ;
#28585 = DIRECTION ( 'NONE',  ( -1.000000000000000000, 0.000000000000000000, 0.000000000000000000 ) ) ;
#28586 = AXIS2_PLACEMENT_3D ( 'NONE', #4425, #1956, #31999 ) ;
#28587 = VERTEX_POINT ( 'NONE', #23686 ) ;
#28588 = DIRECTION ( 'NONE',  ( -1.101824276508909887E-16, 1.000000000000000000, -0.000000000000000000 ) ) ;
#28589 = ORIENTED_EDGE ( 'NONE', *, *, #521, .F. ) ;
#28590 = CARTESIAN_POINT ( 'NONE',  ( -40.50965841522093314, 7.583953161651079355, 60.22550310247657279 ) ) ;
#28591 = CARTESIAN_POINT ( 'NONE',  ( 45.73035263060504718, 30.03954579807169978, 44.36855633853329550 ) ) ;
#28592 = AXIS2_PLACEMENT_3D ( 'NONE', #27279, #16330, #1396 ) ;
#28593 = PLANE ( 'NONE',  #23782 ) ;
#28594 = CIRCLE ( 'NONE', #291, 0.1250000000000001110 ) ;
#28595 = ORIENTED_EDGE ( 'NONE', *, *, #17256, .F. ) ;
#28596 = CARTESIAN_POINT ( 'NONE',  ( 51.92400919103565116, -5.935454207752203892, -13.58917618696519725 ) ) ;
#28597 = DIRECTION ( 'NONE',  ( -0.8746197071393790878, 0.4848096202463673676, 1.277302113040196197E-17 ) ) ;
#28598 = DIRECTION ( 'NONE',  ( -0.8746197071393926326, 0.4848096202463430537, 8.676864087101709653E-18 ) ) ;
#28599 = EDGE_LOOP ( 'NONE', ( #12827, #12008, #11212, #19386 ) ) ;
#28600 = CARTESIAN_POINT ( 'NONE',  ( 8.474859994195286461, 29.84184655352422411, 47.04930799450051637 ) ) ;
#28601 = VECTOR ( 'NONE', #7925, 1000.000000000000000 ) ;
#28602 = FACE_OUTER_BOUND ( 'NONE', #2082, .T. ) ;
#28603 = PRESENTATION_LAYER_ASSIGNMENT (  '', '', ( #10284 ) ) ;
#28604 = ORIENTED_EDGE ( 'NONE', *, *, #3982, .F. ) ;
#28605 = DIRECTION ( 'NONE',  ( 1.000000000000000000, -0.000000000000000000, -0.000000000000000000 ) ) ;
#28606 = EDGE_CURVE ( 'NONE', #14877, #9695, #8405, .T. ) ;
#28607 = CARTESIAN_POINT ( 'NONE',  ( -40.52669582637187062, 7.652910973922026017, 53.94439779120587986 ) ) ;
#28609 = EDGE_CURVE ( 'NONE', #15162, #15932, #12613, .T. ) ;
#28608 = DIRECTION ( 'NONE',  ( -1.000000000000000000, 0.000000000000000000, 0.000000000000000000 ) ) ;
#28610 = EDGE_CURVE ( 'NONE', #10609, #14793, #12875, .T. ) ;
#28611 = CARTESIAN_POINT ( 'NONE',  ( 8.474859994195286461, 26.84184655352419568, 47.04930799450051637 ) ) ;
#28612 = ADVANCED_FACE ( 'NONE', ( #10059 ), #10711, .T. ) ;
#28613 = SURFACE_SIDE_STYLE ('',( #18585 ) ) ;
#28614 = EDGE_LOOP ( 'NONE', ( #31515, #15791, #31208, #11693 ) ) ;
#28615 = DIRECTION ( 'NONE',  ( -0.000000000000000000, -1.000000000000000000, -0.000000000000000000 ) ) ;
#28617 = EDGE_CURVE ( 'NONE', #1121, #32103, #25177, .T. ) ;
#28616 = CARTESIAN_POINT ( 'NONE',  ( 48.77917452769285944, 19.86454579224779948, 50.34524002170125101 ) ) ;
#28618 = DIRECTION ( 'NONE',  ( -1.000000000000000000, 0.000000000000000000, 0.000000000000000000 ) ) ;
#28619 = DIRECTION ( 'NONE',  ( -1.000000000000000000, -1.101824276508909887E-16, 0.000000000000000000 ) ) ;
#28620 = AXIS2_PLACEMENT_3D ( 'NONE', #1302, #6078, #26416 ) ;
#28621 = DIRECTION ( 'NONE',  ( -0.000000000000000000, -1.000000000000000000, 0.000000000000000000 ) ) ;
#28622 = VERTEX_POINT ( 'NONE', #30727 ) ;
#28623 = CARTESIAN_POINT ( 'NONE',  ( 21.09992658989239089, 23.84143805560861296, 47.04930799450051637 ) ) ;
#28624 = CARTESIAN_POINT ( 'NONE',  ( 49.72013424640590529, 24.87319583719382976, 46.29665793277550279 ) ) ;
#28625 = CARTESIAN_POINT ( 'NONE',  ( -42.37913764077812573, 15.23192269303853053, 35.64930799450052490 ) ) ;
#28626 = VERTEX_POINT ( 'NONE', #5294 ) ;
#28627 = CARTESIAN_POINT ( 'NONE',  ( 72.46310410352296572, 9.702389020015065313, 20.34850893876554778 ) ) ;
#28628 = DIRECTION ( 'NONE',  ( -1.101824276508909887E-16, 1.000000000000000000, -0.000000000000000000 ) ) ;
#28629 = CARTESIAN_POINT ( 'NONE',  ( -36.15737491070432696, 8.702841779934164634, 53.64930799450051779 ) ) ;
#28630 = CARTESIAN_POINT ( 'NONE',  ( 49.03810302523404374, 8.582373042058245360, -4.360755707720810115 ) ) ;
#28631 = ORIENTED_EDGE ( 'NONE', *, *, #16744, .F. ) ;
#28632 = ORIENTED_EDGE ( 'NONE', *, *, #9538, .F. ) ;
#28633 = AXIS2_PLACEMENT_3D ( 'NONE', #8561, #25632, #8398 ) ;
#28634 = AXIS2_PLACEMENT_3D ( 'NONE', #19525, #1646, #7225 ) ;
#28635 = ORIENTED_EDGE ( 'NONE', *, *, #9064, .T. ) ;
#28636 = EDGE_CURVE ( 'NONE', #7566, #28192, #25146, .T. ) ;
#28637 = EDGE_CURVE ( 'NONE', #11200, #16822, #15299, .T. ) ;
#28638 = CIRCLE ( 'NONE', #1904, 78.39999999999999147 ) ;
#28639 = PLANE ( 'NONE',  #20745 ) ;
#28640 = CYLINDRICAL_SURFACE ( 'NONE', #16117, 0.1000000000000014905 ) ;
#28641 = CARTESIAN_POINT ( 'NONE',  ( 81.73558347630492449, -5.936245040125570860, 78.00362224660160848 ) ) ;
#28642 = ORIENTED_EDGE ( 'NONE', *, *, #20637, .F. ) ;
#28643 = CARTESIAN_POINT ( 'NONE',  ( 21.09785597605720753, -5.098646251524523443, 47.04930799450052348 ) ) ;
#28644 = ORIENTED_EDGE ( 'NONE', *, *, #27395, .T. ) ;
#28645 = FACE_OUTER_BOUND ( 'NONE', #981, .T. ) ;
#28646 = CARTESIAN_POINT ( 'NONE',  ( 21.09992658989238734, 30.84164230456639544, 47.04930799450051637 ) ) ;
#28647 = DIRECTION ( 'NONE',  ( -1.224646799147353207E-16, -1.349345573449484691E-32, 1.000000000000000000 ) ) ;
#28648 = EDGE_CURVE ( 'NONE', #90, #21602, #16770, .T. ) ;
#28649 = ORIENTED_EDGE ( 'NONE', *, *, #10730, .T. ) ;
#28650 = DIRECTION ( 'NONE',  ( -1.000000000000000000, 0.000000000000000000, 0.000000000000000000 ) ) ;
#28651 = ORIENTED_EDGE ( 'NONE', *, *, #6400, .F. ) ;
#28652 = DIRECTION ( 'NONE',  ( 1.000000000000000000, 0.000000000000000000, -1.224646799147353207E-16 ) ) ;
#28654 = FILL_AREA_STYLE_COLOUR ( '', #18939 ) ;
#28653 = CIRCLE ( 'NONE', #22341, 12.36707279061065279 ) ;
#28655 = ORIENTED_EDGE ( 'NONE', *, *, #5461, .F. ) ;
#28656 = DIRECTION ( 'NONE',  ( 0.000000000000000000, 0.000000000000000000, -1.000000000000000000 ) ) ;
#28657 = DIRECTION ( 'NONE',  ( -1.000000000000000000, 0.000000000000000000, 0.000000000000000000 ) ) ;
#28658 = CARTESIAN_POINT ( 'NONE',  ( -38.32955388700093380, 6.929907785659376707, 47.04930799450051637 ) ) ;
#28659 = CARTESIAN_POINT ( 'NONE',  ( -42.41019933908752648, 14.71530103803245915, 58.95721942880052779 ) ) ;
#28660 = DIRECTION ( 'NONE',  ( 0.4544104193609915243, 0.000000000000000000, 0.8907924397839082076 ) ) ;
#28661 = ORIENTED_EDGE ( 'NONE', *, *, #16890, .T. ) ;
#28662 = CARTESIAN_POINT ( 'NONE',  ( 21.09992658989239089, 23.65414230456639544, 47.04930799450051637 ) ) ;
#28663 = DIRECTION ( 'NONE',  ( 1.000000000000000000, 0.000000000000000000, 0.000000000000000000 ) ) ;
#28664 = EDGE_LOOP ( 'NONE', ( #28809, #27751, #10292, #26938 ) ) ;
#28665 = CARTESIAN_POINT ( 'NONE',  ( -44.16023901230963133, -5.485428030315304682, 41.32037469003774532 ) ) ;
#28666 = AXIS2_PLACEMENT_3D ( 'NONE', #19682, #27235, #14777 ) ;
#28667 = CARTESIAN_POINT ( 'NONE',  ( -40.46271621608484281, 3.081581074246047436, 48.54930799450051637 ) ) ;
#28668 = VERTEX_POINT ( 'NONE', #683 ) ;
#28669 = ADVANCED_FACE ( 'NONE', ( #12847 ), #3130, .F. ) ;
#28670 = ORIENTED_EDGE ( 'NONE', *, *, #20609, .T. ) ;
#28671 = ADVANCED_FACE ( 'NONE', ( #22838 ), #15457, .F. ) ;
#28672 = ORIENTED_EDGE ( 'NONE', *, *, #18119, .T. ) ;
#28673 = EDGE_CURVE ( 'NONE', #9336, #13719, #20367, .T. ) ;
#28674 = AXIS2_PLACEMENT_3D ( 'NONE', #5983, #13696, #28780 ) ;
#28675 = EDGE_CURVE ( 'NONE', #16288, #27795, #2642, .T. ) ;
#28676 = EDGE_CURVE ( 'NONE', #26626, #16357, #11036, .T. ) ;
#28677 = VERTEX_POINT ( 'NONE', #20215 ) ;
#28678 = FACE_OUTER_BOUND ( 'NONE', #988, .T. ) ;
#28679 = VERTEX_POINT ( 'NONE', #30239 ) ;
#28680 = DIRECTION ( 'NONE',  ( -1.224646799147353207E-16, -1.349345573449484691E-32, 1.000000000000000000 ) ) ;
#28681 = DIRECTION ( 'NONE',  ( -1.224646799147353207E-16, -1.349345573449484691E-32, 1.000000000000000000 ) ) ;
#28682 = DIRECTION ( 'NONE',  ( 0.000000000000000000, 0.000000000000000000, 1.000000000000000000 ) ) ;
#28683 = CARTESIAN_POINT ( 'NONE',  ( 44.74832014356462651, 27.68456182964376566, 46.92728461490987257 ) ) ;
#28684 = EDGE_CURVE ( 'NONE', #7619, #17055, #23585, .T. ) ;
#28685 = ORIENTED_EDGE ( 'NONE', *, *, #30304, .T. ) ;
#28686 = VERTEX_POINT ( 'NONE', #13170 ) ;
#28687 = CARTESIAN_POINT ( 'NONE',  ( 21.09785597605719332, 25.56454579224780232, 126.2593585008393831 ) ) ;
#28688 = ORIENTED_EDGE ( 'NONE', *, *, #15526, .T. ) ;
#28689 = CARTESIAN_POINT ( 'NONE',  ( 8.698509210239581790, 31.84164230456639544, 47.04930799450051637 ) ) ;
#28690 = CARTESIAN_POINT ( 'NONE',  ( -40.70098307446854591, 6.778209214780407166, 39.41092630925031415 ) ) ;
#28691 = DIRECTION ( 'NONE',  ( -1.101824276508909887E-16, 1.000000000000000000, -0.000000000000000000 ) ) ;
#28692 = VECTOR ( 'NONE', #13800, 1000.000000000000000 ) ;
#28693 = DIRECTION ( 'NONE',  ( 0.000000000000000000, 0.000000000000000000, -1.000000000000000000 ) ) ;
#28694 = FACE_OUTER_BOUND ( 'NONE', #31201, .T. ) ;
#28695 = ORIENTED_EDGE ( 'NONE', *, *, #23612, .T. ) ;
#28696 = DIRECTION ( 'NONE',  ( -1.000000000000000000, 0.000000000000000000, 0.000000000000000000 ) ) ;
#28697 = DIRECTION ( 'NONE',  ( -0.8746197071393925215, 0.4848096202463429982, 8.676864087101709653E-18 ) ) ;
#28698 = CIRCLE ( 'NONE', #32362, 0.1250000000000001110 ) ;
#28699 = DIRECTION ( 'NONE',  ( -0.2756373558169973870, 0.9612616959383193382, 1.315048337272770435E-17 ) ) ;
#28700 = TOROIDAL_SURFACE ( 'NONE', #3079, 0.8928932188134564019, 0.1000000000000000056 ) ;
#28701 = DIRECTION ( 'NONE',  ( -1.000000000000000000, 0.000000000000000000, 0.000000000000000000 ) ) ;
#28702 = DIRECTION ( 'NONE',  ( -1.101824276508909887E-16, 1.000000000000000000, -0.000000000000000000 ) ) ;
#28703 = ORIENTED_EDGE ( 'NONE', *, *, #18469, .F. ) ;
#28704 = CARTESIAN_POINT ( 'NONE',  ( 45.35708200440645044, 26.99118040159426357, 45.92000246470680480 ) ) ;
#28705 = AXIS2_PLACEMENT_3D ( 'NONE', #29105, #32381, #6618 ) ;
#28706 = ADVANCED_FACE ( 'NONE', ( #20054 ), #31971, .T. ) ;
#28707 = EDGE_LOOP ( 'NONE', ( #24928, #16759, #31286, #29527 ) ) ;
#28708 = CARTESIAN_POINT ( 'NONE',  ( 21.09785597605720753, -5.098646251524523443, 47.04930799450052348 ) ) ;
#28709 = CARTESIAN_POINT ( 'NONE',  ( -40.65487266620045403, 9.475231293617264683, 35.46144002885649371 ) ) ;
#28710 = EDGE_CURVE ( 'NONE', #4802, #1140, #3657, .T. ) ;
#28711 = CIRCLE ( 'NONE', #5118, 36.51080762834750715 ) ;
#28712 = ORIENTED_EDGE ( 'NONE', *, *, #26871, .T. ) ;
#28713 = ADVANCED_FACE ( 'NONE', ( #22508 ), #3622, .T. ) ;
#28714 = ADVANCED_FACE ( 'NONE', ( #30085 ), #2116, .T. ) ;
#28715 = ORIENTED_EDGE ( 'NONE', *, *, #1294, .T. ) ;
#28716 = CARTESIAN_POINT ( 'NONE',  ( 48.23388202445966044, 25.55087065737811969, 49.27628909396054979 ) ) ;
#28717 = AXIS2_PLACEMENT_3D ( 'NONE', #6877, #3922, #29192 ) ;
#28718 = CARTESIAN_POINT ( 'NONE',  ( 21.09992658989239089, 26.96664230456639899, 47.04930799450051637 ) ) ;
#28719 = DIRECTION ( 'NONE',  ( -0.9612616959383207815, -0.2756373558169926685, -8.795445018804289444E-19 ) ) ;
#28720 = AXIS2_PLACEMENT_3D ( 'NONE', #16006, #31116, #27842 ) ;
#28721 = ORIENTED_EDGE ( 'NONE', *, *, #2840, .F. ) ;
#28722 = AXIS2_PLACEMENT_3D ( 'NONE', #19891, #29430, #11866 ) ;
#28723 = CARTESIAN_POINT ( 'NONE',  ( 13.79206092585403454, -13.30632128221581212, -8.403770473392276230 ) ) ;
#28724 =( BOUNDED_CURVE ( )  B_SPLINE_CURVE ( 3, ( #29285, #19429, #18770, #24354 ),
 .UNSPECIFIED., .F., .F. ) 
 B_SPLINE_CURVE_WITH_KNOTS ( ( 4, 4 ),
 ( 4.712388980384689674, 5.234911742780512967 ),
 .UNSPECIFIED. ) 
 CURVE ( )  GEOMETRIC_REPRESENTATION_ITEM ( )  RATIONAL_B_SPLINE_CURVE ( ( 1.000000000000000000, 0.9773766218953314766, 0.9773766218953314766, 1.000000000000000000 ) ) 
 REPRESENTATION_ITEM ( '' )  );
#28725 = CIRCLE ( 'NONE', #22955, 0.1250000000000001110 ) ;
#28726 = CARTESIAN_POINT ( 'NONE',  ( 21.09992658989239089, 23.59164230456639544, 47.04930799450051637 ) ) ;
#28727 = CARTESIAN_POINT ( 'NONE',  ( 72.46537437338240295, 9.162376348828955130, 19.70867165547888789 ) ) ;
#28728 = ORIENTED_EDGE ( 'NONE', *, *, #11051, .T. ) ;
#28729 = DIRECTION ( 'NONE',  ( -1.101824276508909887E-16, 1.000000000000000000, -0.000000000000000000 ) ) ;
#28730 = EDGE_LOOP ( 'NONE', ( #30117, #1743, #13627, #13112 ) ) ;
#28731 = AXIS2_PLACEMENT_3D ( 'NONE', #14970, #12682, #24972 ) ;
#28732 = CARTESIAN_POINT ( 'NONE',  ( -42.48853158357926674, 14.65761848575743898, 58.96871121695127016 ) ) ;
#28733 = DIRECTION ( 'NONE',  ( 0.000000000000000000, 0.000000000000000000, 1.000000000000000000 ) ) ;
#28734 = FACE_OUTER_BOUND ( 'NONE', #24529, .T. ) ;
#28735 = SURFACE_SIDE_STYLE ('',( #25787 ) ) ;
#28736 = EDGE_LOOP ( 'NONE', ( #26113, #3615, #16397, #8396 ) ) ;
#28737 = EDGE_LOOP ( 'NONE', ( #28323, #21676, #21980, #7541 ) ) ;
#28738 = LINE ( 'NONE', #11029, #27058 ) ;
#28739 = FACE_OUTER_BOUND ( 'NONE', #9425, .T. ) ;
#28740 = EDGE_LOOP ( 'NONE', ( #27179, #20088, #6191, #30431 ) ) ;
#28741 = CARTESIAN_POINT ( 'NONE',  ( 33.71785032049137243, 25.21664230456640254, 47.04930799450051637 ) ) ;
#28742 = FACE_OUTER_BOUND ( 'NONE', #4003, .T. ) ;
#28743 = VERTEX_POINT ( 'NONE', #1477 ) ;
#28744 = DIRECTION ( 'NONE',  ( -0.8746197071393926326, 0.4848096202463430537, 8.676864087101709653E-18 ) ) ;
#28745 = CARTESIAN_POINT ( 'NONE',  ( 50.10320668408830613, 27.00621246473837544, 47.20539118556276037 ) ) ;
#28746 = AXIS2_PLACEMENT_3D ( 'NONE', #13032, #7460, #15006 ) ;
#28747 = VECTOR ( 'NONE', #1544, 1000.000000000000227 ) ;
#28748 = CIRCLE ( 'NONE', #14600, 2.000000000000001776 ) ;
#28749 = CARTESIAN_POINT ( 'NONE',  ( 33.50134396954523908, 27.84164230456639544, 47.04930799450051637 ) ) ;
#28750 = AXIS2_PLACEMENT_3D ( 'NONE', #1973, #12161, #14463 ) ;
#28751 = AXIS2_PLACEMENT_3D ( 'NONE', #2396, #10112, #32107 ) ;
#28752 = ADVANCED_FACE ( 'NONE', ( #28734 ), #3301, .F. ) ;
#28753 = TOROIDAL_SURFACE ( 'NONE', #8839, 12.40141737965287305, 0.1250000000000000833 ) ;
#28754 = EDGE_LOOP ( 'NONE', ( #16246, #26745, #32064, #3193 ) ) ;
#28755 = ADVANCED_FACE ( 'NONE', ( #1002 ), #16092, .F. ) ;
#28756 = CYLINDRICAL_SURFACE ( 'NONE', #6717, 0.1000000000000028644 ) ;
#28757 = DIRECTION ( 'NONE',  ( -1.101824276508909887E-16, 1.000000000000000000, -0.000000000000000000 ) ) ;
#28758 = CARTESIAN_POINT ( 'NONE',  ( 48.40186567930498285, 29.61618040159425647, 45.03923535223908203 ) ) ;
#28759 = ORIENTED_EDGE ( 'NONE', *, *, #6523, .F. ) ;
#28760 = DIRECTION ( 'NONE',  ( 0.4544104193609903586, 0.000000000000000000, 0.8907924397839087627 ) ) ;
#28761 = CYLINDRICAL_SURFACE ( 'NONE', #4097, 12.36707279061065101 ) ;
#28762 = AXIS2_PLACEMENT_3D ( 'NONE', #26051, #28680, #3733 ) ;
#28763 = AXIS2_PLACEMENT_3D ( 'NONE', #7118, #22042, #19583 ) ;
#28764 = ORIENTED_EDGE ( 'NONE', *, *, #14421, .T. ) ;
#28765 = CARTESIAN_POINT ( 'NONE',  ( 45.00053793792376666, 26.53655426599985745, 45.68869892245983522 ) ) ;
#28766 = CIRCLE ( 'NONE', #5649, 19.21451602543517367 ) ;
#28767 = CARTESIAN_POINT ( 'NONE',  ( -40.18454328187963398, 7.548069831825862330, 60.44930799450051495 ) ) ;
#28768 = DIRECTION ( 'NONE',  ( 0.000000000000000000, 0.000000000000000000, -1.000000000000000000 ) ) ;
#28769 = CYLINDRICAL_SURFACE ( 'NONE', #6883, 0.1000000000000014905 ) ;
#28770 =( NAMED_UNIT ( * ) SI_UNIT ( $, .STERADIAN. ) SOLID_ANGLE_UNIT ( ) );
#28771 = ORIENTED_EDGE ( 'NONE', *, *, #9626, .T. ) ;
#28772 = DIRECTION ( 'NONE',  ( 1.188208965918164993E-16, 1.880121038077812639E-16, 1.000000000000000000 ) ) ;
#28773 = CARTESIAN_POINT ( 'NONE',  ( 46.99023568444673771, 27.13791119454915446, 49.12151524109405898 ) ) ;
#28774 = B_SPLINE_CURVE_WITH_KNOTS ( 'NONE', 3,
 ( #23366, #30604, #10417, #13368, #235, #10898, #23035, #18265, #12892, #20896, #18428, #15498 ),
 .UNSPECIFIED., .F., .F.,
 ( 4, 2, 2, 2, 2, 4 ),
 ( 0.0003422200191418650270, 0.002082436906217388032, 0.003822653793292911037, 0.005562870680368433608, 0.006432979123906195328, 0.007303087567443957047 ),
 .UNSPECIFIED. ) ;
#28775 = DIRECTION ( 'NONE',  ( -1.000000000000000000, -1.101824276508909887E-16, 0.000000000000000000 ) ) ;
#28776 = CARTESIAN_POINT ( 'NONE',  ( -41.56459318755936749, 7.281738416154046156, 60.54930799450051637 ) ) ;
#28777 = VECTOR ( 'NONE', #22120, 999.9999999999998863 ) ;
#28778 = DIRECTION ( 'NONE',  ( -0.000000000000000000, -1.000000000000000000, 0.000000000000000000 ) ) ;
#28779 = EDGE_LOOP ( 'NONE', ( #31534, #31058 ) ) ;
#28780 = DIRECTION ( 'NONE',  ( -1.000000000000000000, 0.000000000000000000, 0.000000000000000000 ) ) ;
#28781 = DIRECTION ( 'NONE',  ( -2.472450503250596893E-15, -7.226442137580869828E-16, 1.000000000000000000 ) ) ;
#28782 = CARTESIAN_POINT ( 'NONE',  ( 21.09992658989239089, 30.46664230456641675, 47.04930799450051637 ) ) ;
#28783 = ORIENTED_EDGE ( 'NONE', *, *, #8371, .T. ) ;
#28784 = DIRECTION ( 'NONE',  ( -0.8746197071393926326, 0.4848096202463430537, 8.676864087101709653E-18 ) ) ;
#28785 = CARTESIAN_POINT ( 'NONE',  ( 21.09785597605719332, 17.16451738380053627, 34.36516646732340519 ) ) ;
#28786 = DIRECTION ( 'NONE',  ( 0.000000000000000000, 0.000000000000000000, -1.000000000000000000 ) ) ;
#28787 = CARTESIAN_POINT ( 'NONE',  ( 47.79865503179234310, 9.702389020015065313, 97.45038561958638468 ) ) ;
#28788 = VERTEX_POINT ( 'NONE', #21327 ) ;
#28789 = CARTESIAN_POINT ( 'NONE',  ( 48.35060479220636154, 22.84434098701873950, 48.79307647092393552 ) ) ;
#28790 = ORIENTED_EDGE ( 'NONE', *, *, #23114, .F. ) ;
#28791 = CIRCLE ( 'NONE', #13591, 0.1249999999999931721 ) ;
#28793 = EDGE_CURVE ( 'NONE', #24444, #17822, #29654, .T. ) ;
#28792 = AXIS2_PLACEMENT_3D ( 'NONE', #18756, #19737, #14344 ) ;
#28794 = ORIENTED_EDGE ( 'NONE', *, *, #1993, .F. ) ;
#28795 = EDGE_CURVE ( 'NONE', #7978, #28788, #24136, .T. ) ;
#28796 = ADVANCED_FACE ( 'NONE', ( #26275 ), #26766, .T. ) ;
#28797 = EDGE_CURVE ( 'NONE', #28668, #19852, #8395, .T. ) ;
#28798 = EDGE_CURVE ( 'NONE', #30715, #15904, #19319, .T. ) ;
#28799 = EDGE_CURVE ( 'NONE', #5512, #21772, #15792, .T. ) ;
#28800 = AXIS2_PLACEMENT_3D ( 'NONE', #212, #29761, #2353 ) ;
#28801 = CIRCLE ( 'NONE', #10477, 0.5999999999999980904 ) ;
#28802 = CIRCLE ( 'NONE', #16749, 0.7000000000000061728 ) ;
#28803 = CYLINDRICAL_SURFACE ( 'NONE', #8199, 12.62506659569710266 ) ;
#28804 = CARTESIAN_POINT ( 'NONE',  ( -34.43190828144128091, -4.192658519183404486, 80.43389084567178315 ) ) ;
#28805 = CARTESIAN_POINT ( 'NONE',  ( 21.09785597605719332, 11.92558985988973497, 47.04930799450051637 ) ) ;
#28806 = AXIS2_PLACEMENT_3D ( 'NONE', #5505, #8131, #25520 ) ;
#28807 = ORIENTED_EDGE ( 'NONE', *, *, #31216, .F. ) ;
#28808 = CARTESIAN_POINT ( 'NONE',  ( -42.48178708409979265, 14.60617548783703690, 55.10133939125226021 ) ) ;
#28809 = ORIENTED_EDGE ( 'NONE', *, *, #19783, .F. ) ;
#28810 = DIRECTION ( 'NONE',  ( -0.000000000000000000, -1.000000000000000000, 0.000000000000000000 ) ) ;
#28811 = DIRECTION ( 'NONE',  ( 0.000000000000000000, 0.000000000000000000, -1.000000000000000000 ) ) ;
#28812 = ADVANCED_FACE ( 'NONE', ( #25785 ), #13334, .T. ) ;
#28813 = CARTESIAN_POINT ( 'NONE',  ( -39.85048242108726413, 2.742214340073605872, 47.04930799450051637 ) ) ;
#28814 = ORIENTED_EDGE ( 'NONE', *, *, #20892, .T. ) ;
#28815 = DIRECTION ( 'NONE',  ( -0.9612616959383221138, -0.2756373558169876170, 0.000000000000000000 ) ) ;
#28816 = DIRECTION ( 'NONE',  ( -0.000000000000000000, -1.000000000000000000, 0.000000000000000000 ) ) ;
#28817 = CARTESIAN_POINT ( 'NONE',  ( 8.590256034766447613, 23.65414230456639544, 47.04930799450051637 ) ) ;
#28818 = DIRECTION ( 'NONE',  ( -1.000000000000000000, 0.000000000000000000, 0.000000000000000000 ) ) ;
#28819 = AXIS2_PLACEMENT_3D ( 'NONE', #30761, #25663, #3335 ) ;
#28820 = EDGE_LOOP ( 'NONE', ( #16883, #5304, #14991, #11966 ) ) ;
#28821 = LINE ( 'NONE', #25028, #10610 ) ;
#28822 = CARTESIAN_POINT ( 'NONE',  ( 21.09785597605719332, 25.56454579224779877, 47.04930799450051637 ) ) ;
#28823 = DIRECTION ( 'NONE',  ( -1.000000000000000000, -1.101824276508909887E-16, 0.000000000000000000 ) ) ;
#28824 = PLANE ( 'NONE',  #15369 ) ;
#28825 = EDGE_LOOP ( 'NONE', ( #23760, #14055, #29497, #22747 ) ) ;
#28826 = DIRECTION ( 'NONE',  ( -1.000000000000000000, 0.000000000000000000, 0.000000000000000000 ) ) ;
#28827 = CARTESIAN_POINT ( 'NONE',  ( -40.60023598829667435, 7.576973264584798251, 35.33853321918559942 ) ) ;
#28828 = VERTEX_POINT ( 'NONE', #28422 ) ;
#28830 = EDGE_CURVE ( 'NONE', #30606, #8039, #5936, .T. ) ;
#28829 = LINE ( 'NONE', #3720, #24013 ) ;
#28831 = AXIS2_PLACEMENT_3D ( 'NONE', #14569, #29339, #30003 ) ;
#28832 = VECTOR ( 'NONE', #30555, 1000.000000000000000 ) ;
#28833 = CARTESIAN_POINT ( 'NONE',  ( 45.96182992765471909, 25.20087065737812182, 44.82232689504102296 ) ) ;
#28834 = ORIENTED_EDGE ( 'NONE', *, *, #1202, .T. ) ;
#28835 = VECTOR ( 'NONE', #2820, 1000.000000000000000 ) ;
#28836 = ORIENTED_EDGE ( 'NONE', *, *, #11365, .F. ) ;
#28837 = VECTOR ( 'NONE', #7348, 1000.000000000000227 ) ;
#28838 = AXIS2_PLACEMENT_3D ( 'NONE', #17111, #9251, #4650 ) ;
#28839 = EDGE_LOOP ( 'NONE', ( #21864, #12395, #13316, #951 ) ) ;
#28840 = AXIS2_PLACEMENT_3D ( 'NONE', #11514, #22001, #19542 ) ;
#28841 = EDGE_CURVE ( 'NONE', #27647, #20897, #5805, .T. ) ;
#28842 = AXIS2_PLACEMENT_3D ( 'NONE', #15937, #25944, #22996 ) ;
#28843 = ORIENTED_EDGE ( 'NONE', *, *, #10274, .F. ) ;
#28844 = DIRECTION ( 'NONE',  ( -1.101824276508909887E-16, 1.000000000000000000, -0.000000000000000000 ) ) ;
#28845 = AXIS2_PLACEMENT_3D ( 'NONE', #15699, #25719, #13261 ) ;
#28846 = CONICAL_SURFACE ( 'NONE', #31471, 39.63553620740810857, 0.6632251157578421541 ) ;
#28847 = EDGE_LOOP ( 'NONE', ( #7645, #24775, #12025, #26672 ) ) ;
#28848 = FACE_OUTER_BOUND ( 'NONE', #23384, .T. ) ;
#28849 = DIRECTION ( 'NONE',  ( -1.000000000000000000, 0.000000000000000000, 0.000000000000000000 ) ) ;
#28850 = AXIS2_PLACEMENT_3D ( 'NONE', #30044, #27899, #3093 ) ;
#28851 = FACE_OUTER_BOUND ( 'NONE', #4911, .T. ) ;
#28852 = CARTESIAN_POINT ( 'NONE',  ( -40.41647043964083252, 8.356895951721261540, 54.44930799450051495 ) ) ;
#28853 = CARTESIAN_POINT ( 'NONE',  ( 45.81741271322955100, 27.14452976649964810, 49.02305402274571122 ) ) ;
#28854 = AXIS2_PLACEMENT_3D ( 'NONE', #12269, #9963, #15211 ) ;
#28855 = VECTOR ( 'NONE', #31340, 1000.000000000000000 ) ;
#28856 = ORIENTED_EDGE ( 'NONE', *, *, #14987, .T. ) ;
#28857 = EDGE_LOOP ( 'NONE', ( #25121, #20188, #10503, #7996 ) ) ;
#28858 = CARTESIAN_POINT ( 'NONE',  ( 21.09992658989238734, 30.96183152705961206, 47.04930799450051637 ) ) ;
#28859 = VERTEX_POINT ( 'NONE', #23489 ) ;
#28861 = EDGE_CURVE ( 'NONE', #21198, #28587, #544, .T. ) ;
#28860 = DIRECTION ( 'NONE',  ( -1.000000000000000000, 0.000000000000000000, 0.000000000000000000 ) ) ;
#28862 = CARTESIAN_POINT ( 'NONE',  ( 21.09785597605719332, -15.93545420775219945, 119.0493079945005093 ) ) ;
#28863 = DIRECTION ( 'NONE',  ( -2.779292025043186357E-18, 1.288349127009862057E-17, -1.000000000000000000 ) ) ;
#28864 = FACE_BOUND ( 'NONE', #21244, .T. ) ;
#28865 = CARTESIAN_POINT ( 'NONE',  ( 49.28428300279882990, 27.64787913140504116, 48.46772541801551171 ) ) ;
#28866 = CARTESIAN_POINT ( 'NONE',  ( 0.1369267683895796783, 11.91444431924556469, -5.596515685912667237 ) ) ;
#28867 = DIRECTION ( 'NONE',  ( -1.101824276508909887E-16, 1.000000000000000000, -0.000000000000000000 ) ) ;
#28868 = EDGE_LOOP ( 'NONE', ( #22864, #13602, #29034, #4047 ) ) ;
#28869 = B_SPLINE_CURVE_WITH_KNOTS ( 'NONE', 3,
 ( #29116, #6631, #26646, #31744, #9254, #7287 ),
 .UNSPECIFIED., .F., .F.,
 ( 4, 2, 4 ),
 ( 0.000000000000000000, 0.5000000000000000000, 1.000000000000000000 ),
 .UNSPECIFIED. ) ;
#28870 = DIRECTION ( 'NONE',  ( -1.101824276508909887E-16, 1.000000000000000000, -0.000000000000000000 ) ) ;
#28872 = ADVANCED_FACE ( 'NONE', ( #29555 ), #28352, .T. ) ;
#28871 = DIRECTION ( 'NONE',  ( -0.4441739386572047255, 0.2110602665713113557, -0.8707256032141197366 ) ) ;
#28873 = CIRCLE ( 'NONE', #13156, 12.36707279061065101 ) ;
#28874 = DIRECTION ( 'NONE',  ( -1.101824276508909887E-16, 1.000000000000000000, -0.000000000000000000 ) ) ;
#28875 = EDGE_CURVE ( 'NONE', #24589, #3003, #2137, .T. ) ;
#28876 = DIRECTION ( 'NONE',  ( -1.101824276508909887E-16, 1.000000000000000000, -0.000000000000000000 ) ) ;
#28877 = CARTESIAN_POINT ( 'NONE',  ( 21.09992658989238734, 38.56284415653841791, 47.04930799450051637 ) ) ;
#28878 = VERTEX_POINT ( 'NONE', #31690 ) ;
#28879 = CARTESIAN_POINT ( 'NONE',  ( -40.68535844407768565, 8.206233278606877235, 54.52001867261917312 ) ) ;
#28880 = VERTEX_POINT ( 'NONE', #22146 ) ;
#28881 = DIRECTION ( 'NONE',  ( -0.000000000000000000, -1.000000000000000000, -0.000000000000000000 ) ) ;
#28882 = DIRECTION ( 'NONE',  ( 0.2756373558169958327, -0.9612616959383198934, 0.000000000000000000 ) ) ;
#28883 = AXIS2_PLACEMENT_3D ( 'NONE', #11415, #6333, #8642 ) ;
#28884 = ORIENTED_EDGE ( 'NONE', *, *, #31023, .F. ) ;
#28885 = AXIS2_PLACEMENT_3D ( 'NONE', #13300, #13132, #26235 ) ;
#28886 = VECTOR ( 'NONE', #192, 999.9999999999998863 ) ;
#28887 = TOROIDAL_SURFACE ( 'NONE', #14731, 64.50000000000000000, 5.499019513592785735 ) ;
#28888 = EDGE_CURVE ( 'NONE', #5554, #19454, #30432, .T. ) ;
#28889 = EDGE_LOOP ( 'NONE', ( #28930, #3884, #1414, #21708 ) ) ;
#28890 = DIRECTION ( 'NONE',  ( -1.101824276508909887E-16, 1.000000000000000000, -0.000000000000000000 ) ) ;
#28891 = DIRECTION ( 'NONE',  ( -2.779292025043186357E-18, 1.288349127009862211E-17, -1.000000000000000000 ) ) ;
#28892 = DIRECTION ( 'NONE',  ( -0.000000000000000000, -1.000000000000000000, -0.000000000000000000 ) ) ;
#28893 = AXIS2_PLACEMENT_3D ( 'NONE', #24080, #21615, #1600 ) ;
#28894 = VERTEX_POINT ( 'NONE', #6902 ) ;
#28895 = CARTESIAN_POINT ( 'NONE',  ( -32.92991496113891259, -13.30632128221581212, 61.52060788219944953 ) ) ;
#28896 = CARTESIAN_POINT ( 'NONE',  ( -36.45222641229887017, 9.925589859889722533, 42.04930799450051637 ) ) ;
#28897 = DIRECTION ( 'NONE',  ( 0.000000000000000000, 0.000000000000000000, 1.000000000000000000 ) ) ;
#28898 = ADVANCED_FACE ( 'NONE', ( #29713 ), #15758, .T. ) ;
#28899 = ORIENTED_EDGE ( 'NONE', *, *, #20642, .F. ) ;
#28900 = CARTESIAN_POINT ( 'NONE',  ( -40.46271621608484281, 3.081581074246047436, 47.04930799450051637 ) ) ;
#28901 = ORIENTED_EDGE ( 'NONE', *, *, #5121, .F. ) ;
#28902 = ADVANCED_FACE ( 'NONE', ( #11989 ), #14782, .F. ) ;
#28903 = CARTESIAN_POINT ( 'NONE',  ( 21.09785597605719332, -15.93545420775219945, 47.04930799450051637 ) ) ;
#28904 = CARTESIAN_POINT ( 'NONE',  ( 45.84097905237065618, 22.86454579224779948, 48.98672734302541443 ) ) ;
#28905 = DIRECTION ( 'NONE',  ( -1.000000000000000000, -1.101824276508909887E-16, 0.000000000000000000 ) ) ;
#28906 = AXIS2_PLACEMENT_3D ( 'NONE', #19927, #2046, #9770 ) ;
#28907 = SHAPE_REPRESENTATION_RELATIONSHIP ( 'NONE' , 'NONE' ,  #28161, #18649 ) ;
#28908 = EDGE_LOOP ( 'NONE', ( #18465, #23013, #32419, #18014 ) ) ;
#28909 = EDGE_LOOP ( 'NONE', ( #24209, #2951, #12296, #7014 ) ) ;
#28910 = CIRCLE ( 'NONE', #1649, 12.62506659569710266 ) ;
#28911 = DIRECTION ( 'NONE',  ( 0.2756373558170082672, -0.9612616959383162296, 0.000000000000000000 ) ) ;
#28912 = AXIS2_PLACEMENT_3D ( 'NONE', #20787, #15384, #10306 ) ;
#28913 = EDGE_CURVE ( 'NONE', #15199, #31427, #9199, .T. ) ;
#28914 = EDGE_CURVE ( 'NONE', #29694, #30888, #19191, .T. ) ;
#28915 = DIRECTION ( 'NONE',  ( 0.000000000000000000, -1.000000000000000000, 0.000000000000000000 ) ) ;
#28916 = EDGE_LOOP ( 'NONE', ( #24227, #24172, #8751, #9712 ) ) ;
#28917 = CARTESIAN_POINT ( 'NONE',  ( -12.31990217110675800, -4.114116020023733888, -9.341889586185132544 ) ) ;
#28918 = CARTESIAN_POINT ( 'NONE',  ( 79.32175637497276455, -13.74047052604243646, 43.23856262457181998 ) ) ;
#28919 = ORIENTED_EDGE ( 'NONE', *, *, #3442, .T. ) ;
#28920 = CARTESIAN_POINT ( 'NONE',  ( 33.62240545574881878, 32.54735957529758394, 47.04930799450051637 ) ) ;
#28921 = CARTESIAN_POINT ( 'NONE',  ( 44.09250526802607340, 30.15621246473836692, 46.89322480343881949 ) ) ;
#28922 = TOROIDAL_SURFACE ( 'NONE', #14767, 12.68414152717710763, 0.1999999999999992339 ) ;
#28923 = FACE_OUTER_BOUND ( 'NONE', #21021, .T. ) ;
#28924 = ORIENTED_EDGE ( 'NONE', *, *, #11629, .T. ) ;
#28925 = AXIS2_PLACEMENT_3D ( 'NONE', #27127, #2017, #30252 ) ;
#28926 = DIRECTION ( 'NONE',  ( -1.000000000000000000, 0.000000000000000000, 0.000000000000000000 ) ) ;
#28927 = CARTESIAN_POINT ( 'NONE',  ( 52.03879352760534260, -5.936629510748245409, -13.61281336867091696 ) ) ;
#28928 = CARTESIAN_POINT ( 'NONE',  ( 46.55854765242722237, 28.66960992152947085, 44.51792966461572121 ) ) ;
#28929 = CARTESIAN_POINT ( 'NONE',  ( 47.20353132263855400, 26.15286309983298807, 45.01455027646041174 ) ) ;
#28930 = ORIENTED_EDGE ( 'NONE', *, *, #12349, .F. ) ;
#28931 = DIRECTION ( 'NONE',  ( 0.2756373558170093774, -0.9612616959383158965, 0.000000000000000000 ) ) ;
#28932 = FACE_OUTER_BOUND ( 'NONE', #14566, .T. ) ;
#28933 = EDGE_CURVE ( 'NONE', #25766, #893, #15243, .T. ) ;
#28934 = CIRCLE ( 'NONE', #23173, 0.1250000000000001110 ) ;
#28935 = EDGE_CURVE ( 'NONE', #8568, #30811, #11666, .T. ) ;
#28936 = CARTESIAN_POINT ( 'NONE',  ( -40.50720532202722524, 7.584939507552747706, 60.08350751967648762 ) ) ;
#28937 = DIRECTION ( 'NONE',  ( -1.000000000000000000, 0.000000000000000000, 0.000000000000000000 ) ) ;
#28938 = LINE ( 'NONE', #16291, #30425 ) ;
#28939 = VECTOR ( 'NONE', #11862, 1000.000000000000114 ) ;
#28940 = CARTESIAN_POINT ( 'NONE',  ( 45.36511207810797686, 27.90948166895303117, 45.12672418911604666 ) ) ;
#28941 = ORIENTED_EDGE ( 'NONE', *, *, #3195, .T. ) ;
#28942 = CARTESIAN_POINT ( 'NONE',  ( 21.09992658989238734, 32.09164230456639899, 47.04930799450051637 ) ) ;
#28943 = CARTESIAN_POINT ( 'NONE',  ( 48.94625023931840246, 25.97124452788249371, 46.10640627770148825 ) ) ;
#28944 = DIRECTION ( 'NONE',  ( -0.6184495258776567805, 0.3428121700606641120, -0.7071067811865474617 ) ) ;
#28945 = EDGE_CURVE ( 'NONE', #8738, #3050, #9691, .T. ) ;
#28946 = CIRCLE ( 'NONE', #26315, 1.899999999999999023 ) ;
#28947 = CARTESIAN_POINT ( 'NONE',  ( -40.10975985016548151, 6.833710191006537649, 34.61556979244075194 ) ) ;
#28948 = ADVANCED_FACE ( 'NONE', ( #9034 ), #8932, .T. ) ;
#28949 = LINE ( 'NONE', #16134, #4780 ) ;
#28950 = ORIENTED_EDGE ( 'NONE', *, *, #3259, .F. ) ;
#28951 = AXIS2_PLACEMENT_3D ( 'NONE', #17359, #27381, #20145 ) ;
#28952 = CYLINDRICAL_SURFACE ( 'NONE', #21319, 0.1000000000000008243 ) ;
#28953 = DIRECTION ( 'NONE',  ( 0.2756373558169947779, -0.9612616959383201154, 0.000000000000000000 ) ) ;
#28954 = FACE_OUTER_BOUND ( 'NONE', #6556, .T. ) ;
#28955 = ORIENTED_EDGE ( 'NONE', *, *, #1578, .T. ) ;
#28956 = CARTESIAN_POINT ( 'NONE',  ( 33.71785032049129427, 32.46664230456639899, 47.04930799450051637 ) ) ;
#28957 = DIRECTION ( 'NONE',  ( -1.000000000000000000, 0.000000000000000000, 0.000000000000000000 ) ) ;
#28958 = CARTESIAN_POINT ( 'NONE',  ( 21.09785597605719687, 45.06299627138002251, 69.55109051435312040 ) ) ;
#28959 = CARTESIAN_POINT ( 'NONE',  ( 21.09992658989239089, 28.22145308207318237, 47.04930799450051637 ) ) ;
#28960 = ORIENTED_EDGE ( 'NONE', *, *, #29948, .T. ) ;
#28961 = SPHERICAL_SURFACE ( 'NONE', #3602, 36.01080762834750715 ) ;
#28962 = EDGE_LOOP ( 'NONE', ( #16088, #17528, #15537, #725 ) ) ;
#28963 = ORIENTED_EDGE ( 'NONE', *, *, #31392, .F. ) ;
#28964 = CIRCLE ( 'NONE', #29484, 2.000000000000001776 ) ;
#28965 = VECTOR ( 'NONE', #11263, 1000.000000000000000 ) ;
#28966 = AXIS2_PLACEMENT_3D ( 'NONE', #30293, #15192, #5353 ) ;
#28967 = DIRECTION ( 'NONE',  ( -1.101824276508909887E-16, 1.000000000000000000, -0.000000000000000000 ) ) ;
#28968 = CARTESIAN_POINT ( 'NONE',  ( 21.09992658989238734, 38.56284415653841791, 47.04930799450051637 ) ) ;
#28969 = ORIENTED_EDGE ( 'NONE', *, *, #10287, .T. ) ;
#28970 = CARTESIAN_POINT ( 'NONE',  ( 52.02704899015044759, -5.937394935145313468, -13.39445452378610568 ) ) ;
#28971 = ORIENTED_EDGE ( 'NONE', *, *, #28795, .F. ) ;
#28972 = FACE_OUTER_BOUND ( 'NONE', #24349, .T. ) ;
#28973 = DIRECTION ( 'NONE',  ( 0.2756373558169942228, -0.9612616959383203374, 0.000000000000000000 ) ) ;
#28974 = VERTEX_POINT ( 'NONE', #21977 ) ;
#28975 = CARTESIAN_POINT ( 'NONE',  ( 21.09992658989238734, 32.59164230456639899, 47.04930799450051637 ) ) ;
#28976 = CARTESIAN_POINT ( 'NONE',  ( 33.72499318558949000, 38.56284415653841791, 47.04930799450051637 ) ) ;
#28977 = FACE_OUTER_BOUND ( 'NONE', #20953, .T. ) ;
#28978 = VERTEX_POINT ( 'NONE', #26757 ) ;
#28979 = CARTESIAN_POINT ( 'NONE',  ( 21.09785597605719332, 25.56454579224779877, 23.54930799450051637 ) ) ;
#28980 = EDGE_CURVE ( 'NONE', #16546, #5971, #13964, .T. ) ;
#28981 = DIRECTION ( 'NONE',  ( -0.000000000000000000, 1.000000000000000000, -0.000000000000000000 ) ) ;
#28982 = CARTESIAN_POINT ( 'NONE',  ( 21.09992658989239089, 27.47145308207318593, 47.04930799450051637 ) ) ;
#28983 = CARTESIAN_POINT ( 'NONE',  ( 21.09992658989239089, 28.34184655352419213, 47.04930799450051637 ) ) ;
#28984 = ADVANCED_FACE ( 'NONE', ( #7061 ), #11831, .T. ) ;
#28985 = EDGE_CURVE ( 'NONE', #21737, #6336, #19423, .T. ) ;
#28986 = VECTOR ( 'NONE', #12611, 1000.000000000000000 ) ;
#28987 = FACE_OUTER_BOUND ( 'NONE', #13340, .T. ) ;
#28988 = EDGE_CURVE ( 'NONE', #18054, #10039, #12630, .T. ) ;
#28989 = VERTEX_POINT ( 'NONE', #20503 ) ;
#28990 = DIRECTION ( 'NONE',  ( 0.000000000000000000, 0.000000000000000000, 1.000000000000000000 ) ) ;
#28991 = CARTESIAN_POINT ( 'NONE',  ( -40.02540636251514172, 2.839176264122877047, 57.04930799450051637 ) ) ;
#28992 = VECTOR ( 'NONE', #12268, 1000.000000000000000 ) ;
#28993 = EDGE_LOOP ( 'NONE', ( #582, #1004, #28477, #27511 ) ) ;
#28994 = DIRECTION ( 'NONE',  ( -0.8746197071393927436, 0.4848096202463423876, 1.277302113040827440E-17 ) ) ;
#28995 = CARTESIAN_POINT ( 'NONE',  ( 21.09992658989239089, 28.59143805560861296, 47.04930799450051637 ) ) ;
#28996 = VERTEX_POINT ( 'NONE', #22316 ) ;
#28997 = AXIS2_PLACEMENT_3D ( 'NONE', #12043, #9089, #18923 ) ;
#28998 = VECTOR ( 'NONE', #18355, 1000.000000000000000 ) ;
#28999 = ORIENTED_EDGE ( 'NONE', *, *, #23881, .F. ) ;
#29000 = ORIENTED_EDGE ( 'NONE', *, *, #23307, .F. ) ;
#29001 = AXIS2_PLACEMENT_3D ( 'NONE', #28983, #14052, #6659 ) ;
#29002 = AXIS2_PLACEMENT_3D ( 'NONE', #13003, #4961, #7916 ) ;
#29003 = DIRECTION ( 'NONE',  ( 1.431146867680865853E-17, 2.558717127065790464E-17, 1.000000000000000000 ) ) ;
#29004 = EDGE_CURVE ( 'NONE', #31841, #16102, #2785, .T. ) ;
#29005 = ORIENTED_EDGE ( 'NONE', *, *, #1216, .F. ) ;
#29006 = DIRECTION ( 'NONE',  ( -1.000000000000000000, -1.101824276508909764E-16, 0.000000000000000000 ) ) ;
#29007 = CIRCLE ( 'NONE', #7005, 0.1249999999999983763 ) ;
#29008 = AXIS2_PLACEMENT_3D ( 'NONE', #21837, #6267, #16272 ) ;
#29009 = CIRCLE ( 'NONE', #10161, 2.000000000000001776 ) ;
#29010 = CARTESIAN_POINT ( 'NONE',  ( 21.09785597605718266, 77.37245976740706510, 131.0041182124821830 ) ) ;
#29011 = CARTESIAN_POINT ( 'NONE',  ( 45.28286642839709231, 29.18619643316631240, 47.97516931882780966 ) ) ;
#29012 = ORIENTED_EDGE ( 'NONE', *, *, #11933, .F. ) ;
#29013 = VERTEX_POINT ( 'NONE', #318 ) ;
#29014 = LINE ( 'NONE', #11618, #13768 ) ;
#29015 = ORIENTED_EDGE ( 'NONE', *, *, #2118, .T. ) ;
#29016 = CARTESIAN_POINT ( 'NONE',  ( -42.03703168893574116, 3.954238390689462257, 48.94930799450051495 ) ) ;
#29017 = DIRECTION ( 'NONE',  ( -1.101824276508909887E-16, 1.000000000000000000, -0.000000000000000000 ) ) ;
#29018 = DIRECTION ( 'NONE',  ( -1.101824276508909887E-16, 1.000000000000000000, -0.000000000000000000 ) ) ;
#29019 = DIRECTION ( 'NONE',  ( -0.000000000000000000, -0.000000000000000000, -1.000000000000000000 ) ) ;
#29020 = EDGE_CURVE ( 'NONE', #8513, #14507, #13147, .T. ) ;
#29021 = EDGE_CURVE ( 'NONE', #1158, #9965, #31475, .T. ) ;
#29022 = CARTESIAN_POINT ( 'NONE',  ( 44.77625694075214824, 28.11454579807170617, 48.23360063142255427 ) ) ;
#29023 = EDGE_CURVE ( 'NONE', #19411, #13392, #11231, .T. ) ;
#29024 = CARTESIAN_POINT ( 'NONE',  ( 21.09785597605719332, 77.37245976740706510, 47.04930799450051637 ) ) ;
#29025 = DIRECTION ( 'NONE',  ( 0.1949050434465282311, -0.6797146636928673713, -0.7071067811865470176 ) ) ;
#29026 = EDGE_CURVE ( 'NONE', #2319, #23152, #8046, .T. ) ;
#29027 = ORIENTED_EDGE ( 'NONE', *, *, #3292, .F. ) ;
#29028 = LINE ( 'NONE', #18675, #23409 ) ;
#29029 = CARTESIAN_POINT ( 'NONE',  ( -40.18454328187963398, 7.548069831825863218, 53.54930799450051637 ) ) ;
#29030 = DIRECTION ( 'NONE',  ( -0.000000000000000000, 1.000000000000000000, -0.000000000000000000 ) ) ;
#29031 = CARTESIAN_POINT ( 'NONE',  ( 21.09785597605720042, 12.39166260509097484, 101.6006104443987397 ) ) ;
#29032 = FACE_OUTER_BOUND ( 'NONE', #30485, .T. ) ;
#29033 = CIRCLE ( 'NONE', #28216, 12.36707279061065101 ) ;
#29034 = ORIENTED_EDGE ( 'NONE', *, *, #11238, .F. ) ;
#29035 = DIRECTION ( 'NONE',  ( 0.000000000000000000, 0.000000000000000000, 1.000000000000000000 ) ) ;
#29036 = ORIENTED_EDGE ( 'NONE', *, *, #24308, .F. ) ;
#29037 = CARTESIAN_POINT ( 'NONE',  ( 21.09785597605719687, 25.56454579224779877, 27.04930799450051637 ) ) ;
#29038 = DIRECTION ( 'NONE',  ( 0.000000000000000000, 1.000000000000000000, 0.000000000000000000 ) ) ;
#29039 = CIRCLE ( 'NONE', #20123, 0.1250000000000001110 ) ;
#29040 = ORIENTED_EDGE ( 'NONE', *, *, #21571, .T. ) ;
#29041 = VERTEX_POINT ( 'NONE', #22641 ) ;
#29042 = DIRECTION ( 'NONE',  ( -1.224646799147353207E-16, 0.000000000000000000, -1.000000000000000000 ) ) ;
#29043 = EDGE_CURVE ( 'NONE', #593, #4576, #16798, .T. ) ;
#29044 = CARTESIAN_POINT ( 'NONE',  ( 33.46699938050303302, 38.56284415653841791, 47.04930799450051637 ) ) ;
#29045 = LINE ( 'NONE', #6719, #19391 ) ;
#29046 = EDGE_CURVE ( 'NONE', #2645, #23989, #20016, .T. ) ;
#29047 = ORIENTED_EDGE ( 'NONE', *, *, #3931, .F. ) ;
#29048 = DIRECTION ( 'NONE',  ( 0.8746197071393925215, -0.4848096202463429982, -8.676864087101708112E-18 ) ) ;
#29049 = DIRECTION ( 'NONE',  ( -1.000000000000000000, 0.000000000000000000, 0.000000000000000000 ) ) ;
#29050 = CARTESIAN_POINT ( 'NONE',  ( 77.89472409461923519, -4.535950511381784622, 13.85981127911711575 ) ) ;
#29051 = AXIS2_PLACEMENT_3D ( 'NONE', #27182, #9961, #14889 ) ;
#29052 = VERTEX_POINT ( 'NONE', #24951 ) ;
#29053 = LINE ( 'NONE', #14121, #14800 ) ;
#29054 = ORIENTED_EDGE ( 'NONE', *, *, #29059, .T. ) ;
#29055 = AXIS2_PLACEMENT_3D ( 'NONE', #8221, #8700, #13474 ) ;
#29056 = FACE_BOUND ( 'NONE', #13905, .T. ) ;
#29057 = DIRECTION ( 'NONE',  ( 1.000000000000000000, 0.000000000000000000, 0.000000000000000000 ) ) ;
#29058 = CARTESIAN_POINT ( 'NONE',  ( -45.63949534714383560, -5.900352476715130301, 40.43365730525594870 ) ) ;
#29059 = EDGE_CURVE ( 'NONE', #5208, #22400, #22956, .T. ) ;
#29060 = ORIENTED_EDGE ( 'NONE', *, *, #17792, .T. ) ;
#29061 = ORIENTED_EDGE ( 'NONE', *, *, #4217, .F. ) ;
#29062 = CARTESIAN_POINT ( 'NONE',  ( 21.09785597605720753, 17.16474120167318063, 47.04930799450052348 ) ) ;
#29063 = DIRECTION ( 'NONE',  ( 0.4848096202463429427, 0.8746197071393925215, -2.352477780477436787E-16 ) ) ;
#29064 = EDGE_LOOP ( 'NONE', ( #26754, #4333, #20866, #5263 ) ) ;
#29065 = CYLINDRICAL_SURFACE ( 'NONE', #13507, 32.50000000000000711 ) ;
#29066 = CARTESIAN_POINT ( 'NONE',  ( 78.94643999631821885, -13.74047052604243113, 39.42791148283190239 ) ) ;
#29067 = ORIENTED_EDGE ( 'NONE', *, *, #12911, .T. ) ;
#29068 = CARTESIAN_POINT ( 'NONE',  ( -40.59758774925371938, 7.567737757495683226, 39.54930799450052348 ) ) ;
#29069 = CARTESIAN_POINT ( 'NONE',  ( 44.91142894931555674, 29.39787913140503761, 45.63089057098605394 ) ) ;
#29070 = DIRECTION ( 'NONE',  ( -1.000000000000000000, 0.000000000000000000, 0.000000000000000000 ) ) ;
#29071 = AXIS2_PLACEMENT_3D ( 'NONE', #31039, #15290, #13479 ) ;
#29072 = ADVANCED_FACE ( 'NONE', ( #28063 ), #25207, .F. ) ;
#29073 = CIRCLE ( 'NONE', #781, 0.1250000000000001110 ) ;
#29074 = CIRCLE ( 'NONE', #13875, 12.62506659569710266 ) ;
#29075 = VECTOR ( 'NONE', #19967, 1000.000000000000114 ) ;
#29076 = EDGE_CURVE ( 'NONE', #16751, #29171, #32398, .T. ) ;
#29077 = AXIS2_PLACEMENT_3D ( 'NONE', #14439, #24433, #31825 ) ;
#29078 = ORIENTED_EDGE ( 'NONE', *, *, #3807, .F. ) ;
#29079 = CARTESIAN_POINT ( 'NONE',  ( 21.09992658989238734, 31.84164230456639544, 47.04930799450051637 ) ) ;
#29080 = FACE_OUTER_BOUND ( 'NONE', #27045, .T. ) ;
#29081 = EDGE_CURVE ( 'NONE', #9952, #9196, #7881, .T. ) ;
#29082 = CARTESIAN_POINT ( 'NONE',  ( -39.58809650894544774, 2.596771453999702661, 47.04930799450051637 ) ) ;
#29083 = CARTESIAN_POINT ( 'NONE',  ( 45.79384627280941089, 29.26618040159425860, 49.05938063676249072 ) ) ;
#29084 = EDGE_CURVE ( 'NONE', #4784, #29883, #5293, .T. ) ;
#29085 = ORIENTED_EDGE ( 'NONE', *, *, #10627, .T. ) ;
#29086 = EDGE_CURVE ( 'NONE', #2250, #4802, #478, .T. ) ;
#29087 = DIRECTION ( 'NONE',  ( 0.000000000000000000, 0.000000000000000000, -1.000000000000000000 ) ) ;
#29088 = DIRECTION ( 'NONE',  ( -1.101824276508909887E-16, 1.000000000000000000, -0.000000000000000000 ) ) ;
#29089 = CARTESIAN_POINT ( 'NONE',  ( 21.09992658989239089, 27.84164230456639544, 47.04930799450051637 ) ) ;
#29090 = CARTESIAN_POINT ( 'NONE',  ( 21.09785597605719332, 12.06852548259731961, 47.04930799450051637 ) ) ;
#29091 = LINE ( 'NONE', #16767, #28939 ) ;
#29092 = CARTESIAN_POINT ( 'NONE',  ( -34.15232302351033411, -13.74047052604243646, 28.28865559504964011 ) ) ;
#29093 = DIRECTION ( 'NONE',  ( 0.000000000000000000, 0.000000000000000000, -1.000000000000000000 ) ) ;
#29094 = TOROIDAL_SURFACE ( 'NONE', #21755, 12.40141737965284641, 0.1249999999999995698 ) ;
#29095 = CARTESIAN_POINT ( 'NONE',  ( 45.36511207810797686, 25.23213139976340713, 45.12672418911604666 ) ) ;
#29096 = CIRCLE ( 'NONE', #23867, 0.09999999999999766020 ) ;
#29097 = ADVANCED_FACE ( 'NONE', ( #17392 ), #23629, .F. ) ;
#29098 = SURFACE_STYLE_USAGE ( .BOTH. , #7266 ) ;
#29099 = ORIENTED_EDGE ( 'NONE', *, *, #21763, .F. ) ;
#29100 = DIRECTION ( 'NONE',  ( 0.000000000000000000, 0.000000000000000000, -1.000000000000000000 ) ) ;
#29101 = CARTESIAN_POINT ( 'NONE',  ( 48.40186567930497574, 27.42957786121582231, 45.03923535223907493 ) ) ;
#29102 = VECTOR ( 'NONE', #8311, 1000.000000000000000 ) ;
#29103 = AXIS2_PLACEMENT_3D ( 'NONE', #25869, #3379, #28502 ) ;
#29104 = CARTESIAN_POINT ( 'NONE',  ( 21.09785597605719332, -5.721341737285094098, 47.04930799450051637 ) ) ;
#29105 = CARTESIAN_POINT ( 'NONE',  ( 33.50134396954520355, 30.59164230456639544, 47.04930799450051637 ) ) ;
#29106 = CIRCLE ( 'NONE', #17576, 47.39944366991822733 ) ;
#29107 = DIRECTION ( 'NONE',  ( -1.101824276508909887E-16, 1.000000000000000000, -0.000000000000000000 ) ) ;
#29108 = ORIENTED_EDGE ( 'NONE', *, *, #2811, .T. ) ;
#29109 = CARTESIAN_POINT ( 'NONE',  ( -39.54762467759688604, -5.935999211605547998, 77.95416007536729808 ) ) ;
#29110 = DIRECTION ( 'NONE',  ( -0.4848096202463421656, -0.8746197071393929656, -9.920727850371707821E-18 ) ) ;
#29111 = CARTESIAN_POINT ( 'NONE',  ( 21.09785597605719332, 42.30003263981368633, 47.04930799450051637 ) ) ;
#29112 = ORIENTED_EDGE ( 'NONE', *, *, #14535, .F. ) ;
#29113 = DIRECTION ( 'NONE',  ( -1.224646799147353207E-16, -1.349345573449484691E-32, 1.000000000000000000 ) ) ;
#29114 = CARTESIAN_POINT ( 'NONE',  ( 21.09992658989239089, 30.09164230456639544, 47.04930799450051637 ) ) ;
#29115 = LINE ( 'NONE', #16948, #20406 ) ;
#29116 = CARTESIAN_POINT ( 'NONE',  ( 46.33059210211230550, 22.93807716476589675, 45.54522087609679204 ) ) ;
#29117 = ORIENTED_EDGE ( 'NONE', *, *, #5574, .F. ) ;
#29118 = DIRECTION ( 'NONE',  ( -0.000000000000000000, -1.000000000000000000, 0.000000000000000000 ) ) ;
#29119 = ORIENTED_EDGE ( 'NONE', *, *, #18608, .T. ) ;
#29120 = EDGE_CURVE ( 'NONE', #13785, #20229, #20178, .T. ) ;
#29121 = ADVANCED_FACE ( 'NONE', ( #27734 ), #26218, .T. ) ;
#29122 = ORIENTED_EDGE ( 'NONE', *, *, #2834, .F. ) ;
#29123 = AXIS2_PLACEMENT_3D ( 'NONE', #9475, #7168, #12430 ) ;
#29124 = CARTESIAN_POINT ( 'NONE',  ( 21.09785597605719332, 7.264443105416139801, 27.83479196906534625 ) ) ;
#29125 = MECHANICAL_DESIGN_GEOMETRIC_PRESENTATION_REPRESENTATION (  '', ( #12885 ), #20732 ) ;
#29126 = EDGE_CURVE ( 'NONE', #8390, #13490, #26063, .T. ) ;
#29127 = AXIS2_PLACEMENT_3D ( 'NONE', #19553, #7091, #27110 ) ;
#29128 = EDGE_CURVE ( 'NONE', #19572, #19635, #20483, .T. ) ;
#29129 = DIRECTION ( 'NONE',  ( 0.000000000000000000, 0.000000000000000000, -1.000000000000000000 ) ) ;
#29130 = CARTESIAN_POINT ( 'NONE',  ( -29.57396024870593365, 10.91176617787883174, 71.86136379807102514 ) ) ;
#29131 = DIRECTION ( 'NONE',  ( 1.000000000000000000, 0.000000000000000000, 0.000000000000000000 ) ) ;
#29132 = AXIS2_PLACEMENT_3D ( 'NONE', #18059, #25456, #2958 ) ;
#29133 = ORIENTED_EDGE ( 'NONE', *, *, #14063, .F. ) ;
#29134 = CARTESIAN_POINT ( 'NONE',  ( 51.97542764375435809, -5.937448199248382075, -13.39445452378610568 ) ) ;
#29135 = ORIENTED_EDGE ( 'NONE', *, *, #30737, .T. ) ;
#29136 = DIRECTION ( 'NONE',  ( -1.000000000000000000, 0.000000000000000000, 0.000000000000000000 ) ) ;
#29137 = CARTESIAN_POINT ( 'NONE',  ( -43.43257085947613660, 1.024086014757300767, 60.54930799450051637 ) ) ;
#29138 = VERTEX_POINT ( 'NONE', #11305 ) ;
#29139 = DIRECTION ( 'NONE',  ( 0.8746197071393925215, -0.4848096202463429982, -8.676864087101709653E-18 ) ) ;
#29140 = DIRECTION ( 'NONE',  ( -1.101824276508909887E-16, 1.000000000000000000, -0.000000000000000000 ) ) ;
#29141 = CARTESIAN_POINT ( 'NONE',  ( -40.16174044770769314, 7.468546898574135895, 53.64930799450051779 ) ) ;
#29142 = ORIENTED_EDGE ( 'NONE', *, *, #14168, .T. ) ;
#29143 = CARTESIAN_POINT ( 'NONE',  ( 21.09785597605720042, -16.03545420775219910, 47.04930799450051637 ) ) ;
#29144 = FACE_OUTER_BOUND ( 'NONE', #23238, .T. ) ;
#29145 = CARTESIAN_POINT ( 'NONE',  ( 21.09992658989238734, 32.34164230456639899, 47.04930799450051637 ) ) ;
#29146 = DIRECTION ( 'NONE',  ( -1.224646799147353207E-16, -1.349345573449484691E-32, 1.000000000000000000 ) ) ;
#29147 = CARTESIAN_POINT ( 'NONE',  ( 8.698509210239508960, 24.34164230456639544, 47.04930799450051637 ) ) ;
#29148 = ORIENTED_EDGE ( 'NONE', *, *, #6998, .F. ) ;
#29149 = CARTESIAN_POINT ( 'NONE',  ( 21.09785597605719332, 15.43591091851533115, 34.06511779397349926 ) ) ;
#29150 = FACE_OUTER_BOUND ( 'NONE', #17006, .T. ) ;
#29151 = EDGE_LOOP ( 'NONE', ( #31696, #5752, #5881 ) ) ;
#29152 = AXIS2_PLACEMENT_3D ( 'NONE', #19853, #7717, #4770 ) ;
#29153 =( GEOMETRIC_REPRESENTATION_CONTEXT ( 3 ) GLOBAL_UNCERTAINTY_ASSIGNED_CONTEXT ( ( #28524 ) ) GLOBAL_UNIT_ASSIGNED_CONTEXT ( ( #1810, #20180, #24953 ) ) REPRESENTATION_CONTEXT ( 'NONE', 'WORKASPACE' ) );
#29154 = DIRECTION ( 'NONE',  ( -1.000000000000000000, 0.000000000000000000, 0.000000000000000000 ) ) ;
#29155 = ORIENTED_EDGE ( 'NONE', *, *, #594, .T. ) ;
#29156 = VERTEX_POINT ( 'NONE', #6377 ) ;
#29157 = B_SPLINE_CURVE_WITH_KNOTS ( 'NONE', 3,
 ( #27543, #24921, #12618, #2434 ),
 .UNSPECIFIED., .F., .F.,
 ( 4, 4 ),
 ( 0.07560733880179559829, 0.09146776418496910255 ),
 .UNSPECIFIED. ) ;
#29158 = TOROIDAL_SURFACE ( 'NONE', #15014, 1.142135311067127068, 0.1000000000000000056 ) ;
#29159 = EDGE_LOOP ( 'NONE', ( #3095, #11390, #24453, #5234 ) ) ;
#29160 = EDGE_CURVE ( 'NONE', #1265, #8738, #2148, .T. ) ;
#29161 = EDGE_CURVE ( 'NONE', #30996, #19482, #13706, .T. ) ;
#29162 = PLANE ( 'NONE',  #21889 ) ;
#29163 = CIRCLE ( 'NONE', #3481, 12.27641737965281621 ) ;
#29164 = PRODUCT_DEFINITION_FORMATION_WITH_SPECIFIED_SOURCE ( 'ANY', '', #29749, .NOT_KNOWN. ) ;
#29165 = ORIENTED_EDGE ( 'NONE', *, *, #1779, .T. ) ;
#29166 = CARTESIAN_POINT ( 'NONE',  ( 21.09785597605718976, 7.881678200673687407, 66.30757762003366906 ) ) ;
#29167 = CARTESIAN_POINT ( 'NONE',  ( 21.09992658989239089, 28.09184655352419213, 47.04930799450051637 ) ) ;
#29168 = DIRECTION ( 'NONE',  ( 0.000000000000000000, 0.000000000000000000, -1.000000000000000000 ) ) ;
#29169 = CARTESIAN_POINT ( 'NONE',  ( 8.698509210239587119, 32.34164230456639899, 47.04930799450051637 ) ) ;
#29170 = CARTESIAN_POINT ( 'NONE',  ( 49.44739180854976013, 28.77786309983298096, 47.17133137409169308 ) ) ;
#29171 = VERTEX_POINT ( 'NONE', #21295 ) ;
#29172 = DIRECTION ( 'NONE',  ( -1.224646799147353207E-16, -1.349345573449484691E-32, 1.000000000000000000 ) ) ;
#29173 = EDGE_LOOP ( 'NONE', ( #25940, #15325, #26375, #22926, #16695, #11117 ) ) ;
#29174 = PLANE ( 'NONE',  #20062 ) ;
#29175 = ORIENTED_EDGE ( 'NONE', *, *, #23285, .F. ) ;
#29176 = FACE_OUTER_BOUND ( 'NONE', #32145, .T. ) ;
#29177 = DIRECTION ( 'NONE',  ( -1.188208965918164993E-16, -1.880121038077812639E-16, -1.000000000000000000 ) ) ;
#29178 = CIRCLE ( 'NONE', #7157, 55.72436264418301732 ) ;
#29179 = CARTESIAN_POINT ( 'NONE',  ( -40.50410981870283678, 7.604537000166497585, 38.76008276981544753 ) ) ;
#29180 = CARTESIAN_POINT ( 'NONE',  ( 48.59785597605719687, 13.86454579224779948, 47.04930799450052348 ) ) ;
#29181 = CARTESIAN_POINT ( 'NONE',  ( 33.71785032049135822, 26.71664230456639899, 47.04930799450051637 ) ) ;
#29182 = CARTESIAN_POINT ( 'NONE',  ( 45.73035263060504718, 25.13954579807171186, 44.36855633853329550 ) ) ;
#29183 = CARTESIAN_POINT ( 'NONE',  ( 46.72376704384358703, 22.91413368675619111, 48.81312807415246624 ) ) ;
#29184 = DIRECTION ( 'NONE',  ( -1.000000000000000000, 0.000000000000000000, 0.000000000000000000 ) ) ;
#29185 = VERTEX_POINT ( 'NONE', #8203 ) ;
#29186 = CYLINDRICAL_SURFACE ( 'NONE', #19715, 2.000000000000001776 ) ;
#29187 = DIRECTION ( 'NONE',  ( 0.8746197071393926326, -0.4848096202463430537, -8.676864087101709653E-18 ) ) ;
#29188 = DIRECTION ( 'NONE',  ( 0.4544104193609903586, 0.000000000000000000, 0.8907924397839087627 ) ) ;
#29189 = CARTESIAN_POINT ( 'NONE',  ( 48.01680169312756874, 22.93807716476589675, 45.63279442905646022 ) ) ;
#29190 = DIRECTION ( 'NONE',  ( 0.2756373558169954441, -0.9612616959383198934, 1.479773560108263204E-16 ) ) ;
#29191 = VERTEX_POINT ( 'NONE', #8520 ) ;
#29192 = DIRECTION ( 'NONE',  ( 0.000000000000000000, 0.000000000000000000, -1.000000000000000000 ) ) ;
#29193 = VERTEX_POINT ( 'NONE', #18190 ) ;
#29194 = CARTESIAN_POINT ( 'NONE',  ( 21.09992658989238734, 38.56284415653841791, 47.04930799450051637 ) ) ;
#29195 = CARTESIAN_POINT ( 'NONE',  ( -40.70335362822509495, 9.387769322903325886, 39.54930799450052348 ) ) ;
#29196 = TOROIDAL_SURFACE ( 'NONE', #1943, 0.9000000000000003553, 0.1000000000000000056 ) ;
#29197 = ORIENTED_EDGE ( 'NONE', *, *, #27010, .T. ) ;
#29198 = CIRCLE ( 'NONE', #15061, 30.00000000000000711 ) ;
#29199 = EDGE_CURVE ( 'NONE', #24404, #4539, #27847, .T. ) ;
#29200 = ADVANCED_FACE ( 'NONE', ( #20823 ), #15779, .F. ) ;
#29201 =( BOUNDED_CURVE ( )  B_SPLINE_CURVE ( 2, ( #2887, #17820, #23551, #1069, #5849, #25854, #3367, #18297, #21082 ),
 .UNSPECIFIED., .F., .F. ) 
 B_SPLINE_CURVE_WITH_KNOTS ( ( 3, 2, 2, 2, 3 ),
 ( 0.3214285702672988188, 0.3333333333333333703, 0.3571428571428570953, 0.3809523809523809312, 0.3928571416958702711 ),
 .UNSPECIFIED. ) 
 CURVE ( )  GEOMETRIC_REPRESENTATION_ITEM ( )  RATIONAL_B_SPLINE_CURVE ( ( 0.9330127018922199644, 0.9330126953578159466, 1.000000000000000000, 0.8660254037844387076, 1.000000000000000000, 0.8660254037844387076, 1.000000000000000000, 0.9330127084266224280, 0.9330127018922200755 ) ) 
 REPRESENTATION_ITEM ( '' )  );
#29202 = ORIENTED_EDGE ( 'NONE', *, *, #15069, .T. ) ;
#29203 = EDGE_CURVE ( 'NONE', #2086, #8185, #23293, .T. ) ;
#29204 = EDGE_CURVE ( 'NONE', #26418, #27205, #28223, .T. ) ;
#29205 = CARTESIAN_POINT ( 'NONE',  ( -42.38687957179149635, 4.148162238787999279, 38.34930799450052064 ) ) ;
#29206 = CARTESIAN_POINT ( 'NONE',  ( -40.23967075304302909, 7.740322171013526820, 53.80788663826320573 ) ) ;
#29207 = CARTESIAN_POINT ( 'NONE',  ( 8.732853799281738105, 25.96183152705960140, 47.04930799450051637 ) ) ;
#29208 = ORIENTED_EDGE ( 'NONE', *, *, #17195, .F. ) ;
#29209 = CARTESIAN_POINT ( 'NONE',  ( 45.75738744548056758, 22.91413368675619111, 45.84342743610336868 ) ) ;
#29210 = AXIS2_PLACEMENT_3D ( 'NONE', #1752, #21438, #1910 ) ;
#29211 = CARTESIAN_POINT ( 'NONE',  ( 21.09785597605719332, 77.37245976740706510, 47.04930799450051637 ) ) ;
#29212 = DIRECTION ( 'NONE',  ( -1.000000000000000000, 0.000000000000000000, 0.000000000000000000 ) ) ;
#29213 = AXIS2_PLACEMENT_3D ( 'NONE', #20549, #25481, #30095 ) ;
#29214 = VERTEX_POINT ( 'NONE', #31326 ) ;
#29215 = EDGE_LOOP ( 'NONE', ( #19948, #17150, #24610, #1080 ) ) ;
#29216 = CARTESIAN_POINT ( 'NONE',  ( 21.09992658989238734, 38.56284415653841791, 47.04930799450051637 ) ) ;
#29217 = CARTESIAN_POINT ( 'NONE',  ( 21.09992658989238734, 38.56284415653841791, 47.04930799450051637 ) ) ;
#29218 = TOROIDAL_SURFACE ( 'NONE', #26589, 39.69941114636694834, 0.3000000000000000444 ) ;
#29219 = CARTESIAN_POINT ( 'NONE',  ( -38.36853489569023168, 7.065850718397949315, 32.04930799450052348 ) ) ;
#29220 = VERTEX_POINT ( 'NONE', #807 ) ;
#29221 = ORIENTED_EDGE ( 'NONE', *, *, #24913, .T. ) ;
#29222 = APPLICATION_CONTEXT ( 'automotive_design' ) ;
#29223 = DIRECTION ( 'NONE',  ( -1.101824276508909887E-16, 1.000000000000000000, -0.000000000000000000 ) ) ;
#29224 = DIRECTION ( 'NONE',  ( -0.4441739386572013393, -0.2110602665713099402, -0.8707256032141217350 ) ) ;
#29225 = CARTESIAN_POINT ( 'NONE',  ( -40.06561427811386267, 7.496110634155836117, 59.44930799450051495 ) ) ;
#29226 = ORIENTED_EDGE ( 'NONE', *, *, #7398, .F. ) ;
#29227 = CARTESIAN_POINT ( 'NONE',  ( 45.96182992765472619, 26.47822092656774728, 44.82232689504103007 ) ) ;
#29228 = CARTESIAN_POINT ( 'NONE',  ( 77.45956091363653684, -13.74047052604244001, 31.95286555045028720 ) ) ;
#29229 = VERTEX_POINT ( 'NONE', #10832 ) ;
#29230 = DIRECTION ( 'NONE',  ( 0.000000000000000000, 0.000000000000000000, -1.000000000000000000 ) ) ;
#29231 = CARTESIAN_POINT ( 'NONE',  ( 50.10320668408830613, 26.30621246473837616, 47.20539118556276037 ) ) ;
#29232 = EDGE_CURVE ( 'NONE', #4736, #5228, #16378, .T. ) ;
#29233 = EDGE_CURVE ( 'NONE', #29041, #24330, #17499, .T. ) ;
#29234 = CARTESIAN_POINT ( 'NONE',  ( 21.09785597605720753, -14.04221034894631615, 105.9124997376166277 ) ) ;
#29235 = AXIS2_PLACEMENT_3D ( 'NONE', #19954, #7499, #14553 ) ;
#29236 = EDGE_LOOP ( 'NONE', ( #4286, #17121, #31797, #27719 ) ) ;
#29237 = AXIS2_PLACEMENT_3D ( 'NONE', #31495, #16697, #18998 ) ;
#29238 = DIRECTION ( 'NONE',  ( -1.000000000000000000, 0.000000000000000000, 0.000000000000000000 ) ) ;
#29239 = EDGE_CURVE ( 'NONE', #13343, #8733, #10677, .T. ) ;
#29240 = CARTESIAN_POINT ( 'NONE',  ( 45.35708200440645044, 28.39118040159425860, 45.92000246470679770 ) ) ;
#29241 = CIRCLE ( 'NONE', #31342, 1.500000000000001332 ) ;
#29242 = ORIENTED_EDGE ( 'NONE', *, *, #22196, .F. ) ;
#29243 = DIRECTION ( 'NONE',  ( 0.9612616959383193382, 0.2756373558169973870, 8.795445018804928853E-19 ) ) ;
#29244 = CYLINDRICAL_SURFACE ( 'NONE', #17718, 55.00000000000000000 ) ;
#29245 = CARTESIAN_POINT ( 'NONE',  ( 53.31593463385092235, -5.523138741469208135, -10.01380679907181737 ) ) ;
#29246 = FACE_BOUND ( 'NONE', #21153, .T. ) ;
#29247 = FACE_OUTER_BOUND ( 'NONE', #861, .T. ) ;
#29248 = CARTESIAN_POINT ( 'NONE',  ( 2.337203576606338373, -13.74047052604243646, 102.2994869940680474 ) ) ;
#29249 = CARTESIAN_POINT ( 'NONE',  ( -40.60333149162104860, 7.557375771971046596, 58.05249952744806308 ) ) ;
#29250 = EDGE_CURVE ( 'NONE', #21573, #9948, #18392, .T. ) ;
#29251 = CARTESIAN_POINT ( 'NONE',  ( 45.96182992765471909, 27.87822092656774231, 44.82232689504102296 ) ) ;
#29252 =( NAMED_UNIT ( * ) SI_UNIT ( $, .STERADIAN. ) SOLID_ANGLE_UNIT ( ) );
#29253 = EDGE_LOOP ( 'NONE', ( #23945, #19761, #22806, #32334, #13409 ) ) ;
#29254 = CARTESIAN_POINT ( 'NONE',  ( 21.09785597605719332, 48.06454579224779877, 47.04930799450051637 ) ) ;
#29255 = VECTOR ( 'NONE', #30749, 1000.000000000000114 ) ;
#29256 = AXIS2_PLACEMENT_3D ( 'NONE', #26826, #8940, #29131 ) ;
#29257 = CARTESIAN_POINT ( 'NONE',  ( 44.35155721551191021, 25.17319976284614924, 46.90667869236616383 ) ) ;
#29258 = EDGE_CURVE ( 'NONE', #13589, #24454, #28384, .T. ) ;
#29259 = LINE ( 'NONE', #26634, #13509 ) ;
#29260 = CIRCLE ( 'NONE', #958, 1.799999999999998490 ) ;
#29261 = AXIS2_PLACEMENT_3D ( 'NONE', #22884, #5174, #30609 ) ;
#29262 = FACE_OUTER_BOUND ( 'NONE', #29773, .T. ) ;
#29263 = ORIENTED_EDGE ( 'NONE', *, *, #10129, .F. ) ;
#29264 = CARTESIAN_POINT ( 'NONE',  ( -39.55665669155531106, -5.935685895218067998, 77.88576325833030012 ) ) ;
#29265 = CARTESIAN_POINT ( 'NONE',  ( -63.90214402394282445, 9.925589859889736744, 40.04930799450051637 ) ) ;
#29266 = AXIS2_PLACEMENT_3D ( 'NONE', #21107, #6506, #31142 ) ;
#29267 = ORIENTED_EDGE ( 'NONE', *, *, #16076, .F. ) ;
#29268 = ORIENTED_EDGE ( 'NONE', *, *, #9260, .F. ) ;
#29269 = DIRECTION ( 'NONE',  ( 0.8746197071393926326, -0.4848096202463430537, -8.676864087101709653E-18 ) ) ;
#29270 = DIRECTION ( 'NONE',  ( 0.4544104193609905806, -6.737912671758737363E-17, 0.8907924397839086517 ) ) ;
#29271 = ADVANCED_FACE ( 'NONE', ( #3425 ), #19646, .F. ) ;
#29272 = ADVANCED_FACE ( 'NONE', ( #9161 ), #12121, .T. ) ;
#29273 = CARTESIAN_POINT ( 'NONE',  ( 33.72499318558949710, 25.09143805560860940, 47.04930799450051637 ) ) ;
#29274 = CIRCLE ( 'NONE', #5680, 12.36707279061065101 ) ;
#29275 = CARTESIAN_POINT ( 'NONE',  ( 56.35714053840848692, -3.295808585244882849, 106.7232700815558957 ) ) ;
#29276 = ORIENTED_EDGE ( 'NONE', *, *, #15668, .T. ) ;
#29277 = CARTESIAN_POINT ( 'NONE',  ( -41.10400476907452116, 9.333823787025622210, 39.43215070697513625 ) ) ;
#29278 = ORIENTED_EDGE ( 'NONE', *, *, #18289, .T. ) ;
#29279 = EDGE_LOOP ( 'NONE', ( #13078, #20298, #14734, #17669 ) ) ;
#29280 = EDGE_CURVE ( 'NONE', #607, #12276, #19157, .T. ) ;
#29281 = CARTESIAN_POINT ( 'NONE',  ( 52.07598125554711999, -5.935454207752202116, 107.4212530892143889 ) ) ;
#29282 = AXIS2_PLACEMENT_3D ( 'NONE', #17908, #27, #2808 ) ;
#29283 = AXIS2_PLACEMENT_3D ( 'NONE', #21307, #8212, #3763 ) ;
#29284 = VECTOR ( 'NONE', #30574, 1000.000000000000227 ) ;
#29285 = CARTESIAN_POINT ( 'NONE',  ( -42.24141723705587737, 13.63285518870473290, 59.54930799450050927 ) ) ;
#29286 = DIRECTION ( 'NONE',  ( -1.101824276508909887E-16, 1.000000000000000000, -0.000000000000000000 ) ) ;
#29287 = CARTESIAN_POINT ( 'NONE',  ( -42.66751614955960292, 15.14923148629343963, 35.64930799450052490 ) ) ;
#29288 = ORIENTED_EDGE ( 'NONE', *, *, #12736, .F. ) ;
#29289 = AXIS2_PLACEMENT_3D ( 'NONE', #10383, #25636, #20378 ) ;
#29290 = CARTESIAN_POINT ( 'NONE',  ( 21.09785597605719332, 30.56454579224779522, 47.04930799450051637 ) ) ;
#29291 = EDGE_LOOP ( 'NONE', ( #32267, #18569, #11649, #10479, #21730, #9107 ) ) ;
#29292 = DIRECTION ( 'NONE',  ( -1.000000000000000000, 0.000000000000000000, 0.000000000000000000 ) ) ;
#29293 = EDGE_CURVE ( 'NONE', #22063, #24883, #17334, .T. ) ;
#29294 = CARTESIAN_POINT ( 'NONE',  ( 33.71785032049136532, 25.96664230456639899, 47.04930799450051637 ) ) ;
#29295 = DIRECTION ( 'NONE',  ( -0.000000000000000000, -1.000000000000000000, 0.000000000000000000 ) ) ;
#29296 = EDGE_LOOP ( 'NONE', ( #4776, #31747, #3189, #11828 ) ) ;
#29297 = PLANE ( 'NONE',  #799 ) ;
#29298 = CARTESIAN_POINT ( 'NONE',  ( -43.64073206722599707, 1.267352857069779848, 39.44930799450052916 ) ) ;
#29299 = CARTESIAN_POINT ( 'NONE',  ( 21.09992658989238734, 38.56284415653841791, 47.04930799450051637 ) ) ;
#29300 = DIRECTION ( 'NONE',  ( 0.000000000000000000, 1.000000000000000000, 0.000000000000000000 ) ) ;
#29301 = DIRECTION ( 'NONE',  ( -1.224646799147353207E-16, -1.349345573449484691E-32, 1.000000000000000000 ) ) ;
#29302 = CARTESIAN_POINT ( 'NONE',  ( -40.18117225532238024, 7.056010640735429718, 34.94364560924564245 ) ) ;
#29303 = CARTESIAN_POINT ( 'NONE',  ( 21.09992658989239089, 23.71183152705959429, 47.04930799450051637 ) ) ;
#29304 = VERTEX_POINT ( 'NONE', #21943 ) ;
#29305 = CARTESIAN_POINT ( 'NONE',  ( -40.19935072163751499, 7.013056605096608109, 34.87232122021060832 ) ) ;
#29306 = DIRECTION ( 'NONE',  ( -1.101824276508909887E-16, 1.000000000000000000, -0.000000000000000000 ) ) ;
#29307 = ORIENTED_EDGE ( 'NONE', *, *, #7381, .T. ) ;
#29308 = DIRECTION ( 'NONE',  ( -1.000000000000000000, -1.101824276508909887E-16, 0.000000000000000000 ) ) ;
#29309 = CIRCLE ( 'NONE', #22483, 12.36707279061065279 ) ;
#29310 = ADVANCED_FACE ( 'NONE', ( #9319 ), #6935, .T. ) ;
#29311 = AXIS2_PLACEMENT_3D ( 'NONE', #6880, #22401, #16877 ) ;
#29312 = DIRECTION ( 'NONE',  ( 0.4848096202463430537, 0.8746197071393926326, 1.323854077651070671E-16 ) ) ;
#29313 = ADVANCED_FACE ( 'NONE', ( #3909 ), #13934, .F. ) ;
#29314 = ORIENTED_EDGE ( 'NONE', *, *, #2803, .T. ) ;
#29315 = ORIENTED_EDGE ( 'NONE', *, *, #8023, .T. ) ;
#29316 = AXIS2_PLACEMENT_3D ( 'NONE', #11801, #31980, #19328 ) ;
#29317 = ORIENTED_EDGE ( 'NONE', *, *, #22571, .T. ) ;
#29318 = AXIS2_PLACEMENT_3D ( 'NONE', #1658, #11681, #19369 ) ;
#29319 = FACE_OUTER_BOUND ( 'NONE', #19307, .T. ) ;
#29320 = VECTOR ( 'NONE', #32449, 1000.000000000000114 ) ;
#29321 = AXIS2_PLACEMENT_3D ( 'NONE', #27988, #15349, #23051 ) ;
#29322 = ORIENTED_EDGE ( 'NONE', *, *, #25885, .T. ) ;
#29323 = ORIENTED_EDGE ( 'NONE', *, *, #24799, .F. ) ;
#29324 = CARTESIAN_POINT ( 'NONE',  ( 21.09785597605720753, -5.098646251524523443, 47.04930799450052348 ) ) ;
#29325 = CARTESIAN_POINT ( 'NONE',  ( 47.71045395478045492, 23.04411619146718238, 46.10501571378621577 ) ) ;
#29326 = FACE_BOUND ( 'NONE', #18664, .T. ) ;
#29327 = CARTESIAN_POINT ( 'NONE',  ( -40.50730207061041455, 7.560184202955509747, 53.81891027488745749 ) ) ;
#29328 = ADVANCED_FACE ( 'NONE', ( #8998 ), #14726, .T. ) ;
#29329 = CARTESIAN_POINT ( 'NONE',  ( 48.16694854572211426, 28.66119643316631738, 49.14507740233662503 ) ) ;
#29330 = VERTEX_POINT ( 'NONE', #18994 ) ;
#29331 = FACE_OUTER_BOUND ( 'NONE', #27844, .T. ) ;
#29332 = ORIENTED_EDGE ( 'NONE', *, *, #19097, .F. ) ;
#29333 = CARTESIAN_POINT ( 'NONE',  ( -12.57649835094935931, -1.714651486836148209, -6.690735631693065066 ) ) ;
#29334 = EDGE_LOOP ( 'NONE', ( #4520, #29175, #20475, #31275 ) ) ;
#29335 = CARTESIAN_POINT ( 'NONE',  ( 48.63043294988131748, 29.48064476602542072, 48.61409888045912453 ) ) ;
#29336 = DIRECTION ( 'NONE',  ( 0.000000000000000000, 0.000000000000000000, -1.000000000000000000 ) ) ;
#29337 = CIRCLE ( 'NONE', #31428, 12.27641737965281266 ) ;
#29338 = AXIS2_PLACEMENT_3D ( 'NONE', #16308, #26326, #29607 ) ;
#29339 = DIRECTION ( 'NONE',  ( -1.101824276508909887E-16, 1.000000000000000000, -0.000000000000000000 ) ) ;
#29340 = DIRECTION ( 'NONE',  ( -1.000000000000000000, 0.000000000000000000, 0.000000000000000000 ) ) ;
#29341 = FACE_BOUND ( 'NONE', #18258, .T. ) ;
#29342 = CARTESIAN_POINT ( 'NONE',  ( 49.41945501136223839, 27.76454579807170830, 45.86501535757901848 ) ) ;
#29343 = VECTOR ( 'NONE', #26408, 1000.000000000000114 ) ;
#29344 = CARTESIAN_POINT ( 'NONE',  ( 47.20539956190135200, 23.10527865767145173, 47.62628572795583892 ) ) ;
#29345 = LINE ( 'NONE', #29679, #26905 ) ;
#29346 = ORIENTED_EDGE ( 'NONE', *, *, #26871, .F. ) ;
#29347 = CARTESIAN_POINT ( 'NONE',  ( 8.732853799281734553, 38.56284415653841791, 47.04930799450051637 ) ) ;
#29348 = AXIS2_PLACEMENT_3D ( 'NONE', #569, #17642, #10914 ) ;
#29349 = DIRECTION ( 'NONE',  ( -0.9612616959383205595, -0.2756373558169931681, 1.660411357259282445E-16 ) ) ;
#29350 = CYLINDRICAL_SURFACE ( 'NONE', #6805, 2.499999999999997335 ) ;
#29351 = ADVANCED_FACE ( 'NONE', ( #127 ), #4253, .F. ) ;
#29352 = CARTESIAN_POINT ( 'NONE',  ( 46.04844006429464542, 19.96454579224779380, 44.99211097489548905 ) ) ;
#29353 = EDGE_CURVE ( 'NONE', #20430, #21925, #27695, .T. ) ;
#29354 = CARTESIAN_POINT ( 'NONE',  ( -40.02540636251513462, 2.839176264122874382, 38.34930799450052064 ) ) ;
#29355 = ORIENTED_EDGE ( 'NONE', *, *, #6257, .T. ) ;
#29356 = LINE ( 'NONE', #16545, #3034 ) ;
#29357 = ORIENTED_EDGE ( 'NONE', *, *, #11473, .T. ) ;
#29358 = DIRECTION ( 'NONE',  ( -1.000000000000000000, 0.000000000000000000, 0.000000000000000000 ) ) ;
#29359 = DIRECTION ( 'NONE',  ( 1.188208965918165239E-16, 1.880121038077813132E-16, 1.000000000000000000 ) ) ;
#29360 = AXIS2_PLACEMENT_3D ( 'NONE', #28456, #5642, #5974 ) ;
#29361 = ORIENTED_EDGE ( 'NONE', *, *, #27488, .T. ) ;
#29362 = CIRCLE ( 'NONE', #3680, 2.499999999999998668 ) ;
#29363 = VECTOR ( 'NONE', #18379, 1000.000000000000000 ) ;
#29364 = AXIS2_PLACEMENT_3D ( 'NONE', #13366, #1037, #23996 ) ;
#29365 = EDGE_LOOP ( 'NONE', ( #10378, #16782, #2709, #7923, #12181 ) ) ;
#29366 = AXIS2_PLACEMENT_3D ( 'NONE', #2081, #12765, #271 ) ;
#29367 = DIRECTION ( 'NONE',  ( 0.000000000000000000, 0.000000000000000000, -1.000000000000000000 ) ) ;
#29368 = VECTOR ( 'NONE', #5954, 1000.000000000000000 ) ;
#29369 = DIRECTION ( 'NONE',  ( 0.000000000000000000, -1.000000000000000000, 0.000000000000000000 ) ) ;
#29370 = CARTESIAN_POINT ( 'NONE',  ( 51.92400919103565116, -5.935454207752198563, -11.03616215687537583 ) ) ;
#29371 = CIRCLE ( 'NONE', #16271, 21.49999999999999645 ) ;
#29372 = ORIENTED_EDGE ( 'NONE', *, *, #10970, .T. ) ;
#29373 = FACE_OUTER_BOUND ( 'NONE', #30136, .T. ) ;
#29374 = DIRECTION ( 'NONE',  ( -1.101824276508909887E-16, 1.000000000000000000, -0.000000000000000000 ) ) ;
#29375 = CARTESIAN_POINT ( 'NONE',  ( 8.474859994195286461, 27.59143805560860940, 47.04930799450051637 ) ) ;
#29376 = ORIENTED_EDGE ( 'NONE', *, *, #18488, .T. ) ;
#29377 = ORIENTED_EDGE ( 'NONE', *, *, #1420, .T. ) ;
#29378 = CARTESIAN_POINT ( 'NONE',  ( 33.46699938050304013, 27.97145308207318237, 47.04930799450050927 ) ) ;
#29379 = CIRCLE ( 'NONE', #26752, 0.1250000000000001110 ) ;
#29380 = ORIENTED_EDGE ( 'NONE', *, *, #22300, .F. ) ;
#29381 = FACE_BOUND ( 'NONE', #13473, .T. ) ;
#29382 = DIRECTION ( 'NONE',  ( 0.4544104193609903586, 0.000000000000000000, 0.8907924397839087627 ) ) ;
#29383 = CARTESIAN_POINT ( 'NONE',  ( -45.38828485498197551, -5.820282895468940509, 40.73516372632767002 ) ) ;
#29384 = FILL_AREA_STYLE ('',( #6733 ) ) ;
#29385 = ORIENTED_EDGE ( 'NONE', *, *, #26627, .T. ) ;
#29386 = ORIENTED_EDGE ( 'NONE', *, *, #30629, .F. ) ;
#29387 = DIRECTION ( 'NONE',  ( 0.9612616959383194493, 0.2756373558169974980, 8.795445018804946186E-19 ) ) ;
#29388 = DIRECTION ( 'NONE',  ( 0.9986540920324801229, 6.158269594508761132E-17, 0.05186525298099653458 ) ) ;
#29389 = ADVANCED_FACE ( 'NONE', ( #5216, #25072, #22604, #25395 ), #20296, .T. ) ;
#29390 = AXIS2_PLACEMENT_3D ( 'NONE', #28822, #26517, #4029 ) ;
#29391 = EDGE_CURVE ( 'NONE', #2410, #12082, #29413, .T. ) ;
#29392 = CARTESIAN_POINT ( 'NONE',  ( 21.09992658989238734, 38.56284415653841791, 47.04930799450051637 ) ) ;
#29393 = EDGE_CURVE ( 'NONE', #13364, #10403, #13676, .T. ) ;
#29394 = ADVANCED_FACE ( 'NONE', ( #7522 ), #11590, .T. ) ;
#29395 = ORIENTED_EDGE ( 'NONE', *, *, #4298, .T. ) ;
#29396 = CARTESIAN_POINT ( 'NONE',  ( -11.63095230821880044, 1.147918989839226578, -6.351520201285235423 ) ) ;
#29397 = VECTOR ( 'NONE', #30363, 999.9999999999998863 ) ;
#29398 = DIRECTION ( 'NONE',  ( -1.101824276508909887E-16, 1.000000000000000000, -0.000000000000000000 ) ) ;
#29399 = EDGE_CURVE ( 'NONE', #10259, #25118, #30993, .T. ) ;
#29400 = ORIENTED_EDGE ( 'NONE', *, *, #24678, .F. ) ;
#29401 = CARTESIAN_POINT ( 'NONE',  ( 21.09785597605720042, -16.03545420775219910, 47.04930799450051637 ) ) ;
#29402 = AXIS2_PLACEMENT_3D ( 'NONE', #6163, #24365, #9273 ) ;
#29403 = CARTESIAN_POINT ( 'NONE',  ( 47.23302798462060537, 26.48121246473837687, 44.44659793406428605 ) ) ;
#29404 = B_SPLINE_CURVE_WITH_KNOTS ( 'NONE', 3,
 ( #14251, #24246, #21448, #13166, #1765, #16208, #18986, #8825, #11783, #9313, #13928, #11300, #19311, #18819, #29335, #13767, #15607, #23164 ),
 .UNSPECIFIED., .F., .F.,
 ( 4, 2, 2, 2, 2, 2, 2, 2, 4 ),
 ( 0.000000000000000000, 0.0004968808153924961441, 0.0009937616307849922882, 0.001490642446177488541, 0.001987523261569984576, 0.002484404076962480612, 0.002981284892354977081, 0.003478165707747473117, 0.003975046523139969153 ),
 .UNSPECIFIED. ) ;
#29405 = CARTESIAN_POINT ( 'NONE',  ( -39.52978099598376360, 7.652372239361225681, 61.99930799450051921 ) ) ;
#29406 = AXIS2_PLACEMENT_3D ( 'NONE', #30565, #30726, #20859 ) ;
#29407 = ORIENTED_EDGE ( 'NONE', *, *, #20924, .F. ) ;
#29408 = DIRECTION ( 'NONE',  ( -1.000000000000000000, -1.101824276508909887E-16, 0.000000000000000000 ) ) ;
#29409 = CARTESIAN_POINT ( 'NONE',  ( -43.86882709718853590, -0.1754741395363378920, 32.14930799450051779 ) ) ;
#29410 = CARTESIAN_POINT ( 'NONE',  ( 73.54637414377801008, 11.88152873911358753, 68.55296476473189671 ) ) ;
#29411 = CARTESIAN_POINT ( 'NONE',  ( 45.81741271322955100, 25.74452976649965663, 49.02305402274571122 ) ) ;
#29412 = ORIENTED_EDGE ( 'NONE', *, *, #2449, .T. ) ;
#29413 = CIRCLE ( 'NONE', #577, 1.500000000000001332 ) ;
#29414 = DIRECTION ( 'NONE',  ( -1.000000000000000000, 0.000000000000000000, 0.000000000000000000 ) ) ;
#29415 = DIRECTION ( 'NONE',  ( -1.101824276508909887E-16, 1.000000000000000000, -0.000000000000000000 ) ) ;
#29416 = VECTOR ( 'NONE', #5488, 1000.000000000000000 ) ;
#29417 = EDGE_CURVE ( 'NONE', #3387, #10451, #1454, .T. ) ;
#29418 = CARTESIAN_POINT ( 'NONE',  ( 54.39271611435331977, -0.2653311271195929466, -5.980381597736087684 ) ) ;
#29419 = TOROIDAL_SURFACE ( 'NONE', #26254, 26.49999999999999645, 1.499999999999997780 ) ;
#29420 = CARTESIAN_POINT ( 'NONE',  ( 8.474859994195286461, 29.59184655352418858, 47.04930799450051637 ) ) ;
#29421 = CARTESIAN_POINT ( 'NONE',  ( 49.71782891623905698, 24.91911585698229814, 46.85208669721036046 ) ) ;
#29422 = DIRECTION ( 'NONE',  ( -1.101824276508909887E-16, 1.000000000000000000, -0.000000000000000000 ) ) ;
#29423 = DIRECTION ( 'NONE',  ( -2.779292025043186357E-18, 1.288349127009862211E-17, -1.000000000000000000 ) ) ;
#29424 = DIRECTION ( 'NONE',  ( -0.2756373558170018279, 0.9612616959383181170, 0.000000000000000000 ) ) ;
#29425 = CARTESIAN_POINT ( 'NONE',  ( -10.01358589504979513, -5.935454207834595763, -13.41617548937563598 ) ) ;
#29426 = SHAPE_REPRESENTATION_RELATIONSHIP ( 'NONE' , 'NONE' ,  #17018, #8502 ) ;
#29427 = ORIENTED_EDGE ( 'NONE', *, *, #11344, .F. ) ;
#29428 = CARTESIAN_POINT ( 'NONE',  ( 45.70079091716032593, 22.99884124225578574, 46.82018145558027555 ) ) ;
#29429 = AXIS2_PLACEMENT_3D ( 'NONE', #22836, #15455, #10543 ) ;
#29430 = DIRECTION ( 'NONE',  ( -1.101824276508909887E-16, 1.000000000000000000, -0.000000000000000000 ) ) ;
#29431 = DIRECTION ( 'NONE',  ( -0.000000000000000000, -1.000000000000000000, 0.000000000000000000 ) ) ;
#29432 = EDGE_CURVE ( 'NONE', #12894, #18455, #2687, .T. ) ;
#29433 = CARTESIAN_POINT ( 'NONE',  ( 21.09992658989238734, 38.56284415653841791, 47.04930799450051637 ) ) ;
#29434 = EDGE_CURVE ( 'NONE', #18274, #30996, #18896, .T. ) ;
#29435 = ORIENTED_EDGE ( 'NONE', *, *, #13865, .F. ) ;
#29436 = CARTESIAN_POINT ( 'NONE',  ( -39.57232266946287780, -5.935998081906530111, 77.90559678797934851 ) ) ;
#29437 = CYLINDRICAL_SURFACE ( 'NONE', #25273, 12.62506659569710266 ) ;
#29438 = LINE ( 'NONE', #19410, #21669 ) ;
#29439 = ORIENTED_EDGE ( 'NONE', *, *, #26593, .F. ) ;
#29440 = ORIENTED_EDGE ( 'NONE', *, *, #25932, .T. ) ;
#29441 = LINE ( 'NONE', #5789, #4211 ) ;
#29442 = ADVANCED_FACE ( 'NONE', ( #22429 ), #15272, .T. ) ;
#29443 = CARTESIAN_POINT ( 'NONE',  ( 45.24946171279598417, 29.90784706826092076, 47.99220971130007030 ) ) ;
#29444 = CARTESIAN_POINT ( 'NONE',  ( 64.09785597605721819, 13.86454579224779948, 47.04930799450051637 ) ) ;
#29445 = FACE_OUTER_BOUND ( 'NONE', #29365, .T. ) ;
#29446 = AXIS2_PLACEMENT_3D ( 'NONE', #32096, #5338, #25192 ) ;
#29447 = ORIENTED_EDGE ( 'NONE', *, *, #23578, .T. ) ;
#29448 = CARTESIAN_POINT ( 'NONE',  ( 44.96728230447946117, 29.28052639176819838, 45.96899605402243338 ) ) ;
#29449 = TOROIDAL_SURFACE ( 'NONE', #25763, 12.40141737965280200, 0.1249999999999999445 ) ;
#29450 = ORIENTED_EDGE ( 'NONE', *, *, #19782, .F. ) ;
#29451 =( GEOMETRIC_REPRESENTATION_CONTEXT ( 3 ) GLOBAL_UNCERTAINTY_ASSIGNED_CONTEXT ( ( #16988 ) ) GLOBAL_UNIT_ASSIGNED_CONTEXT ( ( #22510, #31881, #19887 ) ) REPRESENTATION_CONTEXT ( 'NONE', 'WORKASPACE' ) );
#29452 = ORIENTED_EDGE ( 'NONE', *, *, #2553, .T. ) ;
#29453 = DIRECTION ( 'NONE',  ( -0.4848096202463429982, -0.8746197071393925215, -9.920727850371698576E-18 ) ) ;
#29454 = AXIS2_PLACEMENT_3D ( 'NONE', #26673, #6019, #20940 ) ;
#29455 = EDGE_CURVE ( 'NONE', #22939, #3679, #5384, .T. ) ;
#29456 = ORIENTED_EDGE ( 'NONE', *, *, #5, .T. ) ;
#29457 = CARTESIAN_POINT ( 'NONE',  ( -30.89191207862503674, 11.92558985988972609, 67.47405476605740660 ) ) ;
#29458 = CARTESIAN_POINT ( 'NONE',  ( -40.08841711228579641, 7.575633567407562552, 60.29072935073781991 ) ) ;
#29459 = CARTESIAN_POINT ( 'NONE',  ( 21.09785597605719332, -19.93545420775220123, 47.04930799450051637 ) ) ;
#29460 = EDGE_CURVE ( 'NONE', #2537, #12300, #19451, .T. ) ;
#29461 = EDGE_CURVE ( 'NONE', #12291, #3439, #10471, .T. ) ;
#29462 = ORIENTED_EDGE ( 'NONE', *, *, #21807, .F. ) ;
#29463 = FACE_BOUND ( 'NONE', #20238, .T. ) ;
#29464 = ORIENTED_EDGE ( 'NONE', *, *, #12386, .T. ) ;
#29465 = CARTESIAN_POINT ( 'NONE',  ( 21.09992658989238734, 38.56284415653841791, 47.04930799450051637 ) ) ;
#29466 = CIRCLE ( 'NONE', #10082, 1.624998423334081066 ) ;
#29467 = LINE ( 'NONE', #12560, #19995 ) ;
#29468 = DIRECTION ( 'NONE',  ( 0.000000000000000000, 0.000000000000000000, -1.000000000000000000 ) ) ;
#29469 = ORIENTED_EDGE ( 'NONE', *, *, #25671, .T. ) ;
#29470 = CARTESIAN_POINT ( 'NONE',  ( 49.40414881150629611, 19.96454579224779380, 47.16908566558144855 ) ) ;
#29471 = CARTESIAN_POINT ( 'NONE',  ( 79.10241889060681331, -5.935454207752202116, 16.07118271501078510 ) ) ;
#29472 = CARTESIAN_POINT ( 'NONE',  ( -43.68921302925062378, 1.179890886355840163, 39.44930799450052916 ) ) ;
#29473 = CYLINDRICAL_SURFACE ( 'NONE', #3248, 25.00000000000000000 ) ;
#29474 = CARTESIAN_POINT ( 'NONE',  ( -40.46271621608484281, 3.081581074246047880, 37.04930799450052348 ) ) ;
#29475 = FILL_AREA_STYLE ('',( #21583 ) ) ;
#29476 = EDGE_LOOP ( 'NONE', ( #31622, #26340, #17300, #15785 ) ) ;
#29477 = CYLINDRICAL_SURFACE ( 'NONE', #12680, 37.50000000000000711 ) ;
#29478 = CARTESIAN_POINT ( 'NONE',  ( 21.09785597605719332, 25.56454579224779877, 58.84930799450049221 ) ) ;
#29479 = ORIENTED_EDGE ( 'NONE', *, *, #22250, .T. ) ;
#29480 = EDGE_CURVE ( 'NONE', #16381, #382, #5056, .T. ) ;
#29481 = CARTESIAN_POINT ( 'NONE',  ( -63.90214402394282445, -5.935454207752198563, 77.87546120947918382 ) ) ;
#29482 = CIRCLE ( 'NONE', #1674, 94.94530576803560962 ) ;
#29483 = CARTESIAN_POINT ( 'NONE',  ( 33.71785032049136532, 25.71664230456640254, 47.04930799450051637 ) ) ;
#29484 = AXIS2_PLACEMENT_3D ( 'NONE', #20696, #20858, #11023 ) ;
#29485 = ORIENTED_EDGE ( 'NONE', *, *, #24457, .F. ) ;
#29486 = PRODUCT_DEFINITION_SHAPE ( 'NONE', 'NONE',  #17544 ) ;
#29487 = EDGE_LOOP ( 'NONE', ( #14418, #26521, #25428, #3406, #2635 ) ) ;
#29488=STYLED_ITEM('',(#32515),#1464);
#29489 = ORIENTED_EDGE ( 'NONE', *, *, #16961, .T. ) ;
#29490 = AXIS2_PLACEMENT_3D ( 'NONE', #21949, #16701, #1781 ) ;
#29491 = EDGE_CURVE ( 'NONE', #18936, #17919, #23650, .T. ) ;
#29492 = B_SPLINE_CURVE_WITH_KNOTS ( 'NONE', 3,
 ( #6725, #21815, #4093, #1800, #4426, #32000, #29050, #13797, #3945, #23953, #24120, #14448, #14287, #1469, #21652, #6571, #1636, #16564, #1957, #3775, #11660, #31680, #8863, #26265, #21970, #11487, #6243, #24284, #19021, #11823, #9519, #21484, #31835, #28727, #21318, #31523 ),
 .UNSPECIFIED., .F., .F.,
 ( 4, 2, 2, 2, 2, 2, 2, 2, 2, 2, 2, 2, 2, 2, 2, 2, 2, 4 ),
 ( 2.453269466693398698E-18, 0.001253900128824240621, 0.001880850193236375352, 0.002507800257648510299, 0.003134750322060645029, 0.003761700386472778893, 0.005015600515297048353, 0.005642550579709183084, 0.006269500644121316947, 0.007523400772945588143, 0.008777300901769856736, 0.01003120103059412793, 0.01253900128824268247, 0.01504680154589123874, 0.01630070167471552034, 0.01755460180353980021, 0.01880850193236408008, 0.02006240206118835995 ),
 .UNSPECIFIED. ) ;
#29493 = EDGE_CURVE ( 'NONE', #15722, #1158, #9506, .T. ) ;
#29494 = LINE ( 'NONE', #18971, #19260 ) ;
#29495 = EDGE_CURVE ( 'NONE', #3554, #16793, #30464, .T. ) ;
#29496 = ADVANCED_FACE ( 'NONE', ( #6025 ), #30655, .T. ) ;
#29497 = ORIENTED_EDGE ( 'NONE', *, *, #6752, .T. ) ;
#29498 = VERTEX_POINT ( 'NONE', #18483 ) ;
#29499 = DIRECTION ( 'NONE',  ( 0.9612616959383221138, 0.2756373558169876170, 0.000000000000000000 ) ) ;
#29500 = EDGE_CURVE ( 'NONE', #22128, #30310, #26252, .T. ) ;
#29501 = CIRCLE ( 'NONE', #8555, 1.290569415042096324 ) ;
#29502 = CARTESIAN_POINT ( 'NONE',  ( 47.09785597605719687, 23.12036939723557083, 47.04930799450080059 ) ) ;
#29503 = DIRECTION ( 'NONE',  ( 0.8907924397839086517, 1.100109291107994064E-16, -0.4544104193609905251 ) ) ;
#29504 = DIRECTION ( 'NONE',  ( 0.4848096202463429982, 0.8746197071393925215, 9.920727850371698576E-18 ) ) ;
#29505 = AXIS2_PLACEMENT_3D ( 'NONE', #22458, #5077, #24773 ) ;
#29506 = CARTESIAN_POINT ( 'NONE',  ( 48.91284552371730143, 28.13619643316631169, 46.12344667017377020 ) ) ;
#29507 = ORIENTED_EDGE ( 'NONE', *, *, #26257, .T. ) ;
#29508 = CARTESIAN_POINT ( 'NONE',  ( 21.09785597605719332, 40.56454579224780588, 47.04930799450051637 ) ) ;
#29509 = ORIENTED_EDGE ( 'NONE', *, *, #3614, .F. ) ;
#29510 = DIRECTION ( 'NONE',  ( 0.2756373558170082672, -0.9612616959383162296, 0.000000000000000000 ) ) ;
#29511 = ORIENTED_EDGE ( 'NONE', *, *, #20840, .F. ) ;
#29512 = DIRECTION ( 'NONE',  ( 0.000000000000000000, 0.000000000000000000, -1.000000000000000000 ) ) ;
#29513 = DIRECTION ( 'NONE',  ( 0.000000000000000000, 0.000000000000000000, 1.000000000000000000 ) ) ;
#29514 = CARTESIAN_POINT ( 'NONE',  ( 8.732853799281732776, 31.71183152705962272, 47.04930799450051637 ) ) ;
#29515 = CARTESIAN_POINT ( 'NONE',  ( 47.59785597605720397, 13.86454579224779948, 47.04930799450052348 ) ) ;
#29516 = CARTESIAN_POINT ( 'NONE',  ( 44.77625694075215534, 26.71454579807170759, 48.23360063142255427 ) ) ;
#29517 = AXIS2_PLACEMENT_3D ( 'NONE', #6030, #18643, #23265 ) ;
#29518 = CARTESIAN_POINT ( 'NONE',  ( 47.60933809039193676, 23.04411619146718238, 48.05197954673941751 ) ) ;
#29519 = LINE ( 'NONE', #27044, #177 ) ;
#29520 = EDGE_LOOP ( 'NONE', ( #23012, #16077, #14871, #2029 ) ) ;
#29521 = EDGE_CURVE ( 'NONE', #14398, #7056, #15586, .T. ) ;
#29522 = DIRECTION ( 'NONE',  ( 0.000000000000000000, 1.420067270486643379E-16, -1.000000000000000000 ) ) ;
#29523 = DIRECTION ( 'NONE',  ( 0.4544104193609905806, -6.737912671758738596E-17, 0.8907924397839087627 ) ) ;
#29524 = DIRECTION ( 'NONE',  ( -1.000000000000000000, 0.000000000000000000, 0.000000000000000000 ) ) ;
#29525 = CARTESIAN_POINT ( 'NONE',  ( 48.66090045299940670, 22.92747281079970278, 46.25196883385470414 ) ) ;
#29526 = DIRECTION ( 'NONE',  ( 1.000000000000000000, 0.000000000000000000, 0.000000000000000000 ) ) ;
#29527 = ORIENTED_EDGE ( 'NONE', *, *, #3988, .T. ) ;
#29528 = ORIENTED_EDGE ( 'NONE', *, *, #17151, .T. ) ;
#29529 = DIRECTION ( 'NONE',  ( -1.101824276508909887E-16, 1.000000000000000000, -0.000000000000000000 ) ) ;
#29530 = VERTEX_POINT ( 'NONE', #15703 ) ;
#29531 = AXIS2_PLACEMENT_3D ( 'NONE', #611, #22922, #20628 ) ;
#29532 = AXIS2_PLACEMENT_3D ( 'NONE', #19140, #4225, #23756 ) ;
#29533 = EDGE_CURVE ( 'NONE', #11078, #6225, #29943, .T. ) ;
#29534 = EDGE_CURVE ( 'NONE', #3864, #6225, #23138, .T. ) ;
#29535 = TOROIDAL_SURFACE ( 'NONE', #15387, 20.49999999999999645, 1.499999999999997780 ) ;
#29536 = AXIS2_PLACEMENT_3D ( 'NONE', #14577, #19321, #29184 ) ;
#29537 = VERTEX_POINT ( 'NONE', #11271 ) ;
#29538 = DIRECTION ( 'NONE',  ( 0.000000000000000000, 0.000000000000000000, -1.000000000000000000 ) ) ;
#29539 = CARTESIAN_POINT ( 'NONE',  ( 47.79865503179234310, 9.702389020015065313, -3.337848843846767721 ) ) ;
#29540 = CYLINDRICAL_SURFACE ( 'NONE', #10520, 0.1000000000000028644 ) ;
#29541 = EDGE_CURVE ( 'NONE', #12341, #7948, #5698, .T. ) ;
#29542 = ORIENTED_EDGE ( 'NONE', *, *, #17249, .T. ) ;
#29543 = EDGE_CURVE ( 'NONE', #13543, #22868, #10569, .T. ) ;
#29544 = DIRECTION ( 'NONE',  ( -1.101824276508909887E-16, 1.000000000000000000, -0.000000000000000000 ) ) ;
#29545 = LINE ( 'NONE', #9518, #25446 ) ;
#29546 = CARTESIAN_POINT ( 'NONE',  ( -9.880269303432738681, -5.935454207752202116, -13.48461434800281289 ) ) ;
#29547 = EDGE_LOOP ( 'NONE', ( #8673, #2827, #25368, #19829 ) ) ;
#29548 = ORIENTED_EDGE ( 'NONE', *, *, #10892, .F. ) ;
#29549 = DIRECTION ( 'NONE',  ( -1.000000000000000000, -0.000000000000000000, -3.491481338843133355E-15 ) ) ;
#29550 = ORIENTED_EDGE ( 'NONE', *, *, #15084, .F. ) ;
#29551 = CARTESIAN_POINT ( 'NONE',  ( 45.23477325667712989, 24.86454579224779593, 43.39705899138675704 ) ) ;
#29552 = CARTESIAN_POINT ( 'NONE',  ( 8.474859994195282908, 38.56284415653841791, 47.04930799450051637 ) ) ;
#29553 = FACE_OUTER_BOUND ( 'NONE', #4433, .T. ) ;
#29554 = AXIS2_PLACEMENT_3D ( 'NONE', #8319, #15701, #8165 ) ;
#29555 = FACE_OUTER_BOUND ( 'NONE', #5238, .T. ) ;
#29556 = PRESENTATION_STYLE_ASSIGNMENT (( #19357 ) ) ;
#29557 = EDGE_LOOP ( 'NONE', ( #22512, #20349, #27069, #14968 ) ) ;
#29558 = EDGE_LOOP ( 'NONE', ( #6614, #31441, #7571, #9130 ) ) ;
#29559 = DIRECTION ( 'NONE',  ( -1.000000000000000000, 0.000000000000000000, 0.000000000000000000 ) ) ;
#29560 = CARTESIAN_POINT ( 'NONE',  ( -41.04685960816998147, 9.497330455345890599, 35.54930799450052348 ) ) ;
#29561 = CIRCLE ( 'NONE', #1753, 0.1249999999999966416 ) ;
#29562 = DIRECTION ( 'NONE',  ( -1.101824276508909887E-16, 1.000000000000000000, -0.000000000000000000 ) ) ;
#29563 = ORIENTED_EDGE ( 'NONE', *, *, #21181, .T. ) ;
#29564 = CIRCLE ( 'NONE', #15404, 0.1250000000000001110 ) ;
#29565 = CARTESIAN_POINT ( 'NONE',  ( -10.80400125034478087, -5.721341737285083440, -11.23070561388631816 ) ) ;
#29566 = CARTESIAN_POINT ( 'NONE',  ( 46.89984767728661552, -13.74047052604243646, 99.38286875800068287 ) ) ;
#29567 = VERTEX_POINT ( 'NONE', #18319 ) ;
#29568 = CARTESIAN_POINT ( 'NONE',  ( -40.06561427811386267, 7.496110634155836117, 58.05249952744806308 ) ) ;
#29569 = CARTESIAN_POINT ( 'NONE',  ( 44.77625694075214824, 25.31454579807171257, 48.23360063142255427 ) ) ;
#29570 = DIRECTION ( 'NONE',  ( 0.000000000000000000, 0.000000000000000000, -1.000000000000000000 ) ) ;
#29571 = ORIENTED_EDGE ( 'NONE', *, *, #18617, .F. ) ;
#29572 = AXIS2_PLACEMENT_3D ( 'NONE', #21195, #31235, #29414 ) ;
#29573 = LINE ( 'NONE', #23824, #13506 ) ;
#29574 = CARTESIAN_POINT ( 'NONE',  ( -39.37937466094673766, 7.181451953876404559, 39.54930799450052348 ) ) ;
#29575 = CARTESIAN_POINT ( 'NONE',  ( 45.84097905237065618, 22.80400562401890241, 48.98672734302541443 ) ) ;
#29576 = CARTESIAN_POINT ( 'NONE',  ( 48.83862994770794330, 26.64118040159426570, 48.17861352429476796 ) ) ;
#29577 = EDGE_CURVE ( 'NONE', #32221, #5223, #22072, .T. ) ;
#29578 = ORIENTED_EDGE ( 'NONE', *, *, #21005, .F. ) ;
#29579 = EDGE_CURVE ( 'NONE', #11099, #14523, #4274, .T. ) ;
#29580 = CARTESIAN_POINT ( 'NONE',  ( -40.65093765668705572, 9.567768634527945792, 35.64930799450052490 ) ) ;
#29581 = DIRECTION ( 'NONE',  ( -1.000000000000000000, 0.000000000000000000, 0.000000000000000000 ) ) ;
#29582 = DIRECTION ( 'NONE',  ( 0.2250569586005206069, -0.7848668881104323702, 0.5773502691896226224 ) ) ;
#29583 = DIRECTION ( 'NONE',  ( 0.4544104193609937448, 0.000000000000000000, 0.8907924397839072084 ) ) ;
#29584 = FACE_BOUND ( 'NONE', #21190, .T. ) ;
#29585 = DIRECTION ( 'NONE',  ( 0.000000000000000000, 0.000000000000000000, 1.000000000000000000 ) ) ;
#29586 = CARTESIAN_POINT ( 'NONE',  ( -8.081090960560100456, -13.74047052604243646, 97.57784857907851972 ) ) ;
#29587 = DIRECTION ( 'NONE',  ( 0.000000000000000000, 0.000000000000000000, -1.000000000000000000 ) ) ;
#29588 = CARTESIAN_POINT ( 'NONE',  ( 8.698509210239544487, 27.84164230456639544, 47.04930799450051637 ) ) ;
#29589 = DIRECTION ( 'NONE',  ( 0.000000000000000000, 0.000000000000000000, 1.000000000000000000 ) ) ;
#29590 = ORIENTED_EDGE ( 'NONE', *, *, #30020, .T. ) ;
#29591 = CARTESIAN_POINT ( 'NONE',  ( 45.69268131687783807, 22.99884124225578574, 46.97633003370108185 ) ) ;
#29592 = CARTESIAN_POINT ( 'NONE',  ( -30.11252088733392895, 11.69089543585256230, 24.41124053607467559 ) ) ;
#29593 = DIRECTION ( 'NONE',  ( 1.234978253042719660E-16, -1.000000000000000000, -1.109335647967047851E-31 ) ) ;
#29594 = AXIS2_PLACEMENT_3D ( 'NONE', #23680, #31873, #6760 ) ;
#29595 = ORIENTED_EDGE ( 'NONE', *, *, #19814, .F. ) ;
#29596 =( BOUNDED_CURVE ( )  B_SPLINE_CURVE ( 3, ( #2091, #22600, #17350, #24411 ),
 .UNSPECIFIED., .F., .F. ) 
 B_SPLINE_CURVE_WITH_KNOTS ( ( 4, 4 ),
 ( 1.099063246724956588, 1.220321128156879542 ),
 .UNSPECIFIED. ) 
 CURVE ( )  GEOMETRIC_REPRESENTATION_ITEM ( )  RATIONAL_B_SPLINE_CURVE ( ( 1.000000000000000000, 0.9987750858034806223, 0.9987750858034806223, 1.000000000000000000 ) ) 
 REPRESENTATION_ITEM ( '' )  );
#29597 = FACE_OUTER_BOUND ( 'NONE', #15575, .T. ) ;
#29598 = CARTESIAN_POINT ( 'NONE',  ( -40.06561427811386267, 7.496110634155836117, 60.44930799450051495 ) ) ;
#29599 = AXIS2_PLACEMENT_3D ( 'NONE', #14289, #24612, #19352 ) ;
#29600 = EDGE_LOOP ( 'NONE', ( #24230, #20090 ) ) ;
#29601 = VERTEX_POINT ( 'NONE', #23095 ) ;
#29603 = AXIS2_PLACEMENT_3D ( 'NONE', #28171, #13252, #20281 ) ;
#29602 = CARTESIAN_POINT ( 'NONE',  ( -40.12425944110432852, 6.890664497466326921, 39.53069180094396984 ) ) ;
#29604 = CARTESIAN_POINT ( 'NONE',  ( -42.59697395963048194, 14.54042610638008526, 37.04930799450052348 ) ) ;
#29605 = CIRCLE ( 'NONE', #11796, 0.1999999999999918510 ) ;
#29606 = VECTOR ( 'NONE', #15432, 1000.000000000000000 ) ;
#29607 = DIRECTION ( 'NONE',  ( -1.000000000000000000, 0.000000000000000000, 0.000000000000000000 ) ) ;
#29608 = DIRECTION ( 'NONE',  ( -1.000000000000000000, 0.000000000000000000, 0.000000000000000000 ) ) ;
#29609 = CIRCLE ( 'NONE', #15445, 0.09999999999999795164 ) ;
#29610 = DIRECTION ( 'NONE',  ( -1.000000000000000000, 0.000000000000000000, 0.000000000000000000 ) ) ;
#29611 = ORIENTED_EDGE ( 'NONE', *, *, #30755, .T. ) ;
#29612 = ORIENTED_EDGE ( 'NONE', *, *, #1166, .T. ) ;
#29613 = CARTESIAN_POINT ( 'NONE',  ( 52.21187923486668581, -5.935340315990531579, 107.4212530892143889 ) ) ;
#29614 = ORIENTED_EDGE ( 'NONE', *, *, #20159, .T. ) ;
#29615 = EDGE_CURVE ( 'NONE', #12307, #10357, #7427, .T. ) ;
#29616 = AXIS2_PLACEMENT_3D ( 'NONE', #31357, #3944, #24119 ) ;
#29617 = ADVANCED_FACE ( 'NONE', ( #13266 ), #8976, .T. ) ;
#29618 = DIRECTION ( 'NONE',  ( 0.2756373558169971649, -0.9612616959383194493, 0.000000000000000000 ) ) ;
#29619 = CARTESIAN_POINT ( 'NONE',  ( 8.732853799281732776, 30.96183152705961206, 47.04930799450051637 ) ) ;
#29620 = AXIS2_PLACEMENT_3D ( 'NONE', #18543, #16090, #3620 ) ;
#29621 = EDGE_CURVE ( 'NONE', #13895, #1905, #596, .T. ) ;
#29622 = AXIS2_PLACEMENT_3D ( 'NONE', #21738, #6815, #24368 ) ;
#29623 = AXIS2_PLACEMENT_3D ( 'NONE', #14654, #14044, #12192 ) ;
#29624 = VERTEX_POINT ( 'NONE', #5873 ) ;
#29625 = DIRECTION ( 'NONE',  ( 0.000000000000000000, -1.000000000000000000, 0.000000000000000000 ) ) ;
#29626 = ORIENTED_EDGE ( 'NONE', *, *, #8234, .T. ) ;
#29627 = CIRCLE ( 'NONE', #32255, 12.62506659569710443 ) ;
#29628 = FACE_OUTER_BOUND ( 'NONE', #25176, .T. ) ;
#29629 =( NAMED_UNIT ( * ) PLANE_ANGLE_UNIT ( ) SI_UNIT ( $, .RADIAN. ) );
#29630 = CARTESIAN_POINT ( 'NONE',  ( 72.32087091261323053, 11.70027025134008625, 69.64590718380839007 ) ) ;
#29631 = EDGE_LOOP ( 'NONE', ( #25548, #22369, #30100, #23352 ) ) ;
#29632 = DIRECTION ( 'NONE',  ( 0.000000000000000000, 0.000000000000000000, 1.000000000000000000 ) ) ;
#29633 = DIRECTION ( 'NONE',  ( -0.000000000000000000, -1.000000000000000000, -0.000000000000000000 ) ) ;
#29634 = FACE_OUTER_BOUND ( 'NONE', #13943, .T. ) ;
#29635 = CARTESIAN_POINT ( 'NONE',  ( 21.09785597605720753, -5.098646251524523443, 47.04930799450052348 ) ) ;
#29636 = CARTESIAN_POINT ( 'NONE',  ( 33.72499318558949710, 27.84143805560860940, 47.04930799450051637 ) ) ;
#29637 = DIRECTION ( 'NONE',  ( 0.000000000000000000, 1.000000000000000000, -0.000000000000000000 ) ) ;
#29638 = ORIENTED_EDGE ( 'NONE', *, *, #13628, .F. ) ;
#29639 = CARTESIAN_POINT ( 'NONE',  ( 21.09785597605719332, 15.56454579224779877, 47.04930799450051637 ) ) ;
#29640 = CARTESIAN_POINT ( 'NONE',  ( 38.59785597605721108, 14.86454579224779948, 47.04930799450052348 ) ) ;
#29641 = VERTEX_POINT ( 'NONE', #25881 ) ;
#29642 = CARTESIAN_POINT ( 'NONE',  ( 8.732853799281734553, 28.97145308207318237, 47.04930799450051637 ) ) ;
#29643 = DIRECTION ( 'NONE',  ( -1.000000000000000000, 0.000000000000000000, 0.000000000000000000 ) ) ;
#29644 = ORIENTED_EDGE ( 'NONE', *, *, #21783, .T. ) ;
#29645 = CIRCLE ( 'NONE', #2906, 1.199999999999999734 ) ;
#29646 = VERTEX_POINT ( 'NONE', #10953 ) ;
#29647 = AXIS2_PLACEMENT_3D ( 'NONE', #1436, #8995, #6692 ) ;
#29648 = EDGE_CURVE ( 'NONE', #5195, #28505, #17890, .T. ) ;
#29649 = ADVANCED_FACE ( 'NONE', ( #31614 ), #13722, .T. ) ;
#29650 = COLOUR_RGB ( '',0.7921568627450980005, 0.8196078431372548767, 0.9333333333333333481 ) ;
#29651 = VECTOR ( 'NONE', #25344, 1000.000000000000000 ) ;
#29652 = ORIENTED_EDGE ( 'NONE', *, *, #18212, .T. ) ;
#29653 = AXIS2_PLACEMENT_3D ( 'NONE', #7380, #27397, #14923 ) ;
#29654 = B_SPLINE_CURVE_WITH_KNOTS ( 'NONE', 3,
 ( #30884, #15939, #1155, #11183, #21167, #5774, #31206, #18703 ),
 .UNSPECIFIED., .F., .F.,
 ( 4, 2, 2, 4 ),
 ( 0.000000000000000000, 4.692856542812975473E-05, 7.039284814219625840E-05, 9.385713085626276207E-05 ),
 .UNSPECIFIED. ) ;
#29655 = DIRECTION ( 'NONE',  ( 0.000000000000000000, 0.000000000000000000, 1.000000000000000000 ) ) ;
#29656 = ADVANCED_FACE ( 'NONE', ( #18954 ), #29477, .T. ) ;
#29657 = ORIENTED_EDGE ( 'NONE', *, *, #17980, .T. ) ;
#29658 = ORIENTED_EDGE ( 'NONE', *, *, #4346, .F. ) ;
#29659 = CARTESIAN_POINT ( 'NONE',  ( 78.07303900989995782, -5.485531640240845164, 14.71629385678478741 ) ) ;
#29660 = CARTESIAN_POINT ( 'NONE',  ( -44.30819669882302492, -5.921088224254131838, 53.77189712903503960 ) ) ;
#29661 = CARTESIAN_POINT ( 'NONE',  ( 21.09785597605719332, 30.36454579224779238, 60.04930799450051637 ) ) ;
#29662 = FACE_OUTER_BOUND ( 'NONE', #5566, .T. ) ;
#29663 = FACE_OUTER_BOUND ( 'NONE', #9531, .T. ) ;
#29664 = VERTEX_POINT ( 'NONE', #16342 ) ;
#29665 = CARTESIAN_POINT ( 'NONE',  ( -5.602943079677954685, 9.702389020015065313, 97.51081847724526597 ) ) ;
#29666 = VERTEX_POINT ( 'NONE', #29149 ) ;
#29667 = CARTESIAN_POINT ( 'NONE',  ( -34.19711200706005627, -2.717459485359273508, 13.31095004307637097 ) ) ;
#29669 = CARTESIAN_POINT ( 'NONE',  ( -39.50554051497144314, 7.696103224718195968, 32.14930799450051779 ) ) ;
#29668 = VECTOR ( 'NONE', #12489, 1000.000000000000000 ) ;
#29670 = AXIS2_PLACEMENT_3D ( 'NONE', #7062, #24452, #17063 ) ;
#29671 = EDGE_LOOP ( 'NONE', ( #1615, #13040, #15861, #11740 ) ) ;
#29672 = CARTESIAN_POINT ( 'NONE',  ( 81.54161849434414933, -5.937448199248381187, 77.92687966219790496 ) ) ;
#29673 = CARTESIAN_POINT ( 'NONE',  ( -41.08785830660042393, 9.277514380576530328, 35.49072935073782986 ) ) ;
#29674 = DIRECTION ( 'NONE',  ( -1.188208965918165239E-16, -1.880121038077813132E-16, -1.000000000000000000 ) ) ;
#29675 = CARTESIAN_POINT ( 'NONE',  ( 33.46699938050302592, 32.22145308207317527, 47.04930799450050927 ) ) ;
#29676 = LINE ( 'NONE', #12774, #28986 ) ;
#29677 = CARTESIAN_POINT ( 'NONE',  ( 48.18662509608405031, 29.29624452788248234, 49.18364984542562013 ) ) ;
#29678 = CARTESIAN_POINT ( 'NONE',  ( 47.73724253767792192, 22.99884124225578219, 48.30271392650413276 ) ) ;
#29679 = CARTESIAN_POINT ( 'NONE',  ( 33.46699938050303302, 38.56284415653841791, 47.04930799450051637 ) ) ;
#29680 = EDGE_CURVE ( 'NONE', #3586, #18233, #19464, .T. ) ;
#29681 = ORIENTED_EDGE ( 'NONE', *, *, #31212, .F. ) ;
#29682 = FACE_OUTER_BOUND ( 'NONE', #99, .T. ) ;
#29683 = CARTESIAN_POINT ( 'NONE',  ( 33.71785032049097453, 31.21664230456641675, 47.04930799450051637 ) ) ;
#29684 = EDGE_CURVE ( 'NONE', #17205, #17361, #5345, .T. ) ;
#29685 = AXIS2_PLACEMENT_3D ( 'NONE', #1874, #14361, #6478 ) ;
#29686 = CYLINDRICAL_SURFACE ( 'NONE', #14803, 0.9031915329475500576 ) ;
#29687 = CARTESIAN_POINT ( 'NONE',  ( -38.57628410747783221, 11.92558985988973497, 26.63511333407100778 ) ) ;
#29688 = ORIENTED_EDGE ( 'NONE', *, *, #11481, .F. ) ;
#29689 = ORIENTED_EDGE ( 'NONE', *, *, #10404, .F. ) ;
#29690 = DIRECTION ( 'NONE',  ( -0.000000000000000000, -1.000000000000000000, -0.000000000000000000 ) ) ;
#29691 = EDGE_CURVE ( 'NONE', #7282, #2007, #24184, .T. ) ;
#29692 = ADVANCED_FACE ( 'NONE', ( #4199 ), #27965, .T. ) ;
#29693 = EDGE_CURVE ( 'NONE', #14944, #28177, #6986, .T. ) ;
#29694 = VERTEX_POINT ( 'NONE', #11908 ) ;
#29695 = AXIS2_PLACEMENT_3D ( 'NONE', #9322, #23931, #31659 ) ;
#29696 = ORIENTED_EDGE ( 'NONE', *, *, #32480, .T. ) ;
#29697 = CARTESIAN_POINT ( 'NONE',  ( 45.96600969091793587, 23.04411657098542676, 47.14051579308762285 ) ) ;
#29698 = EDGE_CURVE ( 'NONE', #23541, #5196, #10048, .T. ) ;
#29699 = FACE_OUTER_BOUND ( 'NONE', #5074, .T. ) ;
#29700 = AXIS2_PLACEMENT_3D ( 'NONE', #5476, #27956, #30424 ) ;
#29701 = ORIENTED_EDGE ( 'NONE', *, *, #20379, .F. ) ;
#29702 = DIRECTION ( 'NONE',  ( -1.000000000000000000, -1.101824276508910010E-16, 0.000000000000000000 ) ) ;
#29703 = DIRECTION ( 'NONE',  ( 0.8746197071393926326, -0.4848096202463430537, -8.676864087101709653E-18 ) ) ;
#29704 = DIRECTION ( 'NONE',  ( -2.779292025043186357E-18, 1.288349127009862211E-17, -1.000000000000000000 ) ) ;
#29705 = CARTESIAN_POINT ( 'NONE',  ( 48.94625023931840957, 25.97124452788249371, 46.10640627770150246 ) ) ;
#29706 = ORIENTED_EDGE ( 'NONE', *, *, #24466, .T. ) ;
#29707 = ORIENTED_EDGE ( 'NONE', *, *, #21170, .F. ) ;
#29708 = DIRECTION ( 'NONE',  ( -0.8746197071393926326, 0.4848096202463430537, 8.676864087101709653E-18 ) ) ;
#29709 = ORIENTED_EDGE ( 'NONE', *, *, #14598, .F. ) ;
#29710 = FACE_OUTER_BOUND ( 'NONE', #12635, .T. ) ;
#29711 = DIRECTION ( 'NONE',  ( 0.8746197071393926326, -0.4848096202463430537, -8.676864087101709653E-18 ) ) ;
#29712 = CARTESIAN_POINT ( 'NONE',  ( -3.902144023942795581, -5.098646251524523443, 47.04930799450052348 ) ) ;
#29713 = FACE_OUTER_BOUND ( 'NONE', #19594, .T. ) ;
#29714 = CARTESIAN_POINT ( 'NONE',  ( 46.99023568444673771, 26.43791119454915517, 49.12151524109405898 ) ) ;
#29715 = EDGE_CURVE ( 'NONE', #18274, #13855, #23672, .T. ) ;
#29716 = ORIENTED_EDGE ( 'NONE', *, *, #11094, .T. ) ;
#29717 = EDGE_LOOP ( 'NONE', ( #31182, #7514, #274, #19956, #32121, #11259 ) ) ;
#29718 = CARTESIAN_POINT ( 'NONE',  ( 100.3079064823960493, 25.56454579224780232, 49.54930799450134771 ) ) ;
#29719 = AXIS2_PLACEMENT_3D ( 'NONE', #18357, #28387, #5906 ) ;
#29720 = DIRECTION ( 'NONE',  ( -1.000000000000000000, 0.000000000000000000, 0.000000000000000000 ) ) ;
#29721 = ADVANCED_FACE ( 'NONE', ( #16980 ), #13196, .T. ) ;
#29722 = CARTESIAN_POINT ( 'NONE',  ( 7.796202261960367252, 17.36474115922713324, 47.04930799450052348 ) ) ;
#29723 = ORIENTED_EDGE ( 'NONE', *, *, #18868, .F. ) ;
#29724 = CARTESIAN_POINT ( 'NONE',  ( 21.09785597605718266, 77.37245976740706510, 131.0041182124821830 ) ) ;
#29725 = CARTESIAN_POINT ( 'NONE',  ( -43.95628906790246759, -0.1269931775117038586, 61.94930799450052206 ) ) ;
#29726 = ORIENTED_EDGE ( 'NONE', *, *, #14390, .F. ) ;
#29727 = CARTESIAN_POINT ( 'NONE',  ( 21.09785597605719332, -15.43545420775221366, 47.04930799450051637 ) ) ;
#29728 = CARTESIAN_POINT ( 'NONE',  ( 21.09785597605720753, 13.95840365082257151, 47.04930799450052348 ) ) ;
#29729 = ADVANCED_FACE ( 'NONE', ( #6503 ), #7943, .F. ) ;
#29730 = VECTOR ( 'NONE', #7903, 1000.000000000000114 ) ;
#29731 = PLANE ( 'NONE',  #2862 ) ;
#29732 = EDGE_CURVE ( 'NONE', #9593, #30342, #26274, .T. ) ;
#29733 = ORIENTED_EDGE ( 'NONE', *, *, #13031, .F. ) ;
#29734 = VERTEX_POINT ( 'NONE', #17481 ) ;
#29735 = PLANE ( 'NONE',  #30130 ) ;
#29736 = AXIS2_PLACEMENT_3D ( 'NONE', #8603, #8916, #28469 ) ;
#29737 = CARTESIAN_POINT ( 'NONE',  ( 21.09992658989239089, 29.59164230456639899, 47.04930799450051637 ) ) ;
#29738 = CARTESIAN_POINT ( 'NONE',  ( 45.24946171279598417, 25.00784706826093640, 47.99220971130007030 ) ) ;
#29739 = VERTEX_POINT ( 'NONE', #247 ) ;
#29740 = CIRCLE ( 'NONE', #17690, 0.8999999999999983569 ) ;
#29741 = CARTESIAN_POINT ( 'NONE',  ( 21.09992658989239089, 29.09143805560861296, 47.04930799450051637 ) ) ;
#29742 = CARTESIAN_POINT ( 'NONE',  ( -42.37913764077812573, 15.23192269303852875, 35.64930799450052490 ) ) ;
#29743 = DIRECTION ( 'NONE',  ( 0.000000000000000000, -1.000000000000000000, 0.000000000000000000 ) ) ;
#29744 = PLANE ( 'NONE',  #2325 ) ;
#29745 = DIRECTION ( 'NONE',  ( -1.000000000000000000, -1.101824276508909887E-16, 0.000000000000000000 ) ) ;
#29746 = DIRECTION ( 'NONE',  ( -0.000000000000000000, -1.000000000000000000, 0.000000000000000000 ) ) ;
#29747 = CARTESIAN_POINT ( 'NONE',  ( -34.15232302351031279, -13.74047052604243646, 65.80996039395141395 ) ) ;
#29748 = CARTESIAN_POINT ( 'NONE',  ( 49.32910508985204956, 22.74928388133296764, 48.13418001454558492 ) ) ;
#29749 = PRODUCT ( 'Lower Suspension', 'Lower Suspension', '', ( #7714 ) ) ;
#29750 = DIRECTION ( 'NONE',  ( 0.000000000000000000, -0.000000000000000000, -1.000000000000000000 ) ) ;
#29751 = CARTESIAN_POINT ( 'NONE',  ( -41.07560527903737579, 9.385057823277966449, 34.64930799450051779 ) ) ;
#29752 = ORIENTED_EDGE ( 'NONE', *, *, #12275, .T. ) ;
#29753 = ORIENTED_EDGE ( 'NONE', *, *, #17254, .T. ) ;
#29754 = DIRECTION ( 'NONE',  ( -1.000000000000000000, 0.000000000000000000, 0.000000000000000000 ) ) ;
#29755 = DIRECTION ( 'NONE',  ( 0.000000000000000000, -1.000000000000000000, 0.000000000000000000 ) ) ;
#29756 = LINE ( 'NONE', #19230, #402 ) ;
#29757 = FACE_OUTER_BOUND ( 'NONE', #14943, .T. ) ;
#29758 = ORIENTED_EDGE ( 'NONE', *, *, #519, .F. ) ;
#29759 = DIRECTION ( 'NONE',  ( -1.101824276508909887E-16, 1.000000000000000000, -0.000000000000000000 ) ) ;
#29760 = FACE_OUTER_BOUND ( 'NONE', #22100, .T. ) ;
#29761 = DIRECTION ( 'NONE',  ( -0.000000000000000000, -1.000000000000000000, 0.000000000000000000 ) ) ;
#29762 = ORIENTED_EDGE ( 'NONE', *, *, #20757, .F. ) ;
#29763 = VERTEX_POINT ( 'NONE', #7314 ) ;
#29764 = CARTESIAN_POINT ( 'NONE',  ( -40.11027759654395197, 6.823245743731469304, 39.47270689035109115 ) ) ;
#29765 = CARTESIAN_POINT ( 'NONE',  ( -39.57405207560572791, -5.935416493863505671, 77.98611552785908430 ) ) ;
#29766 = CARTESIAN_POINT ( 'NONE',  ( -40.18454328187963398, 7.548069831825862330, 60.44930799450051495 ) ) ;
#29767 = AXIS2_PLACEMENT_3D ( 'NONE', #22116, #1612, #4402 ) ;
#29768 = EDGE_CURVE ( 'NONE', #18804, #23918, #32073, .T. ) ;
#29769 = CARTESIAN_POINT ( 'NONE',  ( 33.46699938050304013, 27.46183152705960850, 47.04930799450051637 ) ) ;
#29770 = EDGE_CURVE ( 'NONE', #15058, #12822, #4789, .T. ) ;
#29771 = DIRECTION ( 'NONE',  ( -1.000000000000000000, 0.000000000000000000, 0.000000000000000000 ) ) ;
#29772 = CIRCLE ( 'NONE', #29789, 0.2999999999999986011 ) ;
#29773 = EDGE_LOOP ( 'NONE', ( #28460, #28169, #31782, #16122 ) ) ;
#29774 = AXIS2_PLACEMENT_3D ( 'NONE', #16634, #21563, #6643 ) ;
#29775 = ORIENTED_EDGE ( 'NONE', *, *, #25047, .T. ) ;
#29776 = CARTESIAN_POINT ( 'NONE',  ( 21.09785597605719332, 34.11266481626051217, 34.56516646732339382 ) ) ;
#29777 = EDGE_LOOP ( 'NONE', ( #2564, #18700, #8781, #6360 ) ) ;
#29778 = B_SPLINE_CURVE_WITH_KNOTS ( 'NONE', 3,
 ( #25231, #29998, #22595, #14897, #17833, #20288, #15216, #114, #10136, #7513 ),
 .UNSPECIFIED., .F., .F.,
 ( 4, 2, 2, 2, 4 ),
 ( 0.000000000000000000, 0.0008384749106984304813, 0.001257712366047627778, 0.001467331093722245563, 0.001676949821396863131 ),
 .UNSPECIFIED. ) ;
#29779 = DIRECTION ( 'NONE',  ( -1.000000000000000000, 0.000000000000000000, 0.000000000000000000 ) ) ;
#29780 = DIRECTION ( 'NONE',  ( -1.101824276508909887E-16, 1.000000000000000000, -0.000000000000000000 ) ) ;
#29781 = CIRCLE ( 'NONE', #15625, 12.62506659569710266 ) ;
#29782 = AXIS2_PLACEMENT_3D ( 'NONE', #24552, #29821, #29982 ) ;
#29783 = ORIENTED_EDGE ( 'NONE', *, *, #30135, .F. ) ;
#29784 = CARTESIAN_POINT ( 'NONE',  ( -40.84548646114599535, 8.466718295361152613, 34.60485935866290674 ) ) ;
#29785 = ORIENTED_EDGE ( 'NONE', *, *, #15044, .F. ) ;
#29786 = AXIS2_PLACEMENT_3D ( 'NONE', #27979, #243, #15655 ) ;
#29787 = DIRECTION ( 'NONE',  ( 1.000000000000000000, 0.000000000000000000, 0.000000000000000000 ) ) ;
#29788 =( BOUNDED_CURVE ( )  B_SPLINE_CURVE ( 3, ( #20451, #28174, #912, #5859 ),
 .UNSPECIFIED., .F., .F. ) 
 B_SPLINE_CURVE_WITH_KNOTS ( ( 4, 4 ),
 ( 4.712388980384698556, 5.497787143782109531 ),
 .UNSPECIFIED. ) 
 CURVE ( )  GEOMETRIC_REPRESENTATION_ITEM ( )  RATIONAL_B_SPLINE_CURVE ( ( 1.000000000000000000, 0.9492530216741960070, 0.9492530216741960070, 1.000000000000000000 ) ) 
 REPRESENTATION_ITEM ( '' )  );
#29789 = AXIS2_PLACEMENT_3D ( 'NONE', #22608, #2269, #7526 ) ;
#29790 = CARTESIAN_POINT ( 'NONE',  ( -41.56459318755936749, 7.281738416154046156, 60.54930799450051637 ) ) ;
#29791 = DIRECTION ( 'NONE',  ( 0.000000000000000000, -0.2756373558169902815, -0.9612616959383214477 ) ) ;
#29792 = ORIENTED_EDGE ( 'NONE', *, *, #5943, .T. ) ;
#29793 = CARTESIAN_POINT ( 'NONE',  ( 77.87624645123068490, -5.321843574075664662, 79.54248989857433116 ) ) ;
#29794 = CARTESIAN_POINT ( 'NONE',  ( 33.46699938050304013, 38.56284415653841791, 47.04930799450051637 ) ) ;
#29795 = DIRECTION ( 'NONE',  ( -1.000000000000000000, 0.000000000000000000, 0.000000000000000000 ) ) ;
#29796 = CARTESIAN_POINT ( 'NONE',  ( 8.698509210239512512, 24.59164230456639544, 47.04930799450051637 ) ) ;
#29797 = CARTESIAN_POINT ( 'NONE',  ( 21.09992658989238734, 38.56284415653841791, 47.04930799450051637 ) ) ;
#29798 = AXIS2_PLACEMENT_3D ( 'NONE', #29742, #7585, #25139 ) ;
#29799 = LINE ( 'NONE', #25030, #6884 ) ;
#29800 = ORIENTED_EDGE ( 'NONE', *, *, #29577, .F. ) ;
#29801 = CARTESIAN_POINT ( 'NONE',  ( 21.09785597605720753, 14.86454579224779948, 47.04930799450052348 ) ) ;
#29802 = CYLINDRICAL_SURFACE ( 'NONE', #27445, 0.9031915329475500576 ) ;
#29803 = ORIENTED_EDGE ( 'NONE', *, *, #8269, .F. ) ;
#29804 = CARTESIAN_POINT ( 'NONE',  ( 21.09785597605719332, 34.11266481626051217, 47.04930799450051637 ) ) ;
#29805 = EDGE_CURVE ( 'NONE', #17230, #4784, #15289, .T. ) ;
#29806 = LINE ( 'NONE', #19944, #31624 ) ;
#29807 = ADVANCED_FACE ( 'NONE', ( #17311 ), #3727, .T. ) ;
#29808 = EDGE_CURVE ( 'NONE', #13651, #9009, #25254, .T. ) ;
#29809 = ORIENTED_EDGE ( 'NONE', *, *, #7611, .T. ) ;
#29810 = EDGE_CURVE ( 'NONE', #1894, #13157, #17365, .T. ) ;
#29811 = VERTEX_POINT ( 'NONE', #9780 ) ;
#29812 = EDGE_CURVE ( 'NONE', #32455, #2915, #30479, .T. ) ;
#29813 = ADVANCED_FACE ( 'NONE', ( #27655 ), #29449, .T. ) ;
#29814 = AXIS2_PLACEMENT_3D ( 'NONE', #6402, #11175, #31198 ) ;
#29815 = VECTOR ( 'NONE', #18684, 1000.000000000000114 ) ;
#29816 = ORIENTED_EDGE ( 'NONE', *, *, #20850, .T. ) ;
#29817 = AXIS2_PLACEMENT_3D ( 'NONE', #5258, #20184, #10513 ) ;
#29818 = AXIS2_PLACEMENT_3D ( 'NONE', #287, #5549, #8492 ) ;
#29819 = TOROIDAL_SURFACE ( 'NONE', #5192, 3.700000000000000178, 0.5000000000000002220 ) ;
#29820 = EDGE_CURVE ( 'NONE', #10313, #31117, #2166, .T. ) ;
#29821 = DIRECTION ( 'NONE',  ( -0.000000000000000000, 1.000000000000000000, -0.000000000000000000 ) ) ;
#29822 = ORIENTED_EDGE ( 'NONE', *, *, #12262, .T. ) ;
#29823 = VERTEX_POINT ( 'NONE', #30133 ) ;
#29824 = CARTESIAN_POINT ( 'NONE',  ( 21.09992658989238734, 38.56284415653841791, 47.04930799450051637 ) ) ;
#29825 = DIRECTION ( 'NONE',  ( -1.000000000000000000, -1.101824276508909887E-16, 0.000000000000000000 ) ) ;
#29826 = SPHERICAL_SURFACE ( 'NONE', #6000, 36.51080762834750715 ) ;
#29827 = CARTESIAN_POINT ( 'NONE',  ( 21.09992658989238734, 31.84164230456639544, 47.04930799450051637 ) ) ;
#29828 = DIRECTION ( 'NONE',  ( 0.000000000000000000, 0.000000000000000000, -1.000000000000000000 ) ) ;
#29829 = EDGE_CURVE ( 'NONE', #20710, #20780, #21549, .T. ) ;
#29830 = ORIENTED_EDGE ( 'NONE', *, *, #17900, .T. ) ;
#29831 = DIRECTION ( 'NONE',  ( 0.8746197071393925215, -0.4848096202463429982, -8.676864087101708112E-18 ) ) ;
#29832 = VERTEX_POINT ( 'NONE', #15185 ) ;
#29833 = CARTESIAN_POINT ( 'NONE',  ( -36.50219711772859910, -5.247624208983634908, 14.46472410127245212 ) ) ;
#29834 = DIRECTION ( 'NONE',  ( -0.4441739386572048920, -0.2110602665713094683, -0.8707256032141200697 ) ) ;
#29835 = EDGE_LOOP ( 'NONE', ( #21, #3718, #29934, #4611 ) ) ;
#29836 = CARTESIAN_POINT ( 'NONE',  ( 21.09785597605719332, 15.24673779880127356, 33.56516646732238485 ) ) ;
#29837 = CARTESIAN_POINT ( 'NONE',  ( -40.69193635511749108, 9.347952559758585522, 39.44930799450052206 ) ) ;
#29838 = AXIS2_PLACEMENT_3D ( 'NONE', #19946, #29977, #17493 ) ;
#29839 = DIRECTION ( 'NONE',  ( -1.188208965918165239E-16, -1.880121038077813132E-16, -1.000000000000000000 ) ) ;
#29840 = CARTESIAN_POINT ( 'NONE',  ( 47.22573328838134188, 23.12036939723557083, 47.29998918090146987 ) ) ;
#29841 = CARTESIAN_POINT ( 'NONE',  ( 8.474859994195281132, 38.56284415653841791, 47.04930799450051637 ) ) ;
#29842 = CARTESIAN_POINT ( 'NONE',  ( 45.35708200440645044, 26.90457786121582018, 45.92000246470679770 ) ) ;
#29843 = CARTESIAN_POINT ( 'NONE',  ( 21.09785597605720753, 14.86454579224779948, 47.04930799450052348 ) ) ;
#29844 = DIRECTION ( 'NONE',  ( -1.000000000000000000, 0.000000000000000000, 0.000000000000000000 ) ) ;
#29845 = VERTEX_POINT ( 'NONE', #17142 ) ;
#29846 = CARTESIAN_POINT ( 'NONE',  ( -40.23967075304302909, 7.740322171013528596, 53.80788663826320573 ) ) ;
#29847 = CARTESIAN_POINT ( 'NONE',  ( 45.96182992765471909, 15.77906836436399374, 44.82232689504101586 ) ) ;
#29848 = EDGE_LOOP ( 'NONE', ( #6127, #8171, #18169, #21511 ) ) ;
#29849 = AXIS2_PLACEMENT_3D ( 'NONE', #18197, #5259, #15269 ) ;
#29850 = DIRECTION ( 'NONE',  ( -1.000000000000000000, 0.000000000000000000, 0.000000000000000000 ) ) ;
#29851 = DIRECTION ( 'NONE',  ( -1.101824276508909887E-16, 1.000000000000000000, -0.000000000000000000 ) ) ;
#29852 = EDGE_LOOP ( 'NONE', ( #13710, #11777, #24596, #7044 ) ) ;
#29853 = EDGE_CURVE ( 'NONE', #27647, #3840, #11605, .T. ) ;
#29854 = CONICAL_SURFACE ( 'NONE', #4152, 40.18714373493281755, 0.6632251157578421541 ) ;
#29855 = ORIENTED_EDGE ( 'NONE', *, *, #589, .F. ) ;
#29856 = PLANE ( 'NONE',  #22521 ) ;
#29857 = ADVANCED_FACE ( 'NONE', ( #4683 ), #29969, .T. ) ;
#29858 = VERTEX_POINT ( 'NONE', #17801 ) ;
#29859 = TOROIDAL_SURFACE ( 'NONE', #17253, 12.61792373059896555, 0.1249999999999975853 ) ;
#29860 = CIRCLE ( 'NONE', #11000, 5.099019513592786268 ) ;
#29861 = EDGE_LOOP ( 'NONE', ( #15675, #5730, #735, #741 ) ) ;
#29862 = CARTESIAN_POINT ( 'NONE',  ( 46.94469835654546586, 23.12036939723557083, 47.28539358874152043 ) ) ;
#29863 = FACE_OUTER_BOUND ( 'NONE', #5248, .T. ) ;
#29864 = EDGE_CURVE ( 'NONE', #31848, #27545, #1643, .T. ) ;
#29865 = AXIS2_PLACEMENT_3D ( 'NONE', #27053, #32150, #7365 ) ;
#29866 = ORIENTED_EDGE ( 'NONE', *, *, #13757, .T. ) ;
#29867 = CIRCLE ( 'NONE', #24088, 0.1000000000000008660 ) ;
#29868 = DIRECTION ( 'NONE',  ( -0.000000000000000000, -0.000000000000000000, 1.000000000000000000 ) ) ;
#29869 = DIRECTION ( 'NONE',  ( 1.000000000000000000, 0.000000000000000000, 0.000000000000000000 ) ) ;
#29870 = CARTESIAN_POINT ( 'NONE',  ( 48.16694854572211426, 29.31789516297709142, 49.14507740233662503 ) ) ;
#29871 = EDGE_CURVE ( 'NONE', #30753, #19067, #31038, .T. ) ;
#29872 = ORIENTED_EDGE ( 'NONE', *, *, #27674, .T. ) ;
#29873 = EDGE_LOOP ( 'NONE', ( #28685, #32163, #14130, #32002 ) ) ;
#29874 = CARTESIAN_POINT ( 'NONE',  ( 21.09992658989239089, 25.71664230456640254, 47.04930799450051637 ) ) ;
#29875 = EDGE_CURVE ( 'NONE', #16357, #9876, #24206, .T. ) ;
#29876 = VERTEX_POINT ( 'NONE', #28470 ) ;
#29877 = DIRECTION ( 'NONE',  ( 0.000000000000000000, 0.000000000000000000, -1.000000000000000000 ) ) ;
#29878 = CARTESIAN_POINT ( 'NONE',  ( 21.09785597605719332, 6.671061906060458568, 47.04930799450051637 ) ) ;
#29879 = CARTESIAN_POINT ( 'NONE',  ( -40.23847960489091236, 6.935107575317837281, 34.54930799450052348 ) ) ;
#29880 = CARTESIAN_POINT ( 'NONE',  ( 52.18101245946036215, -5.931148802125862041, -12.49820992465276603 ) ) ;
#29881 = CARTESIAN_POINT ( 'NONE',  ( 49.49063479933183629, 27.31291119454915162, 47.17357720316391578 ) ) ;
#29882 = ORIENTED_EDGE ( 'NONE', *, *, #6408, .F. ) ;
#29883 = VERTEX_POINT ( 'NONE', #25992 ) ;
#29884 = CARTESIAN_POINT ( 'NONE',  ( 33.72499318558949710, 31.09184655352422411, 47.04930799450051637 ) ) ;
#29885 = VECTOR ( 'NONE', #9602, 1000.000000000000000 ) ;
#29886 = DIRECTION ( 'NONE',  ( -1.101824276508909887E-16, 1.000000000000000000, -0.000000000000000000 ) ) ;
#29887 = AXIS2_PLACEMENT_3D ( 'NONE', #29824, #7333, #10126 ) ;
#29888 = DIRECTION ( 'NONE',  ( -1.000000000000000000, 0.000000000000000000, 0.000000000000000000 ) ) ;
#29889 = ORIENTED_EDGE ( 'NONE', *, *, #22787, .T. ) ;
#29890 = CARTESIAN_POINT ( 'NONE',  ( 48.18662509608405742, 27.98284706826092716, 49.18364984542562013 ) ) ;
#29891 = EDGE_LOOP ( 'NONE', ( #19527, #29716, #6743, #5409 ) ) ;
#29892 = CARTESIAN_POINT ( 'NONE',  ( -40.99173213700658636, 9.305078116158229662, 39.54930799450052348 ) ) ;
#29893 = CARTESIAN_POINT ( 'NONE',  ( 33.50134396954526039, 25.34164230456639899, 47.04930799450051637 ) ) ;
#29894 = ADVANCED_FACE ( 'NONE', ( #20589 ), #6135, .F. ) ;
#29895 = AXIS2_PLACEMENT_3D ( 'NONE', #27896, #25585, #20500 ) ;
#29896 = CIRCLE ( 'NONE', #1570, 12.62506659569710266 ) ;
#29897 = DIRECTION ( 'NONE',  ( 0.000000000000000000, 0.000000000000000000, 1.000000000000000000 ) ) ;
#29898 = VECTOR ( 'NONE', #10742, 1000.000000000000000 ) ;
#29899 = CONICAL_SURFACE ( 'NONE', #16314, 67.99999999999998579, 0.5061454830783623793 ) ;
#29900 = AXIS2_PLACEMENT_3D ( 'NONE', #29068, #6589, #18560 ) ;
#29901 = EDGE_LOOP ( 'NONE', ( #27090, #24937, #6585, #21333 ) ) ;
#29902 = ORIENTED_EDGE ( 'NONE', *, *, #31668, .F. ) ;
#29903 = ADVANCED_FACE ( 'NONE', ( #11076 ), #17391, .T. ) ;
#29904 = FACE_OUTER_BOUND ( 'NONE', #11206, .T. ) ;
#29905 = DIRECTION ( 'NONE',  ( -1.000000000000000000, 0.000000000000000000, 0.000000000000000000 ) ) ;
#29906 = CARTESIAN_POINT ( 'NONE',  ( 46.55854765242722948, 27.96960992152947512, 44.51792966461572121 ) ) ;
#29907 = AXIS2_PLACEMENT_3D ( 'NONE', #31880, #9397, #14326 ) ;
#29908 = EDGE_CURVE ( 'NONE', #9365, #9700, #3514, .T. ) ;
#29909 = ORIENTED_EDGE ( 'NONE', *, *, #22445, .T. ) ;
#29910 = CARTESIAN_POINT ( 'NONE',  ( 21.09785597605719332, 40.06454579224778456, 35.04930799450050927 ) ) ;
#29911 = DIRECTION ( 'NONE',  ( 1.234978253042719660E-16, -1.000000000000000000, -1.109335647967047851E-31 ) ) ;
#29912 = CARTESIAN_POINT ( 'NONE',  ( 54.51844488531325084, -0.6526263882323822818, -6.154918745024390070 ) ) ;
#29913 = ADVANCED_FACE ( 'NONE', ( #13531 ), #23155, .T. ) ;
#29914 = CIRCLE ( 'NONE', #11052, 58.46397533894063514 ) ;
#29915 = CARTESIAN_POINT ( 'NONE',  ( 33.62634396954518223, 32.59164230456640610, 47.04930799450050927 ) ) ;
#29916 = EDGE_CURVE ( 'NONE', #22169, #17679, #7970, .T. ) ;
#29917 = FACE_OUTER_BOUND ( 'NONE', #23008, .T. ) ;
#29918 = DIRECTION ( 'NONE',  ( -1.101824276508909887E-16, 1.000000000000000000, -0.000000000000000000 ) ) ;
#29919 = CARTESIAN_POINT ( 'NONE',  ( 21.09785597605719332, -15.93545420775219945, -32.16074251183835031 ) ) ;
#29920 = DIRECTION ( 'NONE',  ( 0.000000000000000000, 0.000000000000000000, 1.000000000000000000 ) ) ;
#29921 = CARTESIAN_POINT ( 'NONE',  ( 8.732853799281738105, 29.96183152705961206, 47.04930799450051637 ) ) ;
#29922 = CIRCLE ( 'NONE', #25180, 0.1000000000000018235 ) ;
#29923 = SURFACE_STYLE_USAGE ( .BOTH. , #32376 ) ;
#29924 = ORIENTED_EDGE ( 'NONE', *, *, #23403, .F. ) ;
#29925 = VERTEX_POINT ( 'NONE', #10910 ) ;
#29926 = CIRCLE ( 'NONE', #28277, 67.18681090792856025 ) ;
#29927 = CARTESIAN_POINT ( 'NONE',  ( -40.02540636251514172, 2.839176264122877047, 57.04930799450051637 ) ) ;
#29928 = FACE_OUTER_BOUND ( 'NONE', #9921, .T. ) ;
#29929 = DIRECTION ( 'NONE',  ( -1.000000000000000000, 0.000000000000000000, 0.000000000000000000 ) ) ;
#29930 = CARTESIAN_POINT ( 'NONE',  ( 54.75981606833478565, -3.374355247260691471, 101.8796202869974508 ) ) ;
#29931 = VERTEX_POINT ( 'NONE', #23217 ) ;
#29932 = CARTESIAN_POINT ( 'NONE',  ( 21.09785597605719332, 6.547041198165487685, 26.66847926540308933 ) ) ;
#29933 = LINE ( 'NONE', #24669, #100 ) ;
#29934 = ORIENTED_EDGE ( 'NONE', *, *, #4217, .T. ) ;
#29935 = EDGE_LOOP ( 'NONE', ( #31982, #22581, #4242, #2633 ) ) ;
#29936 = CARTESIAN_POINT ( 'NONE',  ( -40.16409007829387434, 6.927803014773068924, 39.54930799450049506 ) ) ;
#29937 = CARTESIAN_POINT ( 'NONE',  ( 45.35708200440645044, 29.79118040159425718, 45.92000246470679770 ) ) ;
#29938 = AXIS2_PLACEMENT_3D ( 'NONE', #24081, #19312, #14086 ) ;
#29939 = DIRECTION ( 'NONE',  ( 0.000000000000000000, 0.000000000000000000, -1.000000000000000000 ) ) ;
#29940 = DIRECTION ( 'NONE',  ( -1.000000000000000000, 0.000000000000000000, 0.000000000000000000 ) ) ;
#29941 = EDGE_LOOP ( 'NONE', ( #30704, #18626, #15803, #21718 ) ) ;
#29942 = VERTEX_POINT ( 'NONE', #1050 ) ;
#29943 = CIRCLE ( 'NONE', #5840, 69.99901951359278485 ) ;
#29944 = EDGE_CURVE ( 'NONE', #4981, #11362, #25036, .T. ) ;
#29945 = VECTOR ( 'NONE', #14208, 1000.000000000000000 ) ;
#29946 = DIRECTION ( 'NONE',  ( 0.000000000000000000, 0.000000000000000000, 1.000000000000000000 ) ) ;
#29947 = AXIS2_PLACEMENT_3D ( 'NONE', #18913, #29107, #4148 ) ;
#29948 = EDGE_CURVE ( 'NONE', #28978, #1564, #1146, .T. ) ;
#29949 = EDGE_LOOP ( 'NONE', ( #30228, #552, #25702, #14964 ) ) ;
#29950 = DIRECTION ( 'NONE',  ( -0.9612616959383200044, -0.2756373558169954996, 1.660411357259285896E-16 ) ) ;
#29951 = CARTESIAN_POINT ( 'NONE',  ( -40.32034427004700916, 8.384459687302960873, 54.44930799450051495 ) ) ;
#29952 = TOROIDAL_SURFACE ( 'NONE', #5328, 12.61792373059895134, 0.1249999999999985151 ) ;
#29953 = ADVANCED_FACE ( 'NONE', ( #27984 ), #20015, .T. ) ;
#29954 = ORIENTED_EDGE ( 'NONE', *, *, #23494, .F. ) ;
#29955 = CARTESIAN_POINT ( 'NONE',  ( -40.78689554741473700, 8.436943771353742960, 34.55838508629864947 ) ) ;
#29956 = EDGE_LOOP ( 'NONE', ( #311, #1379, #32188, #3948 ) ) ;
#29957 = CYLINDRICAL_SURFACE ( 'NONE', #5240, 12.62506659569710266 ) ;
#29958 = CARTESIAN_POINT ( 'NONE',  ( 21.09992658989239089, 26.84164230456639899, 47.04930799450051637 ) ) ;
#29959 = FACE_OUTER_BOUND ( 'NONE', #30650, .T. ) ;
#29960 = CARTESIAN_POINT ( 'NONE',  ( 33.37634396954521776, 29.34164230456639899, 47.04930799450051637 ) ) ;
#29961 = ORIENTED_EDGE ( 'NONE', *, *, #20609, .F. ) ;
#29962 = CARTESIAN_POINT ( 'NONE',  ( 71.60189677428111565, 8.508769500014674136, 75.06167927591030775 ) ) ;
#29963 = DIRECTION ( 'NONE',  ( 0.4848096202463645921, 0.8746197071393805311, 0.000000000000000000 ) ) ;
#29964 = FACE_OUTER_BOUND ( 'NONE', #2576, .T. ) ;
#29965 = CARTESIAN_POINT ( 'NONE',  ( 21.09785597605720753, -5.098646251524523443, 47.04930799450052348 ) ) ;
#29966 = TOROIDAL_SURFACE ( 'NONE', #17907, 12.40141737965281621, 0.1249999999999985428 ) ;
#29967 = DIRECTION ( 'NONE',  ( -1.224646799147353207E-16, 0.000000000000000000, -1.000000000000000000 ) ) ;
#29968 = ORIENTED_EDGE ( 'NONE', *, *, #14617, .F. ) ;
#29969 = TOROIDAL_SURFACE ( 'NONE', #15805, 20.27643559902816861, 0.2000000000000001499 ) ;
#29970 = DIRECTION ( 'NONE',  ( -0.000000000000000000, 1.000000000000000000, -0.000000000000000000 ) ) ;
#29971 = CARTESIAN_POINT ( 'NONE',  ( -42.37913764077812573, 15.23192269303853053, 38.44930799450052206 ) ) ;
#29972 = ORIENTED_EDGE ( 'NONE', *, *, #26677, .F. ) ;
#29973 = CIRCLE ( 'NONE', #9507, 12.27641737965280200 ) ;
#29974 = DIRECTION ( 'NONE',  ( -0.000000000000000000, -1.000000000000000000, -0.000000000000000000 ) ) ;
#29975 = DIRECTION ( 'NONE',  ( 0.000000000000000000, -0.000000000000000000, -1.000000000000000000 ) ) ;
#29976 = EDGE_LOOP ( 'NONE', ( #7383, #6895, #6728, #32428 ) ) ;
#29977 = DIRECTION ( 'NONE',  ( -0.4848096202463430537, -0.8746197071393926326, -9.920727850371700117E-18 ) ) ;
#29978 = ORIENTED_EDGE ( 'NONE', *, *, #10838, .T. ) ;
#29979 = VERTEX_POINT ( 'NONE', #15833 ) ;
#29980 = AXIS2_PLACEMENT_3D ( 'NONE', #20504, #23132, #12652 ) ;
#29981 = AXIS2_PLACEMENT_3D ( 'NONE', #13225, #22888, #10429 ) ;
#29982 = DIRECTION ( 'NONE',  ( 0.000000000000000000, 0.000000000000000000, -1.000000000000000000 ) ) ;
#29983 = ADVANCED_FACE ( 'NONE', ( #20421 ), #4823, .T. ) ;
#29984 = ORIENTED_EDGE ( 'NONE', *, *, #24798, .F. ) ;
#29985 = ORIENTED_EDGE ( 'NONE', *, *, #15966, .F. ) ;
#29986 = CARTESIAN_POINT ( 'NONE',  ( 74.63411498000290578, -1.331120222581886559, 13.45026064251962694 ) ) ;
#29987 = ADVANCED_FACE ( 'NONE', ( #20749 ), #19499, .T. ) ;
#29988 = EDGE_CURVE ( 'NONE', #6679, #19118, #10598, .T. ) ;
#29989 = DIRECTION ( 'NONE',  ( -0.000000000000000000, 1.000000000000000000, -0.000000000000000000 ) ) ;
#29990 = ADVANCED_FACE ( 'NONE', ( #21218 ), #29437, .T. ) ;
#29991 = FACE_OUTER_BOUND ( 'NONE', #20723, .T. ) ;
#29992 = DIRECTION ( 'NONE',  ( -0.8389271868029121171, -1.036056831587902747E-16, -0.5442436726714897643 ) ) ;
#29993 = CARTESIAN_POINT ( 'NONE',  ( -58.11219453028166981, 25.56454579224780232, 44.54930799450023216 ) ) ;
#29994 = ORIENTED_EDGE ( 'NONE', *, *, #7805, .F. ) ;
#29995 = CARTESIAN_POINT ( 'NONE',  ( -9.930143012320160167, -5.943281723642242831, 105.0325699373949249 ) ) ;
#29996 = ORIENTED_EDGE ( 'NONE', *, *, #30400, .T. ) ;
#29997 = CARTESIAN_POINT ( 'NONE',  ( -30.26475270700094811, 9.131486844526902402, 19.66223557630849328 ) ) ;
#29998 = CARTESIAN_POINT ( 'NONE',  ( 79.63325375431691100, -5.771419034597325748, 15.25028717822974222 ) ) ;
#29999 = AXIS2_PLACEMENT_3D ( 'NONE', #2220, #25513, #12565 ) ;
#30000 = ORIENTED_EDGE ( 'NONE', *, *, #17817, .T. ) ;
#30001 = CYLINDRICAL_SURFACE ( 'NONE', #32078, 0.1000000000000006301 ) ;
#30002 = CARTESIAN_POINT ( 'NONE',  ( -40.65487266620045403, 9.475231293617264683, 39.54930799450052348 ) ) ;
#30003 = DIRECTION ( 'NONE',  ( -1.000000000000000000, 0.000000000000000000, 0.000000000000000000 ) ) ;
#30004 = CARTESIAN_POINT ( 'NONE',  ( 44.79156314060809763, 19.96454579224779380, 46.92953032342012420 ) ) ;
#30005 = DIRECTION ( 'NONE',  ( -2.779292025043186357E-18, 1.288349127009862211E-17, -1.000000000000000000 ) ) ;
#30006 = AXIS2_PLACEMENT_3D ( 'NONE', #4307, #9726, #29585 ) ;
#30007 = CARTESIAN_POINT ( 'NONE',  ( 45.24946171279598417, 29.12124452788248163, 47.99220971130007030 ) ) ;
#30008 = DIRECTION ( 'NONE',  ( -0.8746197071393926326, 0.4848096202463430537, 8.676864087101709653E-18 ) ) ;
#30009 = CARTESIAN_POINT ( 'NONE',  ( 45.82550680184641578, 24.86454579224779593, 44.55508916310584056 ) ) ;
#30010 = ORIENTED_EDGE ( 'NONE', *, *, #25684, .T. ) ;
#30011 = LINE ( 'NONE', #30175, #28197 ) ;
#30012 = ORIENTED_EDGE ( 'NONE', *, *, #26162, .F. ) ;
#30013 = AXIS2_PLACEMENT_3D ( 'NONE', #312, #27406, #25426 ) ;
#30014 = CARTESIAN_POINT ( 'NONE',  ( -40.05987053574653345, 7.506472619680472746, 39.54930799450052348 ) ) ;
#30015 = ORIENTED_EDGE ( 'NONE', *, *, #20030, .T. ) ;
#30016 = CIRCLE ( 'NONE', #10100, 0.1250000000000001110 ) ;
#30017 = VERTEX_POINT ( 'NONE', #1693 ) ;
#30018 = LINE ( 'NONE', #17531, #9409 ) ;
#30019 = VERTEX_POINT ( 'NONE', #16943 ) ;
#30020 = EDGE_CURVE ( 'NONE', #6712, #14793, #6947, .T. ) ;
#30021 = CIRCLE ( 'NONE', #5382, 65.75844861871132707 ) ;
#30022 = B_SPLINE_SURFACE_WITH_KNOTS ( 'NONE', 3, 1, ( 
 ( #4504, #2961 ),
 ( #10207, #12059 ),
 ( #13158, #5599 ),
 ( #12679, #22496 ),
 ( #5442, #189 ),
 ( #8072, #3120 ),
 ( #15288, #7739 ),
 ( #5111, #501 ),
 ( #31917, #25301 ),
 ( #28091, #7583 ),
 ( #15447, #15597 ),
 ( #17738, #2040 ) ),
 .UNSPECIFIED., .F., .F., .F.,
 ( 4, 1, 1, 1, 1, 1, 1, 1, 1, 4 ),
 ( 2, 2 ),
 ( 0.000000000000000000, 0.1905276476008422870, 0.3132527668879307448, 0.4537607744431124135, 0.6164363868674446190, 0.7844992633237182211, 0.8316956887180538827, 0.8778732246798023331, 0.9250987397538774637, 1.000000000000000000 ),
 ( 0.000000000000000000, 1.000000000000000000 ),
 .UNSPECIFIED. ) ;
#30023 = EDGE_LOOP ( 'NONE', ( #19778, #1986, #25612, #870 ) ) ;
#30024 = CIRCLE ( 'NONE', #1183, 12.36707279061065101 ) ;
#30025 = CARTESIAN_POINT ( 'NONE',  ( 45.70756922570320313, 22.95310733321322161, 47.91958190782160898 ) ) ;
#30026 = CIRCLE ( 'NONE', #23198, 0.1000000000000008243 ) ;
#30027 = ORIENTED_EDGE ( 'NONE', *, *, #3175, .T. ) ;
#30028 = ADVANCED_FACE ( 'NONE', ( #14014 ), #13852, .F. ) ;
#30029 = EDGE_CURVE ( 'NONE', #10913, #10357, #11725, .T. ) ;
#30030 = CYLINDRICAL_SURFACE ( 'NONE', #20916, 31.00000000000000000 ) ;
#30031 = EDGE_CURVE ( 'NONE', #29811, #3515, #16784, .T. ) ;
#30032 = AXIS2_PLACEMENT_3D ( 'NONE', #9619, #1739, #29643 ) ;
#30033 = CARTESIAN_POINT ( 'NONE',  ( -16.40214402394279958, -5.098646251524523443, 47.04930799450052348 ) ) ;
#30034 = CARTESIAN_POINT ( 'NONE',  ( -9.938224104479729704, -5.936921830459688465, -13.33304460041354211 ) ) ;
#30035 = EDGE_CURVE ( 'NONE', #19824, #3250, #15831, .T. ) ;
#30036 = CARTESIAN_POINT ( 'NONE',  ( 44.74832014356462651, 29.08456182964376069, 46.92728461490987257 ) ) ;
#30037 = VERTEX_POINT ( 'NONE', #6297 ) ;
#30038 = ORIENTED_EDGE ( 'NONE', *, *, #7350, .F. ) ;
#30039 = CARTESIAN_POINT ( 'NONE',  ( 47.09785597605719687, 15.77906836436399374, 47.04930799450078638 ) ) ;
#30040 = ORIENTED_EDGE ( 'NONE', *, *, #12683, .F. ) ;
#30041 = CARTESIAN_POINT ( 'NONE',  ( 21.09992658989239089, 26.34184655352419213, 47.04930799450051637 ) ) ;
#30042 = DIRECTION ( 'NONE',  ( 0.000000000000000000, -1.000000000000000000, -1.446921688628131436E-16 ) ) ;
#30043 = CARTESIAN_POINT ( 'NONE',  ( 21.09992658989239089, 27.46664230456639899, 47.04930799450051637 ) ) ;
#30044 = CARTESIAN_POINT ( 'NONE',  ( -40.61178118339597631, 9.038025460530262123, 57.04930799450051637 ) ) ;
#30045 = DIRECTION ( 'NONE',  ( -2.779292025043186357E-18, 1.288349127009862211E-17, -1.000000000000000000 ) ) ;
#30046 = PRODUCT_CONTEXT ( 'NONE', #17040, 'mechanical' ) ;
#30047 = EDGE_LOOP ( 'NONE', ( #12256, #5348, #10384, #6101 ) ) ;
#30048 = ORIENTED_EDGE ( 'NONE', *, *, #23247, .F. ) ;
#30049 = DIRECTION ( 'NONE',  ( 0.2756373558169947779, -0.9612616959383200044, 0.000000000000000000 ) ) ;
#30050 = CARTESIAN_POINT ( 'NONE',  ( 21.09992658989239089, 27.09164230456639899, 47.04930799450051637 ) ) ;
#30051 = CARTESIAN_POINT ( 'NONE',  ( 8.732853799281732776, 38.56284415653841791, 47.04930799450051637 ) ) ;
#30052 = AXIS2_PLACEMENT_3D ( 'NONE', #23764, #21621, #1770 ) ;
#30053 = VERTEX_POINT ( 'NONE', #3832 ) ;
#30054 = CARTESIAN_POINT ( 'NONE',  ( 52.17126980765626598, -5.936694392936854747, 107.4222244474858172 ) ) ;
#30055 = VECTOR ( 'NONE', #3896, 1000.000000000000000 ) ;
#30056 = VERTEX_POINT ( 'NONE', #11713 ) ;
#30057 = FACE_OUTER_BOUND ( 'NONE', #22491, .T. ) ;
#30058 = CARTESIAN_POINT ( 'NONE',  ( 21.09992658989239089, 25.46183152705960140, 47.04930799450051637 ) ) ;
#30059 = CARTESIAN_POINT ( 'NONE',  ( -63.90214402394282445, 11.92558985988973497, 26.63511333407100778 ) ) ;
#30060 = CONICAL_SURFACE ( 'NONE', #20603, 58.67217910650386159, 0.3009234521321452749 ) ;
#30061 = CIRCLE ( 'NONE', #5951, 0.1250000000000001110 ) ;
#30062 = EDGE_CURVE ( 'NONE', #30210, #7068, #1666, .T. ) ;
#30063 = EDGE_CURVE ( 'NONE', #16546, #3409, #30905, .T. ) ;
#30064 = ORIENTED_EDGE ( 'NONE', *, *, #1405, .T. ) ;
#30065 = VERTEX_POINT ( 'NONE', #26806 ) ;
#30066 = DIRECTION ( 'NONE',  ( -0.000000000000000000, -1.000000000000000000, 0.000000000000000000 ) ) ;
#30067 = DIRECTION ( 'NONE',  ( 0.000000000000000000, -1.000000000000000000, -0.000000000000000000 ) ) ;
#30068 = CARTESIAN_POINT ( 'NONE',  ( 49.98072202819530219, 27.76753733014355774, 47.19902993264913960 ) ) ;
#30069 = ORIENTED_EDGE ( 'NONE', *, *, #32352, .F. ) ;
#30070 = TOROIDAL_SURFACE ( 'NONE', #28493, 78.39999999999999147, 0.1000000000000014211 ) ;
#30071 = SPHERICAL_SURFACE ( 'NONE', #22975, 0.1000000000000000056 ) ;
#30072 = CARTESIAN_POINT ( 'NONE',  ( 21.09992658989239089, 29.46664230456640254, 47.04930799450051637 ) ) ;
#30074 = DIRECTION ( 'NONE',  ( 0.000000000000000000, -0.000000000000000000, -1.000000000000000000 ) ) ;
#30073 = CIRCLE ( 'NONE', #30006, 19.99999999999999645 ) ;
#30075 = EDGE_CURVE ( 'NONE', #3078, #3737, #11129, .T. ) ;
#30076 = DIRECTION ( 'NONE',  ( -0.000000000000000000, -1.000000000000000000, 0.000000000000000000 ) ) ;
#30077 = CARTESIAN_POINT ( 'NONE',  ( 21.09785597605720753, -5.098646251524523443, 47.04930799450052348 ) ) ;
#30078 = CYLINDRICAL_SURFACE ( 'NONE', #6541, 12.62506659569710266 ) ;
#30080 = AXIS2_PLACEMENT_3D ( 'NONE', #15834, #1051, #31256 ) ;
#30079 = CYLINDRICAL_SURFACE ( 'NONE', #13308, 0.1000000000000010325 ) ;
#30081 = CYLINDRICAL_SURFACE ( 'NONE', #20498, 12.62506659569710266 ) ;
#30082 = CARTESIAN_POINT ( 'NONE',  ( 21.09785597605720753, -16.63545420775220407, 117.6483275080933169 ) ) ;
#30083 = AXIS2_PLACEMENT_3D ( 'NONE', #23979, #23816, #29070 ) ;
#30084 = CIRCLE ( 'NONE', #8065, 12.62506659569710266 ) ;
#30085 = FACE_OUTER_BOUND ( 'NONE', #14548, .T. ) ;
#30086 = CARTESIAN_POINT ( 'NONE',  ( 21.09785597605719332, 25.56454579224779877, 75.54930799450052348 ) ) ;
#30087 =( NAMED_UNIT ( * ) PLANE_ANGLE_UNIT ( ) SI_UNIT ( $, .RADIAN. ) );
#30088 = ORIENTED_EDGE ( 'NONE', *, *, #31710, .F. ) ;
#30089 = ORIENTED_EDGE ( 'NONE', *, *, #30029, .T. ) ;
#30090 = CARTESIAN_POINT ( 'NONE',  ( 21.09785597605719332, 13.74476430820393347, 47.04930799450051637 ) ) ;
#30091 = CARTESIAN_POINT ( 'NONE',  ( 21.09992658989239089, 25.59164230456639899, 47.04930799450051637 ) ) ;
#30092 = CARTESIAN_POINT ( 'NONE',  ( 21.09992658989238734, 32.46664230456639899, 47.04930799450051637 ) ) ;
#30093 = CARTESIAN_POINT ( 'NONE',  ( 52.07598125554711999, -5.935454207752202116, 105.0538709090500333 ) ) ;
#30094 = ORIENTED_EDGE ( 'NONE', *, *, #8213, .F. ) ;
#30095 = DIRECTION ( 'NONE',  ( -1.000000000000000000, 0.000000000000000000, 0.000000000000000000 ) ) ;
#30096 = CARTESIAN_POINT ( 'NONE',  ( -40.16503835899720087, 7.510440877657823755, 38.80028690913362510 ) ) ;
#30097 = DIRECTION ( 'NONE',  ( -1.101824276508909887E-16, 1.000000000000000000, -0.000000000000000000 ) ) ;
#30098 = ADVANCED_FACE ( 'NONE', ( #31893 ), #1526, .F. ) ;
#30099 = VERTEX_POINT ( 'NONE', #21373 ) ;
#30100 = ORIENTED_EDGE ( 'NONE', *, *, #17420, .T. ) ;
#30101 = CARTESIAN_POINT ( 'NONE',  ( 21.09785597605719332, 15.56454579224779877, 47.04930799450051637 ) ) ;
#30102 = CARTESIAN_POINT ( 'NONE',  ( 47.20547626766766314, 26.87451373492759643, 44.97710074790751378 ) ) ;
#30103 = CARTESIAN_POINT ( 'NONE',  ( -14.16142858629410028, -3.295808585244882849, -3.351769630585352377 ) ) ;
#30104 = EDGE_CURVE ( 'NONE', #10889, #286, #29466, .T. ) ;
#30105 = DIRECTION ( 'NONE',  ( -1.000000000000000000, 0.000000000000000000, 0.000000000000000000 ) ) ;
#30106 = CARTESIAN_POINT ( 'NONE',  ( -12.40214402394279603, 13.86454579224779948, 47.04930799450052348 ) ) ;
#30107 = EDGE_CURVE ( 'NONE', #21817, #13209, #4686, .T. ) ;
#30108 = ADVANCED_FACE ( 'NONE', ( #29597 ), #22200, .F. ) ;
#30109 = ORIENTED_EDGE ( 'NONE', *, *, #20665, .F. ) ;
#30110 = EDGE_CURVE ( 'NONE', #20495, #29138, #28412, .T. ) ;
#30111 = VERTEX_POINT ( 'NONE', #24998 ) ;
#30112 = CARTESIAN_POINT ( 'NONE',  ( -42.59587854516874472, -0.7667456371672795035, 61.94930799450052206 ) ) ;
#30113 = CARTESIAN_POINT ( 'NONE',  ( 21.09785597605720042, -8.874820941924726370, 114.4370741995029448 ) ) ;
#30114 = EDGE_CURVE ( 'NONE', #20299, #5196, #32385, .T. ) ;
#30115 = EDGE_LOOP ( 'NONE', ( #16205, #29456, #22913, #30748 ) ) ;
#30116 = FACE_OUTER_BOUND ( 'NONE', #17886, .T. ) ;
#30117 = ORIENTED_EDGE ( 'NONE', *, *, #24553, .T. ) ;
#30118 = CARTESIAN_POINT ( 'NONE',  ( 80.31073949092039754, -5.884593569754257736, 78.41992512317908393 ) ) ;
#30119 = DIRECTION ( 'NONE',  ( -1.000000000000000000, -1.101824276508909764E-16, 0.000000000000000000 ) ) ;
#30120 = TOROIDAL_SURFACE ( 'NONE', #1255, 1.299999999999999822, 0.1000000000000000056 ) ;
#30121 = CARTESIAN_POINT ( 'NONE',  ( -43.38408989745150990, 1.111547985471240452, 60.44930799450051495 ) ) ;
#30122 = AXIS2_PLACEMENT_3D ( 'NONE', #26016, #11104, #21087 ) ;
#30123 = CARTESIAN_POINT ( 'NONE',  ( -40.69573679811334443, 6.786506765454743295, 39.45085645659242601 ) ) ;
#30124 = ORIENTED_EDGE ( 'NONE', *, *, #27873, .F. ) ;
#30125 = CARTESIAN_POINT ( 'NONE',  ( 77.73252811823751074, -5.211355130743528186, 79.66972472706787300 ) ) ;
#30126 = CYLINDRICAL_SURFACE ( 'NONE', #6383, 19.50000000000000000 ) ;
#30127 = AXIS2_PLACEMENT_3D ( 'NONE', #22343, #5288, #193 ) ;
#30128 = CARTESIAN_POINT ( 'NONE',  ( 45.99457799031791438, 29.23661293962803143, 44.88652376508412090 ) ) ;
#30129 = LINE ( 'NONE', #13053, #4591 ) ;
#30130 = AXIS2_PLACEMENT_3D ( 'NONE', #29409, #3971, #1668 ) ;
#30131 = CARTESIAN_POINT ( 'NONE',  ( 74.78853601277438656, 0.3723237022603859137, 80.12755559773067660 ) ) ;
#30132 = ORIENTED_EDGE ( 'NONE', *, *, #11524, .T. ) ;
#30133 = CARTESIAN_POINT ( 'NONE',  ( 8.474859994195286461, 24.59184655352419213, 47.04930799450051637 ) ) ;
#30134 = CARTESIAN_POINT ( 'NONE',  ( -42.22138300640814634, 14.68176690255379491, 37.04930799450052348 ) ) ;
#30135 = EDGE_CURVE ( 'NONE', #22536, #25197, #14269, .T. ) ;
#30136 = EDGE_LOOP ( 'NONE', ( #26224, #26916, #3085, #15363 ) ) ;
#30137 = CARTESIAN_POINT ( 'NONE',  ( 21.09785597605719332, 17.16451738380053271, 34.06511779397349216 ) ) ;
#30138 = EDGE_CURVE ( 'NONE', #9841, #9952, #12373, .T. ) ;
#30139 = FACE_OUTER_BOUND ( 'NONE', #14342, .T. ) ;
#30140 = EDGE_LOOP ( 'NONE', ( #17737, #32273, #5978, #1683 ) ) ;
#30141 = CARTESIAN_POINT ( 'NONE',  ( -40.02540636251514172, 2.839176264122877047, 55.04930799450051637 ) ) ;
#30142 = ORIENTED_EDGE ( 'NONE', *, *, #30696, .T. ) ;
#30143 = ADVANCED_FACE ( 'NONE', ( #10071 ), #17604, .F. ) ;
#30144 = ORIENTED_EDGE ( 'NONE', *, *, #1837, .T. ) ;
#30145 = AXIS2_PLACEMENT_3D ( 'NONE', #22007, #14644, #19875 ) ;
#30146 = CIRCLE ( 'NONE', #1826, 1.003191532947548925 ) ;
#30147 = AXIS2_PLACEMENT_3D ( 'NONE', #27186, #16680, #19634 ) ;
#30148 = AXIS2_PLACEMENT_3D ( 'NONE', #5690, #21092, #15693 ) ;
#30149 = AXIS2_PLACEMENT_3D ( 'NONE', #8186, #20649, #18175 ) ;
#30150 = CARTESIAN_POINT ( 'NONE',  ( -9.760762082419509156, -5.936463533621010313, 107.7460900765755980 ) ) ;
#30151 = CARTESIAN_POINT ( 'NONE',  ( 45.96182992765471909, 25.77822092656774799, 44.82232689504102296 ) ) ;
#30152 = ORIENTED_EDGE ( 'NONE', *, *, #29199, .T. ) ;
#30153 = ORIENTED_EDGE ( 'NONE', *, *, #17853, .T. ) ;
#30154 = CARTESIAN_POINT ( 'NONE',  ( 77.78074022173946389, -5.264348929021202217, 14.45247463199519267 ) ) ;
#30155 = CARTESIAN_POINT ( 'NONE',  ( 44.24985019830227628, 11.56016961077985350, -4.887484607911599888 ) ) ;
#30156 = DIRECTION ( 'NONE',  ( -0.9612616959383204485, -0.2756373558169933347, 1.660411357259282692E-16 ) ) ;
#30157 = CARTESIAN_POINT ( 'NONE',  ( -40.46271621608484281, 3.081581074246049212, 57.04930799450051637 ) ) ;
#30158 = DIRECTION ( 'NONE',  ( -1.101824276508909887E-16, 1.000000000000000000, -0.000000000000000000 ) ) ;
#30159 = ORIENTED_EDGE ( 'NONE', *, *, #10420, .F. ) ;
#30160 = CARTESIAN_POINT ( 'NONE',  ( 47.86511985000206693, 22.93807716476589320, 48.55339511290479493 ) ) ;
#30161 = EDGE_LOOP ( 'NONE', ( #13423, #27711, #3179, #18148 ) ) ;
#30162 = CARTESIAN_POINT ( 'NONE',  ( -34.69359713753573260, -3.406866929052813742, 13.39243194667643344 ) ) ;
#30163 = DIRECTION ( 'NONE',  ( -0.000000000000000000, -1.000000000000000000, 0.000000000000000000 ) ) ;
#30164 = ORIENTED_EDGE ( 'NONE', *, *, #31028, .F. ) ;
#30165 = CARTESIAN_POINT ( 'NONE',  ( 21.09785597605719332, 30.56554579224779644, 21.04930799450051282 ) ) ;
#30166 = FACE_OUTER_BOUND ( 'NONE', #22372, .T. ) ;
#30167 = CARTESIAN_POINT ( 'NONE',  ( -40.32034427004700916, 8.384459687302960873, 59.54930799450050927 ) ) ;
#30168 = CARTESIAN_POINT ( 'NONE',  ( 45.63968093275011029, 22.91413368675619111, 48.10984057092807831 ) ) ;
#30169 = DIRECTION ( 'NONE',  ( 0.000000000000000000, 1.000000000000000000, -0.000000000000000000 ) ) ;
#30170 = CARTESIAN_POINT ( 'NONE',  ( 48.40186567930498285, 28.82957786121581378, 45.03923535223908203 ) ) ;
#30171 = AXIS2_PLACEMENT_3D ( 'NONE', #11612, #4224, #18660 ) ;
#30172 = CARTESIAN_POINT ( 'NONE',  ( -40.05987053574653345, 7.506472619680471858, 35.39279590939684539 ) ) ;
#30173 = FACE_OUTER_BOUND ( 'NONE', #21285, .T. ) ;
#30174 = ORIENTED_EDGE ( 'NONE', *, *, #8799, .T. ) ;
#30175 = CARTESIAN_POINT ( 'NONE',  ( 48.35473289974373756, 22.86454579224779948, 45.11188864597615833 ) ) ;
#30176 = CIRCLE ( 'NONE', #30683, 12.27641737965279845 ) ;
#30177 = ORIENTED_EDGE ( 'NONE', *, *, #24071, .T. ) ;
#30178 = AXIS2_PLACEMENT_3D ( 'NONE', #8588, #1035, #8432 ) ;
#30179 = CARTESIAN_POINT ( 'NONE',  ( -42.59587854516874472, -0.7667456371672803916, 32.14930799450051779 ) ) ;
#30180 = VERTEX_POINT ( 'NONE', #4978 ) ;
#30181 = EDGE_LOOP ( 'NONE', ( #6319, #26730, #9797, #19541, #4512, #31303 ) ) ;
#30182 = DIRECTION ( 'NONE',  ( 0.8746197071393858602, -0.4848096202463547666, 0.000000000000000000 ) ) ;
#30183 = EDGE_CURVE ( 'NONE', #12727, #13855, #29933, .T. ) ;
#30184 = VERTEX_POINT ( 'NONE', #4485 ) ;
#30185 = EDGE_CURVE ( 'NONE', #5958, #11143, #18439, .T. ) ;
#30186 = EDGE_LOOP ( 'NONE', ( #6542, #3599, #6518, #10740 ) ) ;
#30187 = CARTESIAN_POINT ( 'NONE',  ( 46.79153437246152691, 23.10527845304106265, 47.52148899368456370 ) ) ;
#30188 = AXIS2_PLACEMENT_3D ( 'NONE', #5010, #25666, #12561 ) ;
#30189 = ORIENTED_EDGE ( 'NONE', *, *, #15263, .F. ) ;
#30190 = DIRECTION ( 'NONE',  ( -1.101824276508909887E-16, 1.000000000000000000, -0.000000000000000000 ) ) ;
#30191 = DIRECTION ( 'NONE',  ( -0.9986540920324801229, -1.233316085972235327E-16, -0.05186525298099629866 ) ) ;
#30192 = DIRECTION ( 'NONE',  ( 0.8746197071393926326, -0.4848096202463430537, -8.676864087101709653E-18 ) ) ;
#30193 = CARTESIAN_POINT ( 'NONE',  ( 46.00908685603034343, 26.84624452788248661, 44.91496614357595263 ) ) ;
#30194 = VERTEX_POINT ( 'NONE', #211 ) ;
#30195 = ORIENTED_EDGE ( 'NONE', *, *, #31517, .F. ) ;
#30196 = FACE_OUTER_BOUND ( 'NONE', #20667, .T. ) ;
#30197 = VERTEX_POINT ( 'NONE', #10229 ) ;
#30198 = CIRCLE ( 'NONE', #19163, 12.62506659569710266 ) ;
#30199 = CARTESIAN_POINT ( 'NONE',  ( 8.823575513742490273, 15.24673779880127356, 46.72789464899623368 ) ) ;
#30200 = PLANE ( 'NONE',  #32276 ) ;
#30201 = CARTESIAN_POINT ( 'NONE',  ( 21.09785597605720753, -16.03545420775219910, 111.5493079945005235 ) ) ;
#30202 = CARTESIAN_POINT ( 'NONE',  ( 51.92400919103565116, -5.935454207752198563, -12.64839579672098679 ) ) ;
#30203 = CARTESIAN_POINT ( 'NONE',  ( 21.09785597605719332, 11.92558985988973497, 47.04930799450051637 ) ) ;
#30204 = PRODUCT_CONTEXT ( 'NONE', #9722, 'mechanical' ) ;
#30205 = ORIENTED_EDGE ( 'NONE', *, *, #28366, .T. ) ;
#30206 = VERTEX_POINT ( 'NONE', #12034 ) ;
#30207 = DIRECTION ( 'NONE',  ( 0.9612616959383221138, 0.2756373558169876170, 0.000000000000000000 ) ) ;
#30208 = DIRECTION ( 'NONE',  ( 0.000000000000000000, 0.000000000000000000, 1.000000000000000000 ) ) ;
#30209 = DIRECTION ( 'NONE',  ( 0.000000000000000000, 0.000000000000000000, -1.000000000000000000 ) ) ;
#30210 = VERTEX_POINT ( 'NONE', #22360 ) ;
#30211 = CARTESIAN_POINT ( 'NONE',  ( 52.20929784716416577, -5.935454207834595763, 107.5147914783766510 ) ) ;
#30212 = ORIENTED_EDGE ( 'NONE', *, *, #25128, .T. ) ;
#30213 = CARTESIAN_POINT ( 'NONE',  ( -42.36153388572594736, 13.68895619636815653, 59.44930799450051495 ) ) ;
#30214 = DIRECTION ( 'NONE',  ( 0.000000000000000000, 0.000000000000000000, -1.000000000000000000 ) ) ;
#30215 = AXIS2_PLACEMENT_3D ( 'NONE', #6737, #11993, #6906 ) ;
#30216 =( GEOMETRIC_REPRESENTATION_CONTEXT ( 3 ) GLOBAL_UNCERTAINTY_ASSIGNED_CONTEXT ( ( #16665 ) ) GLOBAL_UNIT_ASSIGNED_CONTEXT ( ( #26106, #6251, #6415 ) ) REPRESENTATION_CONTEXT ( 'NONE', 'WORKASPACE' ) );
#30217 = DIRECTION ( 'NONE',  ( -1.101824276508909887E-16, 1.000000000000000000, -0.000000000000000000 ) ) ;
#30218 = EDGE_CURVE ( 'NONE', #9202, #1958, #3773, .T. ) ;
#30219 = ADVANCED_FACE ( 'NONE', ( #12534 ), #9578, .F. ) ;
#30220 = ADVANCED_FACE ( 'NONE', ( #2187 ), #12155, .F. ) ;
#30221 = EDGE_CURVE ( 'NONE', #4851, #21342, #2199, .T. ) ;
#30222 = CIRCLE ( 'NONE', #31781, 2.500000000000002220 ) ;
#30223 = ORIENTED_EDGE ( 'NONE', *, *, #6664, .T. ) ;
#30224 = ORIENTED_EDGE ( 'NONE', *, *, #25435, .F. ) ;
#30225 = DIRECTION ( 'NONE',  ( -0.8746197071393805311, 0.4848096202463645921, 1.277302113040265530E-17 ) ) ;
#30226 = CARTESIAN_POINT ( 'NONE',  ( -41.94956971822180947, 3.905757428664828890, 48.34930799450052064 ) ) ;
#30227 = CARTESIAN_POINT ( 'NONE',  ( 48.40186567930498285, 25.41618040159426783, 45.03923535223908203 ) ) ;
#30228 = ORIENTED_EDGE ( 'NONE', *, *, #7464, .F. ) ;
#30229 = LINE ( 'NONE', #23793, #31885 ) ;
#30230 = DIRECTION ( 'NONE',  ( -1.101824276508909887E-16, 1.000000000000000000, -0.000000000000000000 ) ) ;
#30231 = DIRECTION ( 'NONE',  ( -1.000000000000000000, 0.000000000000000000, 0.000000000000000000 ) ) ;
#30232 = AXIS2_PLACEMENT_3D ( 'NONE', #22151, #20183, #30207 ) ;
#30233 = CARTESIAN_POINT ( 'NONE',  ( -36.51523247376623971, 9.273102258352469818, 57.04930799450051637 ) ) ;
#30234 = PLANE ( 'NONE',  #16468 ) ;
#30235 = CYLINDRICAL_SURFACE ( 'NONE', #6035, 12.62506659569710443 ) ;
#30236 = CARTESIAN_POINT ( 'NONE',  ( -40.60330327974817521, 7.565477138576668814, 60.21714911875709220 ) ) ;
#30237 = PLANE ( 'NONE',  #18408 ) ;
#30238 = FACE_OUTER_BOUND ( 'NONE', #30664, .T. ) ;
#30239 = CARTESIAN_POINT ( 'NONE',  ( 21.09785597605718621, -12.82881809906321813, -8.911746171680242412 ) ) ;
#30240 = DIRECTION ( 'NONE',  ( 0.1949050434465267045, -0.6797146636928664831, -0.7071067811865482389 ) ) ;
#30241 = FILL_AREA_STYLE_COLOUR ( '', #5031 ) ;
#30242 = ORIENTED_EDGE ( 'NONE', *, *, #32322, .T. ) ;
#30243 = ORIENTED_EDGE ( 'NONE', *, *, #31910, .T. ) ;
#30244 = ADVANCED_FACE ( 'NONE', ( #29760 ), #13223, .F. ) ;
#30245 = FACE_OUTER_BOUND ( 'NONE', #4861, .T. ) ;
#30246 = LINE ( 'NONE', #22514, #29284 ) ;
#30247 = DIRECTION ( 'NONE',  ( 0.4848096202463636484, 0.8746197071393810862, 0.000000000000000000 ) ) ;
#30248 = CIRCLE ( 'NONE', #21836, 3.300000000000000711 ) ;
#30249 = CARTESIAN_POINT ( 'NONE',  ( 47.79865503179234310, 9.702389020015065313, 97.51081847724526597 ) ) ;
#30250 = EDGE_LOOP ( 'NONE', ( #8468, #23982, #17354, #12901 ) ) ;
#30251 = DIRECTION ( 'NONE',  ( -1.000000000000000000, 0.000000000000000000, 0.000000000000000000 ) ) ;
#30252 = DIRECTION ( 'NONE',  ( -0.8746197071393840838, 0.4848096202463581528, 0.000000000000000000 ) ) ;
#30253 = FACE_OUTER_BOUND ( 'NONE', #1463, .T. ) ;
#30254 = ORIENTED_EDGE ( 'NONE', *, *, #13229, .F. ) ;
#30255 = ORIENTED_EDGE ( 'NONE', *, *, #6844, .T. ) ;
#30256 = DIRECTION ( 'NONE',  ( 0.000000000000000000, 1.000000000000000000, -0.000000000000000000 ) ) ;
#30257 = CARTESIAN_POINT ( 'NONE',  ( 44.70507715278255745, 26.34951373492759430, 46.92503878583765697 ) ) ;
#30258 = CARTESIAN_POINT ( 'NONE',  ( 33.72499318558949710, 26.09184655352419213, 47.04930799450051637 ) ) ;
#30259 = DIRECTION ( 'NONE',  ( 0.000000000000000000, -0.000000000000000000, -1.000000000000000000 ) ) ;
#30260 = DIRECTION ( 'NONE',  ( 0.000000000000000000, -0.000000000000000000, -1.000000000000000000 ) ) ;
#30261 = ADVANCED_FACE ( 'NONE', ( #25159 ), #24726, .T. ) ;
#30262 = ORIENTED_EDGE ( 'NONE', *, *, #10158, .T. ) ;
#30263 = DIRECTION ( 'NONE',  ( -1.000000000000000000, 0.000000000000000000, 0.000000000000000000 ) ) ;
#30264 = ORIENTED_EDGE ( 'NONE', *, *, #10439, .T. ) ;
#30265 =( BOUNDED_CURVE ( )  B_SPLINE_CURVE ( 3, ( #28131, #31076, #20571, #30914 ),
 .UNSPECIFIED., .F., .F. ) 
 B_SPLINE_CURVE_WITH_KNOTS ( ( 4, 4 ),
 ( 1.099063246724960363, 1.220321128156882651 ),
 .UNSPECIFIED. ) 
 CURVE ( )  GEOMETRIC_REPRESENTATION_ITEM ( )  RATIONAL_B_SPLINE_CURVE ( ( 1.000000000000000000, 0.9987750858034806223, 0.9987750858034806223, 1.000000000000000000 ) ) 
 REPRESENTATION_ITEM ( '' )  );
#30266 = ADVANCED_FACE ( 'NONE', ( #27295 ), #10616, .T. ) ;
#30267 = DIRECTION ( 'NONE',  ( 0.4848096202463429982, 0.8746197071393925215, 9.920727850371698576E-18 ) ) ;
#30268 = CARTESIAN_POINT ( 'NONE',  ( -9.883074696779189594, -5.935345006353231589, 107.7511683020618705 ) ) ;
#30269 = EDGE_CURVE ( 'NONE', #10922, #7990, #1690, .T. ) ;
#30270 = ORIENTED_EDGE ( 'NONE', *, *, #744, .F. ) ;
#30271 = CARTESIAN_POINT ( 'NONE',  ( -40.76990606341588830, 8.436069916073961394, 34.55282792453324703 ) ) ;
#30272 = ORIENTED_EDGE ( 'NONE', *, *, #23456, .T. ) ;
#30273 = CIRCLE ( 'NONE', #27641, 12.62506659569710266 ) ;
#30274 = CARTESIAN_POINT ( 'NONE',  ( 80.74398714568756930, -5.940946157296531638, 78.01708044332235659 ) ) ;
#30275 = VECTOR ( 'NONE', #26455, 1000.000000000000227 ) ;
#30276 = FACE_OUTER_BOUND ( 'NONE', #18247, .T. ) ;
#30277 = DIRECTION ( 'NONE',  ( -0.4848096202463429982, -0.8746197071393925215, -9.920727850371698576E-18 ) ) ;
#30278 = ORIENTED_EDGE ( 'NONE', *, *, #22196, .T. ) ;
#30279 = ADVANCED_FACE ( 'NONE', ( #11465 ), #19512, .T. ) ;
#30281 = CARTESIAN_POINT ( 'NONE',  ( -9.993688792838534951, -5.936209625872266749, -13.51616825880646111 ) ) ;
#30280 = VECTOR ( 'NONE', #14992, 1000.000000000000000 ) ;
#30282 = ADVANCED_FACE ( 'NONE', ( #1129 ), #21079, .T. ) ;
#30283 = AXIS2_PLACEMENT_3D ( 'NONE', #15578, #29886, #12325 ) ;
#30284 = DIRECTION ( 'NONE',  ( -0.9612616959383194493, -0.2756373558169972759, -8.795445018804905742E-19 ) ) ;
#30285 = CARTESIAN_POINT ( 'NONE',  ( -40.76967387488526384, 8.530668925462080665, 39.44930799450052206 ) ) ;
#30286 = ORIENTED_EDGE ( 'NONE', *, *, #25899, .T. ) ;
#30287 = DIRECTION ( 'NONE',  ( -0.000000000000000000, -1.000000000000000000, 0.000000000000000000 ) ) ;
#30288 = DIRECTION ( 'NONE',  ( 0.000000000000000000, 0.000000000000000000, -1.000000000000000000 ) ) ;
#30289 = CIRCLE ( 'NONE', #14552, 1.000000000001013856 ) ;
#30290 = ORIENTED_EDGE ( 'NONE', *, *, #31390, .T. ) ;
#30291 = DIRECTION ( 'NONE',  ( -1.000000000000000000, 0.000000000000000000, 0.000000000000000000 ) ) ;
#30292 = AXIS2_PLACEMENT_3D ( 'NONE', #24693, #32248, #11569 ) ;
#30293 = CARTESIAN_POINT ( 'NONE',  ( -42.47434154250543514, 4.196643200812633978, 37.04930799450052348 ) ) ;
#30294 = VERTEX_POINT ( 'NONE', #17928 ) ;
#30295 = B_SPLINE_SURFACE_WITH_KNOTS ( 'NONE', 3, 1, ( 
 ( #19255, #29613 ),
 ( #7126, #24350 ),
 ( #4499, #9262 ),
 ( #21722, #29281 ) ),
 .UNSPECIFIED., .F., .F., .F.,
 ( 4, 4 ),
 ( 2, 2 ),
 ( 0.9911194921636459210, 1.000000000000000000 ),
 ( 0.000000000000000000, 1.000000000000000000 ),
 .UNSPECIFIED. ) ;
#30296 = DIRECTION ( 'NONE',  ( -1.000000000000000000, 0.000000000000000000, 0.000000000000000000 ) ) ;
#30297 = ORIENTED_EDGE ( 'NONE', *, *, #2623, .T. ) ;
#30298 = EDGE_CURVE ( 'NONE', #12749, #14790, #2982, .T. ) ;
#30299 = ORIENTED_EDGE ( 'NONE', *, *, #8744, .F. ) ;
#30300 = VECTOR ( 'NONE', #13140, 999.9999999999998863 ) ;
#30301 = AXIS2_PLACEMENT_3D ( 'NONE', #5036, #15043, #12261 ) ;
#30302 = CIRCLE ( 'NONE', #20875, 12.36707279061065101 ) ;
#30303 = VECTOR ( 'NONE', #1935, 1000.000000000000114 ) ;
#30304 = EDGE_CURVE ( 'NONE', #23287, #22939, #22660, .T. ) ;
#30305 = CARTESIAN_POINT ( 'NONE',  ( -41.01929587258828747, 9.401204285752058354, 34.64930799450051779 ) ) ;
#30306 = CARTESIAN_POINT ( 'NONE',  ( 21.09785597605720042, -13.56320000832927875, 47.04930799450051637 ) ) ;
#30307 = ADVANCED_FACE ( 'NONE', ( #8840 ), #11658, .T. ) ;
#30308 = ORIENTED_EDGE ( 'NONE', *, *, #20470, .F. ) ;
#30309 = TOROIDAL_SURFACE ( 'NONE', #26645, 12.40141737965282509, 0.1249999999999980849 ) ;
#30310 = VERTEX_POINT ( 'NONE', #9007 ) ;
#30311 = CARTESIAN_POINT ( 'NONE',  ( 21.09992658989239089, 29.46183152705961206, 47.04930799450051637 ) ) ;
#30312 = DIRECTION ( 'NONE',  ( -0.8746197071393926326, 0.4848096202463430537, 8.676864087101709653E-18 ) ) ;
#30313 = CARTESIAN_POINT ( 'NONE',  ( -31.35900179296935519, 11.88363633076758674, 68.52907228695418951 ) ) ;
#30314 = CARTESIAN_POINT ( 'NONE',  ( 40.09785597605721108, 14.86454579224779948, 47.04930799450052348 ) ) ;
#30315 = ORIENTED_EDGE ( 'NONE', *, *, #13912, .F. ) ;
#30316 = CARTESIAN_POINT ( 'NONE',  ( -11.90685058024091170, 0.5083845707908509759, 99.75471799201011436 ) ) ;
#30317 = ORIENTED_EDGE ( 'NONE', *, *, #8975, .F. ) ;
#30318 = DIRECTION ( 'NONE',  ( -0.000000000000000000, -1.000000000000000000, -0.000000000000000000 ) ) ;
#30319 = CARTESIAN_POINT ( 'NONE',  ( -43.86882709718853590, -0.1754741395363378920, 32.14930799450051779 ) ) ;
#30320 = EDGE_CURVE ( 'NONE', #28041, #22873, #15336, .T. ) ;
#30321 = ORIENTED_EDGE ( 'NONE', *, *, #15892, .T. ) ;
#30322 = CARTESIAN_POINT ( 'NONE',  ( 47.88116631533108603, 22.93807716476589675, 45.54480264941530265 ) ) ;
#30323 = DIRECTION ( 'NONE',  ( -0.000000000000000000, -1.000000000000000000, 0.000000000000000000 ) ) ;
#30324 = CARTESIAN_POINT ( 'NONE',  ( 21.09785597605719332, -5.935454207752083988, 47.04930799450039558 ) ) ;
#30325 = CARTESIAN_POINT ( 'NONE',  ( -41.56459318755936749, 7.281738416154046156, 53.64930799450051779 ) ) ;
#30326 = EDGE_CURVE ( 'NONE', #22362, #26708, #26334, .T. ) ;
#30327 = CARTESIAN_POINT ( 'NONE',  ( 48.83862994770794330, 27.95457786121581734, 48.17861352429476796 ) ) ;
#30328 = CARTESIAN_POINT ( 'NONE',  ( 21.09785597605719332, 13.74476430820393347, 47.04930799450051637 ) ) ;
#30329 = CARTESIAN_POINT ( 'NONE',  ( -36.30817626167056744, 11.56595247146531946, 37.04930799450052348 ) ) ;
#30330 = EDGE_LOOP ( 'NONE', ( #29830, #28794, #26277, #11833 ) ) ;
#30331 = DIRECTION ( 'NONE',  ( 0.000000000000000000, -1.000000000000000000, -0.000000000000000000 ) ) ;
#30332 = CIRCLE ( 'NONE', #17200, 2.000000000000001776 ) ;
#30333 = ORIENTED_EDGE ( 'NONE', *, *, #15234, .T. ) ;
#30334 = CIRCLE ( 'NONE', #17727, 0.1250000000000018319 ) ;
#30335 = VECTOR ( 'NONE', #174, 1000.000000000000000 ) ;
#30336 = CARTESIAN_POINT ( 'NONE',  ( -63.90214402394282445, -5.935454207752198563, 54.04930799450053058 ) ) ;
#30337 = ORIENTED_EDGE ( 'NONE', *, *, #21785, .T. ) ;
#30338 = CIRCLE ( 'NONE', #13548, 12.62506659569710266 ) ;
#30339 = ORIENTED_EDGE ( 'NONE', *, *, #28012, .F. ) ;
#30340 = CARTESIAN_POINT ( 'NONE',  ( 21.09785597605719332, -9.935454207752199451, 47.04930799450051637 ) ) ;
#30341 = AXIS2_PLACEMENT_3D ( 'NONE', #6739, #6583, #9042 ) ;
#30342 = VERTEX_POINT ( 'NONE', #5467 ) ;
#30343 = EDGE_LOOP ( 'NONE', ( #28834, #14981, #31001 ) ) ;
#30344 = EDGE_CURVE ( 'NONE', #5510, #6508, #5392, .T. ) ;
#30345 = CARTESIAN_POINT ( 'NONE',  ( 21.09785597605719687, 30.56454579224779522, 14.54930799450051460 ) ) ;
#30346 = AXIS2_PLACEMENT_3D ( 'NONE', #1588, #4541, #31955 ) ;
#30347 = CONICAL_SURFACE ( 'NONE', #21937, 58.67217910650386159, 0.3009234521321452749 ) ;
#30348 = ORIENTED_EDGE ( 'NONE', *, *, #22715, .F. ) ;
#30349 = CIRCLE ( 'NONE', #18260, 0.1250000000000001110 ) ;
#30350 = CARTESIAN_POINT ( 'NONE',  ( 21.09992658989239089, 25.84184655352419213, 47.04930799450051637 ) ) ;
#30351 = LINE ( 'NONE', #10169, #791 ) ;
#30352 = DIRECTION ( 'NONE',  ( 1.234978253042719660E-16, -1.000000000000000000, -1.109335647967047851E-31 ) ) ;
#30353 = CARTESIAN_POINT ( 'NONE',  ( 46.00908685603034343, 25.44624452788248448, 44.91496614357595263 ) ) ;
#30354 = ORIENTED_EDGE ( 'NONE', *, *, #2605, .F. ) ;
#30355 = ORIENTED_EDGE ( 'NONE', *, *, #3433, .F. ) ;
#30356 = DIRECTION ( 'NONE',  ( 0.000000000000000000, 0.000000000000000000, 1.000000000000000000 ) ) ;
#30357 = EDGE_CURVE ( 'NONE', #7173, #27205, #6221, .T. ) ;
#30358 = EDGE_LOOP ( 'NONE', ( #31108, #19193, #20009, #25572 ) ) ;
#30359 = TOROIDAL_SURFACE ( 'NONE', #16191, 12.40141737965281976, 0.1249999999999999722 ) ;
#30360 = DIRECTION ( 'NONE',  ( -1.000000000000000000, 0.000000000000000000, 0.000000000000000000 ) ) ;
#30361 = DIRECTION ( 'NONE',  ( -1.000000000000000000, 0.000000000000000000, 0.000000000000000000 ) ) ;
#30362 = FACE_OUTER_BOUND ( 'NONE', #29520, .T. ) ;
#30363 = DIRECTION ( 'NONE',  ( 0.9612616959383207815, 0.2756373558169926685, 8.795445018804289444E-19 ) ) ;
#30364 = CARTESIAN_POINT ( 'NONE',  ( -42.26497471389478733, 14.66834543456874940, 60.54930799450051637 ) ) ;
#30365 = ITEM_DEFINED_TRANSFORMATION ( 'NONE', 'NONE', #31239,  #8172 ) ;
#30366 = VERTEX_POINT ( 'NONE', #3919 ) ;
#30367 = DIRECTION ( 'NONE',  ( 0.000000000000000000, -0.000000000000000000, 1.000000000000000000 ) ) ;
#30368 = LINE ( 'NONE', #22647, #13579 ) ;
#30369 = CARTESIAN_POINT ( 'NONE',  ( -9.733400645194006273, -5.935667572904992362, 107.6074630748240537 ) ) ;
#30370 = CARTESIAN_POINT ( 'NONE',  ( 47.20547626766765603, 27.57451373492759572, 44.97710074790751378 ) ) ;
#30371 = EDGE_LOOP ( 'NONE', ( #22058, #21002, #4967, #12363 ) ) ;
#30372 = CARTESIAN_POINT ( 'NONE',  ( -43.37834615508418068, 1.121909970995875971, 34.54930799450052348 ) ) ;
#30373 = CARTESIAN_POINT ( 'NONE',  ( -42.73182147790732444, -0.8057266458565844891, 61.94930799450052206 ) ) ;
#30374 = AXIS2_PLACEMENT_3D ( 'NONE', #9272, #24205, #4509 ) ;
#30375 = AXIS2_PLACEMENT_3D ( 'NONE', #13230, #25680, #8132 ) ;
#30376 = CARTESIAN_POINT ( 'NONE',  ( -31.75494777190936802, 11.92558985988973674, 26.63511333407100778 ) ) ;
#30377 = PRODUCT_RELATED_PRODUCT_CATEGORY ( 'part', '', ( #13281 ) ) ;
#30378 = CIRCLE ( 'NONE', #18324, 12.62506659569710266 ) ;
#30379 = EDGE_LOOP ( 'NONE', ( #11639, #28814, #1618, #22411 ) ) ;
#30380 = AXIS2_PLACEMENT_3D ( 'NONE', #30340, #17363, #32478 ) ;
#30381 = ORIENTED_EDGE ( 'NONE', *, *, #30029, .F. ) ;
#30382 = DIRECTION ( 'NONE',  ( -7.588956326749211550E-18, 4.206627182996912454E-18, -1.000000000000000000 ) ) ;
#30383 = DIRECTION ( 'NONE',  ( -0.4848096202463430537, -0.8746197071393926326, -9.920727850371701658E-18 ) ) ;
#30384 = CARTESIAN_POINT ( 'NONE',  ( 48.81767175631193112, 22.89977464660286444, 46.33034145269077442 ) ) ;
#30385 = ORIENTED_EDGE ( 'NONE', *, *, #19468, .F. ) ;
#30386 = DIRECTION ( 'NONE',  ( 0.4848096202463673676, 0.8746197071393789768, 0.000000000000000000 ) ) ;
#30387 = CYLINDRICAL_SURFACE ( 'NONE', #3907, 0.1000000000000018235 ) ;
#30388 = DIRECTION ( 'NONE',  ( -1.000000000000000000, 0.000000000000000000, -1.224646799147353207E-16 ) ) ;
#30389 = CARTESIAN_POINT ( 'NONE',  ( 45.00053793792376666, 25.95920399681023127, 45.68869892245983522 ) ) ;
#30390 = AXIS2_PLACEMENT_3D ( 'NONE', #1226, #24038, #4181 ) ;
#30392 = ADVANCED_FACE ( 'NONE', ( #25482 ), #12191, .T. ) ;
#30391 = CIRCLE ( 'NONE', #13623, 0.1250000000000001110 ) ;
#30393 = PLANE ( 'NONE',  #1827 ) ;
#30394 = LINE ( 'NONE', #20695, #3397 ) ;
#30395 = DIRECTION ( 'NONE',  ( -1.000000000000000000, 0.000000000000000000, 0.000000000000000000 ) ) ;
#30396 = ADVANCED_FACE ( 'NONE', ( #14584 ), #29686, .F. ) ;
#30397 = DIRECTION ( 'NONE',  ( -0.000000000000000000, -1.000000000000000000, 0.000000000000000000 ) ) ;
#30399 = ADVANCED_FACE ( 'NONE', ( #6703 ), #24755, .F. ) ;
#30398 = DIRECTION ( 'NONE',  ( 1.234978253042719660E-16, -1.000000000000000000, -1.109335647967047851E-31 ) ) ;
#30400 = EDGE_CURVE ( 'NONE', #21242, #27995, #9500, .T. ) ;
#30401 = EDGE_CURVE ( 'NONE', #24621, #11017, #7029, .T. ) ;
#30402 = DIRECTION ( 'NONE',  ( -1.101824276508909887E-16, 1.000000000000000000, -0.000000000000000000 ) ) ;
#30403 = CARTESIAN_POINT ( 'NONE',  ( 48.78406556707242459, 22.93807716476589675, 47.13688154746046166 ) ) ;
#30404 = ORIENTED_EDGE ( 'NONE', *, *, #18518, .T. ) ;
#30405 = ORIENTED_EDGE ( 'NONE', *, *, #7981, .T. ) ;
#30406 = DIRECTION ( 'NONE',  ( 0.000000000000000000, 0.000000000000000000, 1.000000000000000000 ) ) ;
#30407 = DIRECTION ( 'NONE',  ( -1.000000000000000000, 0.000000000000000000, 0.000000000000000000 ) ) ;
#30408 = DIRECTION ( 'NONE',  ( -1.101824276508909887E-16, 1.000000000000000000, -0.000000000000000000 ) ) ;
#30409 = AXIS2_PLACEMENT_3D ( 'NONE', #26322, #6464, #24012 ) ;
#30410 = VECTOR ( 'NONE', #14841, 999.9999999999998863 ) ;
#30411 = DIRECTION ( 'NONE',  ( -0.9612616959383204485, -0.2756373558169933347, 1.660411357259282692E-16 ) ) ;
#30412 = ORIENTED_EDGE ( 'NONE', *, *, #15196, .F. ) ;
#30413 = LINE ( 'NONE', #10070, #16108 ) ;
#30414 = AXIS2_PLACEMENT_3D ( 'NONE', #10414, #7472, #15648 ) ;
#30415 = CARTESIAN_POINT ( 'NONE',  ( 48.78406556707242459, 22.93807716476589675, 47.13688154746047587 ) ) ;
#30416 = CARTESIAN_POINT ( 'NONE',  ( -40.01196617103988018, 7.363926680072800046, 38.86384274482242063 ) ) ;
#30417 = ORIENTED_EDGE ( 'NONE', *, *, #27349, .T. ) ;
#30418 = ORIENTED_EDGE ( 'NONE', *, *, #18157, .T. ) ;
#30419 = DIRECTION ( 'NONE',  ( 0.000000000000000000, -0.2756373558165849391, -0.9612616959384376880 ) ) ;
#30420 = CARTESIAN_POINT ( 'NONE',  ( 48.40186567930498285, 25.41618040159426783, 45.03923535223908203 ) ) ;
#30421 = CIRCLE ( 'NONE', #12589, 12.62506659569710266 ) ;
#30422 = CARTESIAN_POINT ( 'NONE',  ( 45.35708200440645044, 28.30457786121581876, 45.92000246470679770 ) ) ;
#30423 = DIRECTION ( 'NONE',  ( -1.000000000000000000, 0.000000000000000000, 0.000000000000000000 ) ) ;
#30424 = DIRECTION ( 'NONE',  ( -1.000000000000000000, 0.000000000000000000, 0.000000000000000000 ) ) ;
#30425 = VECTOR ( 'NONE', #4140, 1000.000000000000114 ) ;
#30426 = ORIENTED_EDGE ( 'NONE', *, *, #23480, .F. ) ;
#30427 = CARTESIAN_POINT ( 'NONE',  ( 21.09785597605719332, -5.935454207752083988, 47.04930799449963530 ) ) ;
#30428 = EDGE_CURVE ( 'NONE', #19129, #27059, #32149, .T. ) ;
#30429 = TOROIDAL_SURFACE ( 'NONE', #15724, 46.69263079098917046, 1.200000000000001954 ) ;
#30430 = VECTOR ( 'NONE', #25217, 1000.000000000000000 ) ;
#30431 = ORIENTED_EDGE ( 'NONE', *, *, #13674, .F. ) ;
#30432 = CIRCLE ( 'NONE', #14194, 2.923537884824412014 ) ;
#30433 = CARTESIAN_POINT ( 'NONE',  ( -40.02540636251514172, 2.839176264122877047, 55.14930799450051779 ) ) ;
#30434 = CARTESIAN_POINT ( 'NONE',  ( -41.01929587258828036, 9.401204285752060130, 38.64930799450052490 ) ) ;
#30435 = AXIS2_PLACEMENT_3D ( 'NONE', #14315, #26779, #1343 ) ;
#30436 = AXIS2_PLACEMENT_3D ( 'NONE', #19043, #28744, #23501 ) ;
#30437 = AXIS2_PLACEMENT_3D ( 'NONE', #29147, #1406, #4197 ) ;
#30438 = ORIENTED_EDGE ( 'NONE', *, *, #955, .F. ) ;
#30439 = LINE ( 'NONE', #12726, #29651 ) ;
#30440 = EDGE_CURVE ( 'NONE', #13364, #23946, #27052, .T. ) ;
#30441 = CARTESIAN_POINT ( 'NONE',  ( 21.09992658989239089, 25.34143805560860940, 47.04930799450051637 ) ) ;
#30442 = LINE ( 'NONE', #5333, #14678 ) ;
#30443 = ADVANCED_FACE ( 'NONE', ( #9659 ), #3265, .T. ) ;
#30444 = CARTESIAN_POINT ( 'NONE',  ( -1.500160953227123395, 11.69997306056223607, 99.14540122386770804 ) ) ;
#30445 = ADVANCED_FACE ( 'NONE', ( #31662 ), #14285, .T. ) ;
#30446 = CARTESIAN_POINT ( 'NONE',  ( 106.0978559760574029, 9.702389020015065313, 73.75010705023596813 ) ) ;
#30447 = VERTEX_POINT ( 'NONE', #14751 ) ;
#30448 = CARTESIAN_POINT ( 'NONE',  ( 21.09992658989238734, 31.22145308207317171, 47.04930799450051637 ) ) ;
#30449 = DIRECTION ( 'NONE',  ( 0.000000000000000000, -0.000000000000000000, -1.000000000000000000 ) ) ;
#30450 = AXIS2_PLACEMENT_3D ( 'NONE', #9314, #9647, #19640 ) ;
#30451 = CARTESIAN_POINT ( 'NONE',  ( 81.54157720457462233, -5.936746300155055778, 77.98036360551803625 ) ) ;
#30452 = DIRECTION ( 'NONE',  ( -1.000000000000000000, 0.000000000000000000, 0.000000000000000000 ) ) ;
#30453 = CARTESIAN_POINT ( 'NONE',  ( -40.49360782792987834, 7.147293204394356891, 38.94271047082367687 ) ) ;
#30454 = EDGE_LOOP ( 'NONE', ( #29972, #6834, #13016, #16182 ) ) ;
#30455 = CARTESIAN_POINT ( 'NONE',  ( 21.09992658989239089, 29.72145308207318237, 47.04930799450051637 ) ) ;
#30456 = VERTEX_POINT ( 'NONE', #32312 ) ;
#30457 = DIRECTION ( 'NONE',  ( -0.4848096202463431648, -0.8746197071393924105, 0.000000000000000000 ) ) ;
#30458 = FACE_OUTER_BOUND ( 'NONE', #4020, .T. ) ;
#30459 = CARTESIAN_POINT ( 'NONE',  ( 49.32483701613094240, 29.10322093266652033, 45.91328182968236860 ) ) ;
#30460 = AXIS2_PLACEMENT_3D ( 'NONE', #14902, #29839, #24910 ) ;
#30461 = DIRECTION ( 'NONE',  ( -1.000000000000000000, 0.000000000000000000, 0.000000000000000000 ) ) ;
#30462 = ORIENTED_EDGE ( 'NONE', *, *, #29948, .F. ) ;
#30463 = DIRECTION ( 'NONE',  ( 0.000000000000000000, 0.000000000000000000, -1.000000000000000000 ) ) ;
#30464 = CIRCLE ( 'NONE', #17863, 12.62506659569710443 ) ;
#30465 = AXIS2_PLACEMENT_3D ( 'NONE', #5286, #27442, #5603 ) ;
#30466 = ORIENTED_EDGE ( 'NONE', *, *, #9865, .T. ) ;
#30467 = CIRCLE ( 'NONE', #17866, 31.50000000000000000 ) ;
#30468 = AXIS2_PLACEMENT_3D ( 'NONE', #1855, #9406, #16940 ) ;
#30469 = EDGE_LOOP ( 'NONE', ( #5011, #27423 ) ) ;
#30470 =( BOUNDED_CURVE ( )  B_SPLINE_CURVE ( 3, ( #15959, #25496, #15809, #30907 ),
 .UNSPECIFIED., .F., .F. ) 
 B_SPLINE_CURVE_WITH_KNOTS ( ( 4, 4 ),
 ( 1.099063246724954812, 1.220321128156879320 ),
 .UNSPECIFIED. ) 
 CURVE ( )  GEOMETRIC_REPRESENTATION_ITEM ( )  RATIONAL_B_SPLINE_CURVE ( ( 1.000000000000000000, 0.9987750858034805113, 0.9987750858034805113, 1.000000000000000000 ) ) 
 REPRESENTATION_ITEM ( '' )  );
#30471 = EDGE_CURVE ( 'NONE', #3737, #5905, #19000, .T. ) ;
#30472 = EDGE_CURVE ( 'NONE', #7619, #18982, #24231, .T. ) ;
#30473 = DIRECTION ( 'NONE',  ( -0.7141240004913222972, 0.3958453973320028019, -0.5773502691896303940 ) ) ;
#30474 = LINE ( 'NONE', #587, #6309 ) ;
#30475 = CARTESIAN_POINT ( 'NONE',  ( 81.46980107077142463, -5.937449718911897101, 16.02633765848928249 ) ) ;
#30476 = ORIENTED_EDGE ( 'NONE', *, *, #20567, .F. ) ;
#30477 = EDGE_LOOP ( 'NONE', ( #16332, #558, #619, #20925 ) ) ;
#30478 = DIRECTION ( 'NONE',  ( 1.000000000000000000, -0.000000000000000000, 1.224646799147353207E-16 ) ) ;
#30479 = CIRCLE ( 'NONE', #16312, 12.62506659569710266 ) ;
#30480 = CARTESIAN_POINT ( 'NONE',  ( 21.09785597605720042, -17.03545420775220265, -23.54971151909227700 ) ) ;
#30481 = CARTESIAN_POINT ( 'NONE',  ( -34.18913700378557508, -2.705599144416646951, 80.78811439151294849 ) ) ;
#30482 = CARTESIAN_POINT ( 'NONE',  ( 33.72499318558949710, 29.84184655352422411, 47.04930799450051637 ) ) ;
#30483 = AXIS2_PLACEMENT_3D ( 'NONE', #16292, #26143, #31725 ) ;
#30484 = EDGE_CURVE ( 'NONE', #12175, #1564, #11800, .T. ) ;
#30485 = EDGE_LOOP ( 'NONE', ( #18943, #12131, #12594, #26509 ) ) ;
#30486 = CARTESIAN_POINT ( 'NONE',  ( -11.52256075650998035, -5.211355130743549502, 103.6839801366810292 ) ) ;
#30487 = ORIENTED_EDGE ( 'NONE', *, *, #16555, .F. ) ;
#30488 = DIRECTION ( 'NONE',  ( 1.000000000000000000, 0.000000000000000000, 0.000000000000000000 ) ) ;
#30489 = FACE_OUTER_BOUND ( 'NONE', #24847, .T. ) ;
#30490 = AXIS2_PLACEMENT_3D ( 'NONE', #9489, #6864, #31968 ) ;
#30491 = EDGE_LOOP ( 'NONE', ( #4166, #249 ) ) ;
#30492 = FACE_OUTER_BOUND ( 'NONE', #13539, .T. ) ;
#30493 = CARTESIAN_POINT ( 'NONE',  ( 8.482002859293453767, 29.46664230456640254, 47.04930799450051637 ) ) ;
#30494 = FACE_OUTER_BOUND ( 'NONE', #29976, .T. ) ;
#30495 = CARTESIAN_POINT ( 'NONE',  ( 45.24946171279598417, 24.92124452788249300, 47.99220971130007030 ) ) ;
#30496 = AXIS2_PLACEMENT_3D ( 'NONE', #1725, #8783, #14043 ) ;
#30497 = CARTESIAN_POINT ( 'NONE',  ( -40.01185171578377719, 7.339011093366132776, 35.33835236764744536 ) ) ;
#30498 = DIRECTION ( 'NONE',  ( -1.101824276508909887E-16, 1.000000000000000000, -0.000000000000000000 ) ) ;
#30499 = ORIENTED_EDGE ( 'NONE', *, *, #13205, .T. ) ;
#30500 = DIRECTION ( 'NONE',  ( -1.000000000000000000, -1.101824276508910010E-16, 0.000000000000000000 ) ) ;
#30501 = AXIS2_PLACEMENT_3D ( 'NONE', #23254, #768, #20785 ) ;
#30502 = FACE_OUTER_BOUND ( 'NONE', #28472, .T. ) ;
#30503 = ORIENTED_EDGE ( 'NONE', *, *, #4009, .F. ) ;
#30504 = EDGE_CURVE ( 'NONE', #27205, #4649, #19327, .T. ) ;
#30505 = ORIENTED_EDGE ( 'NONE', *, *, #28875, .F. ) ;
#30506 = CARTESIAN_POINT ( 'NONE',  ( 21.09992658989238734, 38.56284415653841791, 47.04930799450051637 ) ) ;
#30507 = EDGE_CURVE ( 'NONE', #24091, #13542, #5919, .T. ) ;
#30508 =( GEOMETRIC_REPRESENTATION_CONTEXT ( 3 ) GLOBAL_UNCERTAINTY_ASSIGNED_CONTEXT ( ( #23907 ) ) GLOBAL_UNIT_ASSIGNED_CONTEXT ( ( #18947, #1555, #1726 ) ) REPRESENTATION_CONTEXT ( 'NONE', 'WORKASPACE' ) );
#30509 = ORIENTED_EDGE ( 'NONE', *, *, #7951, .T. ) ;
#30510 = VECTOR ( 'NONE', #1366, 1000.000000000000000 ) ;
#30511 = EDGE_CURVE ( 'NONE', #2007, #4802, #30016, .T. ) ;
#30512 = EDGE_CURVE ( 'NONE', #7100, #15722, #26319, .T. ) ;
#30513 = ADVANCED_FACE ( 'NONE', ( #12622 ), #16353, .T. ) ;
#30514 = ORIENTED_EDGE ( 'NONE', *, *, #3709, .F. ) ;
#30515 = CARTESIAN_POINT ( 'NONE',  ( 21.09992658989239089, 29.84164230456639899, 47.04930799450051637 ) ) ;
#30516 = AXIS2_PLACEMENT_3D ( 'NONE', #4193, #21256, #9115 ) ;
#30517 = ORIENTED_EDGE ( 'NONE', *, *, #18767, .F. ) ;
#30518 = FILL_AREA_STYLE ('',( #20002 ) ) ;
#30519 = CARTESIAN_POINT ( 'NONE',  ( 21.09785597605719332, -13.49020584019834601, 47.04930799450051637 ) ) ;
#30520 = DIRECTION ( 'NONE',  ( 1.234978253042719660E-16, -1.000000000000000000, -1.109335647967047851E-31 ) ) ;
#30521 = CARTESIAN_POINT ( 'NONE',  ( 48.91284552371730143, 28.09289516297709710, 46.12344667017377020 ) ) ;
#30522 = EDGE_CURVE ( 'NONE', #25945, #29942, #10478, .T. ) ;
#30523 = ORIENTED_EDGE ( 'NONE', *, *, #14764, .F. ) ;
#30524 = ORIENTED_EDGE ( 'NONE', *, *, #27262, .F. ) ;
#30525 = CARTESIAN_POINT ( 'NONE',  ( 8.482002859293473307, 31.96664230456639544, 47.04930799450051637 ) ) ;
#30526 = ORIENTED_EDGE ( 'NONE', *, *, #12836, .F. ) ;
#30527 = AXIS2_PLACEMENT_3D ( 'NONE', #10501, #2933, #20008 ) ;
#30528 = CARTESIAN_POINT ( 'NONE',  ( 45.84097905237065618, 19.96454579224779380, 48.98672734302541443 ) ) ;
#30529 = DIRECTION ( 'NONE',  ( -0.2756373558169942228, 0.9612616959383203374, 0.000000000000000000 ) ) ;
#30530 = CARTESIAN_POINT ( 'NONE',  ( -10.74933306299440083, -5.721341737285946749, 105.3592130793008721 ) ) ;
#30531 = AXIS2_PLACEMENT_3D ( 'NONE', #11313, #28701, #6384 ) ;
#30532 = DIRECTION ( 'NONE',  ( -1.101824276508909887E-16, 1.000000000000000000, -0.000000000000000000 ) ) ;
#30533 = CARTESIAN_POINT ( 'NONE',  ( 44.70507715278255034, 25.56291119454915872, 46.92503878583767118 ) ) ;
#30534 = ORIENTED_EDGE ( 'NONE', *, *, #2683, .F. ) ;
#30535 = CARTESIAN_POINT ( 'NONE',  ( -40.60251150970604073, 6.748447833883063574, 53.54930799450051637 ) ) ;
#30536 = CARTESIAN_POINT ( 'NONE',  ( 21.09785597605720042, 12.26495659406217342, 103.5194520131186096 ) ) ;
#30537 = CARTESIAN_POINT ( 'NONE',  ( -40.28779227465695811, 2.984619150196779813, 57.04930799450051637 ) ) ;
#30538 = CARTESIAN_POINT ( 'NONE',  ( 49.49063479933183629, 26.69951373492759927, 47.17357720316391578 ) ) ;
#30539 = EDGE_CURVE ( 'NONE', #19419, #12604, #28440, .T. ) ;
#30540 = ORIENTED_EDGE ( 'NONE', *, *, #25354, .F. ) ;
#30541 = DIRECTION ( 'NONE',  ( -1.101824276508909887E-16, 1.000000000000000000, -0.000000000000000000 ) ) ;
#30542 = DIRECTION ( 'NONE',  ( -0.9612616959383198934, -0.2756373558169956106, 0.000000000000000000 ) ) ;
#30543 = EDGE_CURVE ( 'NONE', #24828, #16797, #25808, .T. ) ;
#30544 = CARTESIAN_POINT ( 'NONE',  ( -30.86621176729672200, 11.58648227300037803, 23.99474104113578221 ) ) ;
#30545 = EDGE_LOOP ( 'NONE', ( #7140, #27212, #30212, #29027 ) ) ;
#30546 = AXIS2_PLACEMENT_3D ( 'NONE', #18218, #15928, #28250 ) ;
#30547 = EDGE_CURVE ( 'NONE', #18622, #21242, #32116, .T. ) ;
#30548 = CIRCLE ( 'NONE', #9051, 0.4000000000000010214 ) ;
#30549 = ORIENTED_EDGE ( 'NONE', *, *, #14682, .T. ) ;
#30550 = EDGE_CURVE ( 'NONE', #4386, #9438, #2593, .T. ) ;
#30551 = AXIS2_PLACEMENT_3D ( 'NONE', #23903, #11755, #4691 ) ;
#30552 = ORIENTED_EDGE ( 'NONE', *, *, #13909, .F. ) ;
#30553 = CARTESIAN_POINT ( 'NONE',  ( -39.67555847965937943, 2.645252416024337361, 48.34930799450052064 ) ) ;
#30554 = DIRECTION ( 'NONE',  ( -1.000000000000000000, 0.000000000000000000, 0.000000000000000000 ) ) ;
#30555 = DIRECTION ( 'NONE',  ( 8.659560562354994488E-17, -0.7071067811865426878, 0.7071067811865524577 ) ) ;
#30556 = ORIENTED_EDGE ( 'NONE', *, *, #6749, .T. ) ;
#30557 = CARTESIAN_POINT ( 'NONE',  ( -42.85109120870324517, 14.58887732880157273, 55.18058063134417779 ) ) ;
#30558 = CARTESIAN_POINT ( 'NONE',  ( 33.46699938050304013, 38.56284415653841791, 47.04930799450051637 ) ) ;
#30559 = CARTESIAN_POINT ( 'NONE',  ( 21.09785597605720042, -13.56320000832927875, 47.04930799450051637 ) ) ;
#30560 = CARTESIAN_POINT ( 'NONE',  ( -40.34207605779958072, 7.502898035225042506, 60.54930799450051637 ) ) ;
#30561 = CARTESIAN_POINT ( 'NONE',  ( -40.06561427811386267, 7.496110634155836117, 53.64930799450051779 ) ) ;
#30562 = CARTESIAN_POINT ( 'NONE',  ( 48.34748475735720064, 24.86874180309281712, 49.49898713858203791 ) ) ;
#30563 = LINE ( 'NONE', #30724, #27390 ) ;
#30564 = DIRECTION ( 'NONE',  ( -1.000000000000000000, 0.000000000000000000, 0.000000000000000000 ) ) ;
#30565 = CARTESIAN_POINT ( 'NONE',  ( 21.09785597605720753, 14.86454579224779948, 47.04930799450052348 ) ) ;
#30566 = AXIS2_PLACEMENT_3D ( 'NONE', #4393, #11625, #1925 ) ;
#30567 = B_SPLINE_SURFACE_WITH_KNOTS ( 'NONE', 3, 3, ( 
 ( #10749, #30764, #20898, #8275, #5818, #15822 ),
 ( #25828, #3342, #13371, #23369, #10900, #30927 ),
 ( #8437, #18430, #14174, #1847, #24167, #1684 ),
 ( #22023, #17100, #14496, #6939, #14333, #26955 ),
 ( #29591, #29428, #9568, #6615, #32054, #24001 ),
 ( #11539, #21531, #31569, #7101, #16937, #9401 ) ),
 .UNSPECIFIED., .F., .F., .F.,
 ( 4, 2, 4 ),
 ( 4, 2, 4 ),
 ( 0.000000000000000000, 0.5000000000000000000, 1.000000000000000000 ),
 ( 0.000000000000000000, 0.5000000000000000000, 1.000000000000000000 ),
 .UNSPECIFIED. ) ;
#30568 = CARTESIAN_POINT ( 'NONE',  ( -39.59300248568538194, 7.744584186742828891, 62.04930799450052348 ) ) ;
#30569 = AXIS2_PLACEMENT_3D ( 'NONE', #6525, #1590, #11613 ) ;
#30570 = CARTESIAN_POINT ( 'NONE',  ( 49.28428300279882990, 28.34787913140504045, 48.46772541801551171 ) ) ;
#30571 = ORIENTED_EDGE ( 'NONE', *, *, #6351, .T. ) ;
#30572 = VERTEX_POINT ( 'NONE', #12788 ) ;
#30573 = CARTESIAN_POINT ( 'NONE',  ( 45.83138912416445265, -13.30632128221581389, 97.21573990761677919 ) ) ;
#30574 = DIRECTION ( 'NONE',  ( -0.2756373558169954441, 0.9612616959383198934, -1.479773560108263204E-16 ) ) ;
#30575 = CARTESIAN_POINT ( 'NONE',  ( 49.40425470046338319, 8.190330151142697801, 97.59131769823768821 ) ) ;
#30576 = EDGE_LOOP ( 'NONE', ( #18539, #1792, #16579, #29407 ) ) ;
#30577 = TOROIDAL_SURFACE ( 'NONE', #4867, 12.40141737965281976, 0.1249999999999999722 ) ;
#30578 = DIRECTION ( 'NONE',  ( 1.000000000000000000, 0.000000000000000000, 0.000000000000000000 ) ) ;
#30579 = CARTESIAN_POINT ( 'NONE',  ( 47.25101359556892078, 23.12036939723557083, 46.81322240026007364 ) ) ;
#30580 = DIRECTION ( 'NONE',  ( -1.000000000000000000, -1.101824276508909764E-16, 0.000000000000000000 ) ) ;
#30581 = AXIS2_PLACEMENT_3D ( 'NONE', #2622, #22642, #12970 ) ;
#30582 = ORIENTED_EDGE ( 'NONE', *, *, #2924, .T. ) ;
#30583 = ORIENTED_EDGE ( 'NONE', *, *, #14643, .F. ) ;
#30584 = DIRECTION ( 'NONE',  ( 0.000000000000000000, 0.000000000000000000, -1.000000000000000000 ) ) ;
#30585 = CARTESIAN_POINT ( 'NONE',  ( 49.49063479933183629, 25.29951373492760069, 47.17357720316391578 ) ) ;
#30586 = CARTESIAN_POINT ( 'NONE',  ( 46.00908685603034343, 28.94624452788248092, 44.91496614357595263 ) ) ;
#30587 = CARTESIAN_POINT ( 'NONE',  ( -39.39994726806853009, -5.935969479811864069, 77.95691600913359309 ) ) ;
#30588 = ADVANCED_FACE ( 'NONE', ( #136 ), #7850, .F. ) ;
#30589 = EDGE_LOOP ( 'NONE', ( #13420, #14027, #6860, #2205 ) ) ;
#30590 = AXIS2_PLACEMENT_3D ( 'NONE', #16502, #21582, #21745 ) ;
#30591 = CIRCLE ( 'NONE', #20105, 1.499999999999999556 ) ;
#30592 = DIRECTION ( 'NONE',  ( -1.101824276508909887E-16, 1.000000000000000000, -0.000000000000000000 ) ) ;
#30593 = CARTESIAN_POINT ( 'NONE',  ( 8.823509210239558698, 29.09164230456639899, 47.04930799450051637 ) ) ;
#30594 = ORIENTED_EDGE ( 'NONE', *, *, #31985, .T. ) ;
#30595 = CIRCLE ( 'NONE', #15403, 54.30000000000000426 ) ;
#30596 = AXIS2_PLACEMENT_3D ( 'NONE', #11082, #23540, #8288 ) ;
#30597 = AXIS2_PLACEMENT_3D ( 'NONE', #3716, #927, #28663 ) ;
#30598 = DIRECTION ( 'NONE',  ( -1.101824276508909887E-16, 1.000000000000000000, -0.000000000000000000 ) ) ;
#30599 = DIRECTION ( 'NONE',  ( -0.000000000000000000, -1.000000000000000000, 0.000000000000000000 ) ) ;
#30600 = ORIENTED_EDGE ( 'NONE', *, *, #2850, .F. ) ;
#30601 = CARTESIAN_POINT ( 'NONE',  ( 9.016997203727585841, 15.24673779880127356, 47.36565641480107303 ) ) ;
#30602 = CARTESIAN_POINT ( 'NONE',  ( 21.09785597605720753, 14.86454579224779948, 47.04930799450052348 ) ) ;
#30603 = CARTESIAN_POINT ( 'NONE',  ( 58.09785597605721108, 13.86454579224779948, 47.04930799450051637 ) ) ;
#30604 = CARTESIAN_POINT ( 'NONE',  ( -5.147605652606496385, 10.07047442526145531, -3.422300758029766854 ) ) ;
#30605 = CARTESIAN_POINT ( 'NONE',  ( -37.68353499307994525, 12.01442086639228712, 60.54930799450051637 ) ) ;
#30606 = VERTEX_POINT ( 'NONE', #20474 ) ;
#30607 = LINE ( 'NONE', #8118, #11844 ) ;
#30608 = DIRECTION ( 'NONE',  ( -0.3958453973320076313, -0.7141240004913228523, 0.5773502691896265082 ) ) ;
#30609 = DIRECTION ( 'NONE',  ( 0.4848096202463424986, 0.8746197071393928546, -2.220446049250312834E-16 ) ) ;
#30610 = DIRECTION ( 'NONE',  ( -1.101824276508909887E-16, 1.000000000000000000, -0.000000000000000000 ) ) ;
#30611 = VECTOR ( 'NONE', #31867, 1000.000000000000000 ) ;
#30612 = AXIS2_PLACEMENT_3D ( 'NONE', #18249, #2998, #3155 ) ;
#30613 = DIRECTION ( 'NONE',  ( -1.000000000000000000, 0.000000000000000000, 0.000000000000000000 ) ) ;
#30614 = EDGE_LOOP ( 'NONE', ( #28157, #15612, #1052, #20106 ) ) ;
#30615 = LINE ( 'NONE', #1934, #18173 ) ;
#30616 = CARTESIAN_POINT ( 'NONE',  ( -40.59298576501943501, 7.024321269945732027, 38.94336021962444505 ) ) ;
#30617 = DIRECTION ( 'NONE',  ( -1.000000000000000000, 0.000000000000000000, 0.000000000000000000 ) ) ;
#30618 = EDGE_LOOP ( 'NONE', ( #28431, #22461, #16727, #26493 ) ) ;
#30619 = FACE_OUTER_BOUND ( 'NONE', #29253, .T. ) ;
#30620 = FACE_OUTER_BOUND ( 'NONE', #30671, .T. ) ;
#30621 = CARTESIAN_POINT ( 'NONE',  ( 21.09785597605720753, 17.36474115922713324, 47.04930799450052348 ) ) ;
#30622 = DIRECTION ( 'NONE',  ( 0.000000000000000000, 0.000000000000000000, -1.000000000000000000 ) ) ;
#30623 = AXIS2_PLACEMENT_3D ( 'NONE', #16181, #16505, #19609 ) ;
#30624 = ORIENTED_EDGE ( 'NONE', *, *, #11522, .F. ) ;
#30625 = LINE ( 'NONE', #8140, #10971 ) ;
#30626 = ORIENTED_EDGE ( 'NONE', *, *, #11437, .F. ) ;
#30627 = ORIENTED_EDGE ( 'NONE', *, *, #9160, .F. ) ;
#30628 = ADVANCED_FACE ( 'NONE', ( #30502 ), #5062, .T. ) ;
#30629 = EDGE_CURVE ( 'NONE', #20299, #19168, #24758, .T. ) ;
#30630 = EDGE_CURVE ( 'NONE', #28214, #10801, #7474, .T. ) ;
#30631 = EDGE_CURVE ( 'NONE', #22618, #29979, #138, .T. ) ;
#30632 = ADVANCED_FACE ( 'NONE', ( #24926, #22771 ), #292, .F. ) ;
#30633 = CARTESIAN_POINT ( 'NONE',  ( 33.37634396954519644, 31.09164230456639544, 47.04930799450051637 ) ) ;
#30634 = DIRECTION ( 'NONE',  ( 0.5319835227803570987, 0.2110602665713104953, -0.8200287161831886218 ) ) ;
#30635 = FACE_OUTER_BOUND ( 'NONE', #22948, .T. ) ;
#30636 = TOROIDAL_SURFACE ( 'NONE', #14919, 4.099999999999999645, 0.1000000000000002554 ) ;
#30637 = VERTEX_POINT ( 'NONE', #30179 ) ;
#30638 = CARTESIAN_POINT ( 'NONE',  ( -34.42886191242200056, 11.85135941024610418, 40.60668834306612496 ) ) ;
#30639 = ORIENTED_EDGE ( 'NONE', *, *, #26266, .T. ) ;
#30640 = CIRCLE ( 'NONE', #16471, 0.1250000000000001110 ) ;
#30641 = DIRECTION ( 'NONE',  ( -1.101824276508909887E-16, 1.000000000000000000, -0.000000000000000000 ) ) ;
#30642 = FACE_OUTER_BOUND ( 'NONE', #17523, .T. ) ;
#30643 = CARTESIAN_POINT ( 'NONE',  ( 33.72499318558949000, 38.56284415653841791, 47.04930799450051637 ) ) ;
#30644 = CARTESIAN_POINT ( 'NONE',  ( 33.46699938050303302, 38.56284415653841791, 47.04930799450051637 ) ) ;
#30645 = ORIENTED_EDGE ( 'NONE', *, *, #7821, .T. ) ;
#30646 = DIRECTION ( 'NONE',  ( -1.000000000000000000, -1.101824276508909887E-16, 0.000000000000000000 ) ) ;
#30647 = ORIENTED_EDGE ( 'NONE', *, *, #20665, .T. ) ;
#30648 = CARTESIAN_POINT ( 'NONE',  ( -42.28301147118430237, 15.25948642862022986, 35.64930799450052490 ) ) ;
#30649 = PLANE ( 'NONE',  #10595 ) ;
#30650 = EDGE_LOOP ( 'NONE', ( #2270, #15736, #17972, #14774 ) ) ;
#30651 = CARTESIAN_POINT ( 'NONE',  ( 47.71045395478045492, 23.04411619146718238, 46.10501571378621577 ) ) ;
#30652 = CARTESIAN_POINT ( 'NONE',  ( 81.72311593397060392, -5.936969727347467085, 16.00772641743157720 ) ) ;
#30653 = CARTESIAN_POINT ( 'NONE',  ( 8.698509210239569356, 30.09164230456639544, 47.04930799450051637 ) ) ;
#30654 = FILL_AREA_STYLE_COLOUR ( '', #6314 ) ;
#30655 = CYLINDRICAL_SURFACE ( 'NONE', #21520, 12.62506659569710266 ) ;
#30656 = CARTESIAN_POINT ( 'NONE',  ( -40.70323106273447422, 6.774493230553032319, 34.57503839362117759 ) ) ;
#30657 = ORIENTED_EDGE ( 'NONE', *, *, #23389, .T. ) ;
#30659 = EDGE_CURVE ( 'NONE', #15925, #4643, #31065, .T. ) ;
#30658 = DIRECTION ( 'NONE',  ( -0.000000000000000000, -1.000000000000000000, -0.000000000000000000 ) ) ;
#30660 = ADVANCED_FACE ( 'NONE', ( #3391 ), #8797, .T. ) ;
#30661 = FACE_BOUND ( 'NONE', #6069, .T. ) ;
#30662 = ORIENTED_EDGE ( 'NONE', *, *, #10231, .F. ) ;
#30663 = AXIS2_PLACEMENT_3D ( 'NONE', #27270, #14810, #24971 ) ;
#30664 = EDGE_LOOP ( 'NONE', ( #20285, #32077, #11438, #27884 ) ) ;
#30665 = CARTESIAN_POINT ( 'NONE',  ( -42.33363892739273382, 14.73725438281773847, 55.13459228725880479 ) ) ;
#30666 = CIRCLE ( 'NONE', #23295, 0.1250000000000001110 ) ;
#30667 = AXIS2_PLACEMENT_3D ( 'NONE', #1596, #19477, #32129 ) ;
#30668 = AXIS2_PLACEMENT_3D ( 'NONE', #18629, #18149, #18308 ) ;
#30669 = ORIENTED_EDGE ( 'NONE', *, *, #22438, .F. ) ;
#30670 = ADVANCED_FACE ( 'NONE', ( #11276 ), #30577, .T. ) ;
#30671 = EDGE_LOOP ( 'NONE', ( #28522, #20370, #27322, #26965 ) ) ;
#30672 = DIRECTION ( 'NONE',  ( 0.000000000000000000, 0.000000000000000000, -1.000000000000000000 ) ) ;
#30673 = ORIENTED_EDGE ( 'NONE', *, *, #32319, .F. ) ;
#30674 = VECTOR ( 'NONE', #2774, 1000.000000000000000 ) ;
#30675 = CARTESIAN_POINT ( 'NONE',  ( 21.09992658989239089, 26.46183152705960140, 47.04930799450051637 ) ) ;
#30676 = CARTESIAN_POINT ( 'NONE',  ( 49.49821893081623614, 29.23298080189710291, 46.63169638315567767 ) ) ;
#30677 = DIRECTION ( 'NONE',  ( -1.101824276508909887E-16, 1.000000000000000000, -0.000000000000000000 ) ) ;
#30678 = ADVANCED_FACE ( 'NONE', ( #3880 ), #20577, .F. ) ;
#30679 = AXIS2_PLACEMENT_3D ( 'NONE', #3294, #20536, #8235 ) ;
#30680 = CARTESIAN_POINT ( 'NONE',  ( 45.81741271322955100, 25.70122849631043849, 49.02305402274571122 ) ) ;
#30681 = ORIENTED_EDGE ( 'NONE', *, *, #10774, .T. ) ;
#30682 = ORIENTED_EDGE ( 'NONE', *, *, #28088, .T. ) ;
#30684 = CARTESIAN_POINT ( 'NONE',  ( 21.09785597605720753, 14.86454579224779948, 47.04930799450052348 ) ) ;
#30683 = AXIS2_PLACEMENT_3D ( 'NONE', #28975, #4676, #9276 ) ;
#30685 = VECTOR ( 'NONE', #29791, 1000.000000000000000 ) ;
#30686 = ORIENTED_EDGE ( 'NONE', *, *, #27282, .T. ) ;
#30687 = ADVANCED_FACE ( 'NONE', ( #26038 ), #20313, .F. ) ;
#30688 = DIRECTION ( 'NONE',  ( -0.000000000000000000, -1.000000000000000000, -0.000000000000000000 ) ) ;
#30689 = AXIS2_PLACEMENT_3D ( 'NONE', #8579, #30751, #13672 ) ;
#30690 = CARTESIAN_POINT ( 'NONE',  ( 21.09785597605720753, 15.57592086119046826, 47.04930799450052348 ) ) ;
#30691 = FACE_OUTER_BOUND ( 'NONE', #19633, .T. ) ;
#30692 = DIRECTION ( 'NONE',  ( 8.659560562355053653E-17, -0.7071067811865378028, 0.7071067811865573427 ) ) ;
#30693 = DIRECTION ( 'NONE',  ( 0.2756373558170105986, -0.9612616959383156745, 0.000000000000000000 ) ) ;
#30694 = ORIENTED_EDGE ( 'NONE', *, *, #29128, .T. ) ;
#30695 = DIRECTION ( 'NONE',  ( -0.000000000000000000, -1.000000000000000000, 0.000000000000000000 ) ) ;
#30696 = EDGE_CURVE ( 'NONE', #12851, #4827, #5403, .T. ) ;
#30697 = DIRECTION ( 'NONE',  ( -1.224646799147353207E-16, -1.349345573449484691E-32, 1.000000000000000000 ) ) ;
#30698 = EDGE_CURVE ( 'NONE', #14884, #22418, #20796, .T. ) ;
#30699 = CYLINDRICAL_SURFACE ( 'NONE', #29849, 54.29999999999999716 ) ;
#30700 = CARTESIAN_POINT ( 'NONE',  ( 49.49063479933183629, 25.29951373492760069, 47.17357720316391578 ) ) ;
#30701 = EDGE_LOOP ( 'NONE', ( #16503, #25233, #24856 ) ) ;
#30702 = DIRECTION ( 'NONE',  ( -1.101824276508909887E-16, 1.000000000000000000, -0.000000000000000000 ) ) ;
#30703 = CARTESIAN_POINT ( 'NONE',  ( -40.50726676868416121, 7.559560304694834088, 53.83429597860652649 ) ) ;
#30704 = ORIENTED_EDGE ( 'NONE', *, *, #28137, .T. ) ;
#30705 = TOROIDAL_SURFACE ( 'NONE', #5026, 12.61792373059894246, 0.1249999999999989730 ) ;
#30706 = EDGE_CURVE ( 'NONE', #29823, #1311, #12204, .T. ) ;
#30707 = TOROIDAL_SURFACE ( 'NONE', #17076, 12.40141737965280200, 0.1249999999999999445 ) ;
#30708 = AXIS2_PLACEMENT_3D ( 'NONE', #20891, #30919, #11530 ) ;
#30709 = EDGE_LOOP ( 'NONE', ( #4078, #14849, #21748 ) ) ;
#30710 = ORIENTED_EDGE ( 'NONE', *, *, #16661, .T. ) ;
#30711 = CARTESIAN_POINT ( 'NONE',  ( 48.83059987400640978, 25.58213139976340855, 48.97189179988551899 ) ) ;
#30712 = DIRECTION ( 'NONE',  ( -0.000000000000000000, 1.000000000000000000, -0.000000000000000000 ) ) ;
#30713 = CARTESIAN_POINT ( 'NONE',  ( -40.05987053574653345, 7.506472619680472746, 39.54930799450052348 ) ) ;
#30714 = AXIS2_PLACEMENT_3D ( 'NONE', #28244, #30712, #28086 ) ;
#30715 = VERTEX_POINT ( 'NONE', #28833 ) ;
#30716 = CARTESIAN_POINT ( 'NONE',  ( -34.71499704722535284, -13.30632128221581212, 43.39636530629570643 ) ) ;
#30717 = DIRECTION ( 'NONE',  ( 0.000000000000000000, -1.000000000000000000, -0.000000000000000000 ) ) ;
#30718 = FACE_BOUND ( 'NONE', #11157, .T. ) ;
#30719 = EDGE_CURVE ( 'NONE', #29624, #23397, #10960, .T. ) ;
#30720 = DIRECTION ( 'NONE',  ( -1.000000000000000000, 0.000000000000000000, 0.000000000000000000 ) ) ;
#30721 = EDGE_CURVE ( 'NONE', #4851, #10602, #10646, .T. ) ;
#30722 = CARTESIAN_POINT ( 'NONE',  ( 21.09992658989238734, 31.84164230456639544, 47.04930799450051637 ) ) ;
#30723 = CARTESIAN_POINT ( 'NONE',  ( 8.732853799281738105, 24.96183152705960140, 47.04930799450051637 ) ) ;
#30724 = CARTESIAN_POINT ( 'NONE',  ( -40.14651252454546437, 6.746025643617127088, 39.54930799450052348 ) ) ;
#30725 = DIRECTION ( 'NONE',  ( -1.101824276508909887E-16, 1.000000000000000000, -0.000000000000000000 ) ) ;
#30726 = DIRECTION ( 'NONE',  ( -0.000000000000000000, -1.000000000000000000, 0.000000000000000000 ) ) ;
#30727 = CARTESIAN_POINT ( 'NONE',  ( 36.33160203359362583, 14.46497581658974063, 47.04930799450052348 ) ) ;
#30728 = CARTESIAN_POINT ( 'NONE',  ( 44.91142894931555674, 29.39787913140503761, 45.63089057098605394 ) ) ;
#30729 = SURFACE_STYLE_USAGE ( .BOTH. , #20702 ) ;
#30730 = ORIENTED_EDGE ( 'NONE', *, *, #8062, .F. ) ;
#30731 = ORIENTED_EDGE ( 'NONE', *, *, #30630, .T. ) ;
#30732 = CARTESIAN_POINT ( 'NONE',  ( 21.09785597605720753, -5.098646251524523443, 47.04930799450052348 ) ) ;
#30733 = CIRCLE ( 'NONE', #29152, 66.44011198581388555 ) ;
#30734 = AXIS2_PLACEMENT_3D ( 'NONE', #11668, #4277, #9035 ) ;
#30735 = DIRECTION ( 'NONE',  ( 0.000000000000000000, 1.000000000000000000, -0.000000000000000000 ) ) ;
#30736 = EDGE_CURVE ( 'NONE', #19811, #23803, #25731, .T. ) ;
#30737 = EDGE_CURVE ( 'NONE', #30980, #5512, #31300, .T. ) ;
#30738 = CARTESIAN_POINT ( 'NONE',  ( 54.69690332803826749, -1.331120222581874346, 100.5855669984461258 ) ) ;
#30739 = VERTEX_POINT ( 'NONE', #28667 ) ;
#30740 = DIRECTION ( 'NONE',  ( -1.101824276508909887E-16, 1.000000000000000000, -0.000000000000000000 ) ) ;
#30741 = CARTESIAN_POINT ( 'NONE',  ( -40.13646513110854386, 7.213257191581853078, 38.95955396713193863 ) ) ;
#30742 = ORIENTED_EDGE ( 'NONE', *, *, #31538, .F. ) ;
#30743 = LINE ( 'NONE', #7767, #17296 ) ;
#30744 = CARTESIAN_POINT ( 'NONE',  ( 45.24946171279598417, 26.40784706826093498, 47.99220971130007030 ) ) ;
#30745 = CARTESIAN_POINT ( 'NONE',  ( 48.94625023931840246, 29.47124452788248306, 46.10640627770150246 ) ) ;
#30746 = TOROIDAL_SURFACE ( 'NONE', #10314, 12.61792373059898154, 0.1249999999999967248 ) ;
#30747 = CARTESIAN_POINT ( 'NONE',  ( -34.95779894681891165, 11.10722333531405148, 52.41483564559372610 ) ) ;
#30748 = ORIENTED_EDGE ( 'NONE', *, *, #8974, .F. ) ;
#30749 = DIRECTION ( 'NONE',  ( 0.8746197071393925215, -0.4848096202463429982, -8.676864087101708112E-18 ) ) ;
#30750 = CIRCLE ( 'NONE', #2443, 1.499999999999997780 ) ;
#30751 = DIRECTION ( 'NONE',  ( 0.000000000000000000, 1.000000000000000000, 0.000000000000000000 ) ) ;
#30752 = CARTESIAN_POINT ( 'NONE',  ( 21.09992658989239089, 23.71664230456639899, 47.04930799450051637 ) ) ;
#30753 = VERTEX_POINT ( 'NONE', #6180 ) ;
#30754 = SPHERICAL_SURFACE ( 'NONE', #22962, 0.1000000000000000056 ) ;
#30755 = EDGE_CURVE ( 'NONE', #23707, #30037, #9053, .T. ) ;
#30756 = CYLINDRICAL_SURFACE ( 'NONE', #29887, 12.36707279061065279 ) ;
#30757 = AXIS2_PLACEMENT_3D ( 'NONE', #19520, #27408, #14936 ) ;
#30758 = ORIENTED_EDGE ( 'NONE', *, *, #27349, .F. ) ;
#30759 = DIRECTION ( 'NONE',  ( 1.000000000000000000, 0.000000000000000000, 0.000000000000000000 ) ) ;
#30760 = DIRECTION ( 'NONE',  ( -0.8746197071393810862, 0.4848096202463637039, 8.676864087101942305E-18 ) ) ;
#30761 = CARTESIAN_POINT ( 'NONE',  ( 21.09785597605719332, -9.935454207752199451, -20.95069200549946231 ) ) ;
#30762 = DIRECTION ( 'NONE',  ( -1.101824276508909887E-16, 1.000000000000000000, -0.000000000000000000 ) ) ;
#30763 = ORIENTED_EDGE ( 'NONE', *, *, #20157, .T. ) ;
#30764 = CARTESIAN_POINT ( 'NONE',  ( 46.96997866373305186, 23.12036939723557083, 46.79862680810013131 ) ) ;
#30765 = CARTESIAN_POINT ( 'NONE',  ( -42.38263560350583248, 14.61917486843862868, 60.54930799450051637 ) ) ;
#30766 = DIRECTION ( 'NONE',  ( 0.2756373558169947779, -0.9612616959383200044, 0.000000000000000000 ) ) ;
#30767 = ADVANCED_FACE ( 'NONE', ( #18797, #30661 ), #16187, .T. ) ;
#30768 = LINE ( 'NONE', #25355, #13162 ) ;
#30769 = ORIENTED_EDGE ( 'NONE', *, *, #11600, .T. ) ;
#30770 = FACE_OUTER_BOUND ( 'NONE', #15569, .T. ) ;
#30771 = CARTESIAN_POINT ( 'NONE',  ( 49.71806030971111312, 24.89927402503721154, 46.59246371035801815 ) ) ;
#30772 = CARTESIAN_POINT ( 'NONE',  ( 33.37634396954527460, 24.09164230456639544, 47.04930799450051637 ) ) ;
#30773 = ORIENTED_EDGE ( 'NONE', *, *, #14449, .T. ) ;
#30774 = DIRECTION ( 'NONE',  ( -1.000000000000000000, 0.000000000000000000, 0.000000000000000000 ) ) ;
#30775 = DIRECTION ( 'NONE',  ( 0.7848668881104262640, 0.2250569586005336520, 0.5773502691896258421 ) ) ;
#30776 = AXIS2_PLACEMENT_3D ( 'NONE', #32228, #14179, #24496 ) ;
#30777 = CARTESIAN_POINT ( 'NONE',  ( 58.59785597605721108, -5.098646251524523443, 47.04930799450051637 ) ) ;
#30778 = CARTESIAN_POINT ( 'NONE',  ( 21.09992658989239089, 26.09143805560860940, 47.04930799450051637 ) ) ;
#30779 = EDGE_LOOP ( 'NONE', ( #31125, #1473, #5153, #17008, #2409, #973 ) ) ;
#30780 = DIRECTION ( 'NONE',  ( 0.000000000000000000, 0.000000000000000000, 1.000000000000000000 ) ) ;
#30781 = VERTEX_POINT ( 'NONE', #5879 ) ;
#30782 = AXIS2_PLACEMENT_3D ( 'NONE', #4187, #6166, #24369 ) ;
#30783 = ORIENTED_EDGE ( 'NONE', *, *, #25664, .T. ) ;
#30784 = DIRECTION ( 'NONE',  ( -1.101824276508909887E-16, 1.000000000000000000, -0.000000000000000000 ) ) ;
#30785 = DIRECTION ( 'NONE',  ( 1.234978253042719660E-16, -1.000000000000000000, -1.109335647967047851E-31 ) ) ;
#30786 = CARTESIAN_POINT ( 'NONE',  ( 81.46980107077142463, -5.935340315990521809, 15.93528473569102566 ) ) ;
#30787 = CIRCLE ( 'NONE', #392, 0.1250000000000001110 ) ;
#30788 = ORIENTED_EDGE ( 'NONE', *, *, #32245, .F. ) ;
#30789 = CARTESIAN_POINT ( 'NONE',  ( 8.698509210239523171, 25.84164230456639899, 47.04930799450051637 ) ) ;
#30790 = EDGE_LOOP ( 'NONE', ( #16093, #27234, #7706, #27454 ) ) ;
#30791 = DIRECTION ( 'NONE',  ( -0.000000000000000000, 1.000000000000000000, -0.000000000000000000 ) ) ;
#30792 = PLANE ( 'NONE',  #15438 ) ;
#30793 = LINE ( 'NONE', #7994, #15846 ) ;
#30794 = AXIS2_PLACEMENT_3D ( 'NONE', #28147, #5651, #8123 ) ;
#30795 = DIRECTION ( 'NONE',  ( 0.4848096202463673676, 0.8746197071393789768, 0.000000000000000000 ) ) ;
#30796 = ORIENTED_EDGE ( 'NONE', *, *, #28710, .F. ) ;
#30797 = DIRECTION ( 'NONE',  ( -1.000000000000000000, 0.000000000000000000, -1.110223024625155594E-14 ) ) ;
#30798 = ORIENTED_EDGE ( 'NONE', *, *, #11046, .F. ) ;
#30799 = FACE_OUTER_BOUND ( 'NONE', #13250, .T. ) ;
#30800 = DIRECTION ( 'NONE',  ( -1.000000000000000000, 0.000000000000000000, 0.000000000000000000 ) ) ;
#30801 = ORIENTED_EDGE ( 'NONE', *, *, #18846, .T. ) ;
#30802 = FACE_OUTER_BOUND ( 'NONE', #17385, .T. ) ;
#30803 = ADVANCED_FACE ( 'NONE', ( #25887 ), #930, .T. ) ;
#30804 = CARTESIAN_POINT ( 'NONE',  ( -35.16155806787664062, 11.92558985988975806, 53.76629232714613238 ) ) ;
#30805 = CARTESIAN_POINT ( 'NONE',  ( 46.17891025898683921, 22.93807716476589675, 48.46582155994513386 ) ) ;
#30806 = DIRECTION ( 'NONE',  ( -0.000000000000000000, 1.000000000000000000, -0.000000000000000000 ) ) ;
#30807 = EDGE_CURVE ( 'NONE', #2021, #27386, #13789, .T. ) ;
#30808 = EDGE_CURVE ( 'NONE', #23798, #7845, #26686, .T. ) ;
#30809 = DIRECTION ( 'NONE',  ( -1.000000000000000000, 0.000000000000000000, 0.000000000000000000 ) ) ;
#30810 = EDGE_CURVE ( 'NONE', #9948, #21573, #27400, .T. ) ;
#30811 = VERTEX_POINT ( 'NONE', #31777 ) ;
#30812 = CARTESIAN_POINT ( 'NONE',  ( 44.87087493598345134, 28.75322093266651891, 48.18533415931919706 ) ) ;
#30813 = CARTESIAN_POINT ( 'NONE',  ( 1.597855976057205973, -5.098646251524523443, 47.04930799450052348 ) ) ;
#30814 = ADVANCED_FACE ( 'NONE', ( #4039 ), #2063, .F. ) ;
#30815 = EDGE_CURVE ( 'NONE', #12709, #25906, #14831, .T. ) ;
#30816 = ORIENTED_EDGE ( 'NONE', *, *, #18558, .T. ) ;
#30817 = DIRECTION ( 'NONE',  ( -1.000000000000000000, 0.000000000000000000, 0.000000000000000000 ) ) ;
#30818 = DIRECTION ( 'NONE',  ( 1.000000000000000000, 0.000000000000000000, -1.224646799147353207E-16 ) ) ;
#30819 = ORIENTED_EDGE ( 'NONE', *, *, #30221, .F. ) ;
#30820 = ORIENTED_EDGE ( 'NONE', *, *, #5538, .F. ) ;
#30821 = CARTESIAN_POINT ( 'NONE',  ( -11.98523041842830850, -4.708525186292168208, 104.0193796289731409 ) ) ;
#30822 = UNCERTAINTY_MEASURE_WITH_UNIT (LENGTH_MEASURE( 1.000000000000000082E-05 ), #10061, 'distance_accuracy_value', 'NONE');
#30823 = CIRCLE ( 'NONE', #8772, 0.1000000000000008243 ) ;
#30824 = VERTEX_POINT ( 'NONE', #6831 ) ;
#30825 = ADVANCED_BREP_SHAPE_REPRESENTATION ( '', ( #23129, #8172 ), #22330 ) ;
#30826 = CIRCLE ( 'NONE', #4077, 25.50000000000000355 ) ;
#30827 = ADVANCED_FACE ( 'NONE', ( #17147 ), #4206, .F. ) ;
#30828 = VECTOR ( 'NONE', #7953, 1000.000000000000000 ) ;
#30829 = ORIENTED_EDGE ( 'NONE', *, *, #9543, .T. ) ;
#30830 = CARTESIAN_POINT ( 'NONE',  ( 8.823509210239514289, 24.84164230456639544, 47.04930799450051637 ) ) ;
#30831 = ADVANCED_FACE ( 'NONE', ( #14383 ), #25323, .T. ) ;
#30832 = ORIENTED_EDGE ( 'NONE', *, *, #26795, .T. ) ;
#30833 = CARTESIAN_POINT ( 'NONE',  ( 48.58040715586306391, 22.89977464660286444, 48.17922887912574481 ) ) ;
#30834 = CARTESIAN_POINT ( 'NONE',  ( -40.73091736380679606, 9.483895492497154578, 34.64930799450051779 ) ) ;
#30835 = DIRECTION ( 'NONE',  ( -1.101824276508909887E-16, 1.000000000000000000, -0.000000000000000000 ) ) ;
#30836 = CARTESIAN_POINT ( 'NONE',  ( 48.37829923888483563, 26.75122849631043209, 45.07556196625585443 ) ) ;
#30837 = ORIENTED_EDGE ( 'NONE', *, *, #25760, .T. ) ;
#30838 = TOROIDAL_SURFACE ( 'NONE', #6200, 12.40141737965286062, 0.1249999999999998196 ) ;
#30839 = ORIENTED_EDGE ( 'NONE', *, *, #18376, .F. ) ;
#30840 = DIRECTION ( 'NONE',  ( -1.000000000000000000, 0.000000000000000000, 0.000000000000000000 ) ) ;
#30841 = AXIS2_PLACEMENT_3D ( 'NONE', #3891, #19297, #11286 ) ;
#30842 = ORIENTED_EDGE ( 'NONE', *, *, #30218, .F. ) ;
#30843 = CARTESIAN_POINT ( 'NONE',  ( 21.09785597605720042, -14.04221034894631615, 47.04930799450051637 ) ) ;
#30844 = DIRECTION ( 'NONE',  ( -1.000000000000000000, 0.000000000000000000, 0.000000000000000000 ) ) ;
#30845 = CARTESIAN_POINT ( 'NONE',  ( 48.79601671567883159, 22.86454579224779948, 48.10649398831456125 ) ) ;
#30846 = EDGE_CURVE ( 'NONE', #1803, #9995, #16916, .T. ) ;
#30847 = VECTOR ( 'NONE', #27009, 1000.000000000000000 ) ;
#30848 = DIRECTION ( 'NONE',  ( -1.000000000000000000, 0.000000000000000000, 0.000000000000000000 ) ) ;
#30849 = DIRECTION ( 'NONE',  ( -1.000000000000000000, 0.000000000000000000, 0.000000000000000000 ) ) ;
#30850 = EDGE_CURVE ( 'NONE', #12604, #23684, #14226, .T. ) ;
#30851 = VERTEX_POINT ( 'NONE', #21420 ) ;
#30852 = DIRECTION ( 'NONE',  ( -1.101824276508909887E-16, 1.000000000000000000, -0.000000000000000000 ) ) ;
#30853 = DIRECTION ( 'NONE',  ( 0.000000000000000000, 0.000000000000000000, -1.000000000000000000 ) ) ;
#30854 = CIRCLE ( 'NONE', #11435, 12.27641737965288904 ) ;
#30855 = CARTESIAN_POINT ( 'NONE',  ( 38.59785597605721108, 14.86454579224779948, 47.04930799450052348 ) ) ;
#30856 = CARTESIAN_POINT ( 'NONE',  ( 48.40186567930497574, 26.81618040159426641, 45.03923535223907493 ) ) ;
#30857 = VERTEX_POINT ( 'NONE', #19612 ) ;
#30858 = DIRECTION ( 'NONE',  ( 0.4544104193609905806, 5.611869858668448142E-17, 0.8907924397839087627 ) ) ;
#30859 = CARTESIAN_POINT ( 'NONE',  ( -40.70508238852949745, 9.491303552449114278, 35.44930799450052206 ) ) ;
#30860 = EDGE_LOOP ( 'NONE', ( #20335, #5428, #6394, #12857 ) ) ;
#30861 = CIRCLE ( 'NONE', #29814, 0.2000000000000022593 ) ;
#30862 = ADVANCED_FACE ( 'NONE', ( #1413 ), #21623, .T. ) ;
#30863 = AXIS2_PLACEMENT_3D ( 'NONE', #31186, #1455, #10998 ) ;
#30864 = ORIENTED_EDGE ( 'NONE', *, *, #3195, .F. ) ;
#30865 = VECTOR ( 'NONE', #27740, 1000.000000000000227 ) ;
#30866 = ORIENTED_EDGE ( 'NONE', *, *, #4758, .T. ) ;
#30867 = FACE_OUTER_BOUND ( 'NONE', #3830, .T. ) ;
#30868 = EDGE_CURVE ( 'NONE', #30342, #17679, #7497, .T. ) ;
#30869 = CARTESIAN_POINT ( 'NONE',  ( 21.09785597605720753, -5.098646251524523443, 47.04930799450052348 ) ) ;
#30870 = CARTESIAN_POINT ( 'NONE',  ( 21.09992658989239089, 29.97145308207317527, 47.04930799450051637 ) ) ;
#30871 = EDGE_CURVE ( 'NONE', #17692, #5687, #1571, .T. ) ;
#30872 = VECTOR ( 'NONE', #26112, 1000.000000000000114 ) ;
#30873 = ORIENTED_EDGE ( 'NONE', *, *, #2214, .F. ) ;
#30874 = CARTESIAN_POINT ( 'NONE',  ( -23.27936906821728869, -13.30632128221581212, 13.00403739414156590 ) ) ;
#30875 = DIRECTION ( 'NONE',  ( -0.2756373558169974980, 0.9612616959383194493, 1.315048337272770743E-17 ) ) ;
#30876 = DIRECTION ( 'NONE',  ( -1.000000000000000000, 0.000000000000000000, 0.000000000000000000 ) ) ;
#30877 = ORIENTED_EDGE ( 'NONE', *, *, #16642, .F. ) ;
#30878 = CARTESIAN_POINT ( 'NONE',  ( -43.72819403793993587, 1.315833819094414769, 39.54930799450052348 ) ) ;
#30879 = ORIENTED_EDGE ( 'NONE', *, *, #26696, .F. ) ;
#30880 = FACE_OUTER_BOUND ( 'NONE', #10628, .T. ) ;
#30881 = CARTESIAN_POINT ( 'NONE',  ( 36.38461588890405096, 14.98269195386757602, 47.04930799450052348 ) ) ;
#30882 = DIRECTION ( 'NONE',  ( -1.000000000000000000, 0.000000000000000000, 0.000000000000000000 ) ) ;
#30883 = DIRECTION ( 'NONE',  ( -0.4848096202463429427, -0.8746197071393925215, 4.053240046925389072E-19 ) ) ;
#30884 = CARTESIAN_POINT ( 'NONE',  ( -40.64500813507293486, 6.819128862114091305, 34.57932936825760351 ) ) ;
#30885 = DIRECTION ( 'NONE',  ( 0.000000000000000000, 0.000000000000000000, 1.000000000000000000 ) ) ;
#30886 = EDGE_CURVE ( 'NONE', #14337, #29823, #27011, .T. ) ;
#30887 = EDGE_LOOP ( 'NONE', ( #22402, #5924, #4313, #18321 ) ) ;
#30888 = VERTEX_POINT ( 'NONE', #31941 ) ;
#30889 = CYLINDRICAL_SURFACE ( 'NONE', #28633, 0.1000000000000008243 ) ;
#30890 = CIRCLE ( 'NONE', #14109, 12.62506659569710266 ) ;
#30891 = DIRECTION ( 'NONE',  ( -1.000000000000000000, 0.000000000000000000, 0.000000000000000000 ) ) ;
#30892 = AXIS2_PLACEMENT_3D ( 'NONE', #12751, #20914, #18132 ) ;
#30893 = CARTESIAN_POINT ( 'NONE',  ( 21.09992658989239089, 25.96183152705960140, 47.04930799450051637 ) ) ;
#30894 = ORIENTED_EDGE ( 'NONE', *, *, #6446, .T. ) ;
#30895 = FACE_BOUND ( 'NONE', #24285, .T. ) ;
#30896 = VERTEX_POINT ( 'NONE', #14544 ) ;
#30897 = DIRECTION ( 'NONE',  ( -1.101824276508909887E-16, 1.000000000000000000, -0.000000000000000000 ) ) ;
#30898 = CARTESIAN_POINT ( 'NONE',  ( 47.23302798462060537, 29.98121246473836976, 44.44659793406428605 ) ) ;
#30899 = VECTOR ( 'NONE', #10026, 1000.000000000000000 ) ;
#30900 = LINE ( 'NONE', #15629, #2819 ) ;
#30901 = VECTOR ( 'NONE', #5429, 1000.000000000000000 ) ;
#30902 = EDGE_CURVE ( 'NONE', #28880, #14836, #21753, .T. ) ;
#30903 = EDGE_CURVE ( 'NONE', #25423, #20369, #11686, .T. ) ;
#30904 = ORIENTED_EDGE ( 'NONE', *, *, #10015, .T. ) ;
#30905 = B_SPLINE_CURVE_WITH_KNOTS ( 'NONE', 3,
 ( #31414, #21867, #8917, #16303, #11382, #21706, #19236, #31737 ),
 .UNSPECIFIED., .F., .F.,
 ( 4, 2, 2, 4 ),
 ( 0.0005577589035164437319, 0.001153159837334056647, 0.001748560771151669779, 0.002939362638786875877 ),
 .UNSPECIFIED. ) ;
#30906 = APPLICATION_CONTEXT ( 'automotive_design' ) ;
#30907 = CARTESIAN_POINT ( 'NONE',  ( 48.14727188781975542, 22.80400562401890241, 49.10650501410607660 ) ) ;
#30908 = AXIS2_PLACEMENT_3D ( 'NONE', #24397, #31791, #1425 ) ;
#30909 = EDGE_CURVE ( 'NONE', #24538, #27344, #2773, .T. ) ;
#30910 = AXIS2_PLACEMENT_3D ( 'NONE', #29114, #28628, #21543 ) ;
#30911 = ORIENTED_EDGE ( 'NONE', *, *, #18885, .T. ) ;
#30912 = ADVANCED_FACE ( 'NONE', ( #7153 ), #27832, .F. ) ;
#30913 = FACE_OUTER_BOUND ( 'NONE', #8792, .T. ) ;
#30914 = CARTESIAN_POINT ( 'NONE',  ( 44.79156314060809763, 22.80400562401889530, 46.92953032342012420 ) ) ;
#30915 = CARTESIAN_POINT ( 'NONE',  ( 21.09785597605720753, -14.24176827912842391, 105.8992094215394388 ) ) ;
#30916 = AXIS2_PLACEMENT_3D ( 'NONE', #32063, #21374, #4323 ) ;
#30917 = ORIENTED_EDGE ( 'NONE', *, *, #21431, .T. ) ;
#30918 = CIRCLE ( 'NONE', #31429, 12.27641737965279845 ) ;
#30919 = DIRECTION ( 'NONE',  ( 1.188208965918164993E-16, 1.880121038077812639E-16, 1.000000000000000000 ) ) ;
#30920 = DIRECTION ( 'NONE',  ( 0.000000000000000000, 0.000000000000000000, -1.000000000000000000 ) ) ;
#30921 = CARTESIAN_POINT ( 'NONE',  ( 21.09785597605720042, -16.93545420775220123, 47.04930799450051637 ) ) ;
#30922 = AXIS2_PLACEMENT_3D ( 'NONE', #7035, #26567, #1941 ) ;
#30923 = CARTESIAN_POINT ( 'NONE',  ( -4.653529917572326369, 10.40182650318958579, 98.46608932373301570 ) ) ;
#30924 =( LENGTH_UNIT ( ) NAMED_UNIT ( * ) SI_UNIT ( .MILLI., .METRE. ) );
#30925 = VERTEX_POINT ( 'NONE', #20108 ) ;
#30926 = VECTOR ( 'NONE', #18598, 1000.000000000000000 ) ;
#30927 = CARTESIAN_POINT ( 'NONE',  ( 46.18657129672061501, 22.93807716476589675, 45.61868866909985343 ) ) ;
#30928 = CARTESIAN_POINT ( 'NONE',  ( 8.474859994195282908, 38.56284415653841791, 47.04930799450051637 ) ) ;
#30929 = CARTESIAN_POINT ( 'NONE',  ( -40.10917099319649282, 6.845611892227013051, 34.60381041995846374 ) ) ;
#30930 = CARTESIAN_POINT ( 'NONE',  ( -4.902144023942810236, 30.56554579224779644, 47.04930799450042400 ) ) ;
#30931 = VERTEX_POINT ( 'NONE', #5182 ) ;
#30932 = DIRECTION ( 'NONE',  ( -0.000000000000000000, -1.000000000000000000, 0.000000000000000000 ) ) ;
#30933 = CARTESIAN_POINT ( 'NONE',  ( 49.65144901789264509, 24.93175518340850161, 46.50564549375109635 ) ) ;
#30934 = DIRECTION ( 'NONE',  ( -1.101824276508909887E-16, 1.000000000000000000, -0.000000000000000000 ) ) ;
#30935 = ORIENTED_EDGE ( 'NONE', *, *, #26572, .T. ) ;
#30936 = CARTESIAN_POINT ( 'NONE',  ( 49.51946345327874610, 19.86454579224779948, 47.17507454913548770 ) ) ;
#30937 = CARTESIAN_POINT ( 'NONE',  ( -41.50386623137114839, 10.69791363055605515, 57.28220823191252720 ) ) ;
#30938 = AXIS2_PLACEMENT_3D ( 'NONE', #15174, #12397, #32256 ) ;
#30939 = TOROIDAL_SURFACE ( 'NONE', #4191, 12.40141737965284641, 0.1249999999999995698 ) ;
#30940 = DIRECTION ( 'NONE',  ( 0.000000000000000000, 0.000000000000000000, 1.000000000000000000 ) ) ;
#30941 = CARTESIAN_POINT ( 'NONE',  ( 47.79865503179234310, 9.702389020015065313, -4.315940132965163656 ) ) ;
#30942 = EDGE_LOOP ( 'NONE', ( #18509, #12654, #27944, #9523 ) ) ;
#30943 = DIRECTION ( 'NONE',  ( -1.101824276508909887E-16, 1.000000000000000000, -0.000000000000000000 ) ) ;
#30944 = EDGE_LOOP ( 'NONE', ( #5991, #17160, #12766, #18020, #22159 ) ) ;
#30945 = EDGE_CURVE ( 'NONE', #8602, #28135, #12222, .T. ) ;
#30946 = AXIS2_PLACEMENT_3D ( 'NONE', #11301, #1768, #26552 ) ;
#30947 = CIRCLE ( 'NONE', #16765, 0.1250000000000001110 ) ;
#30948 = EDGE_CURVE ( 'NONE', #7900, #20619, #20066, .T. ) ;
#30949 = ORIENTED_EDGE ( 'NONE', *, *, #29258, .F. ) ;
#30950 = AXIS2_PLACEMENT_3D ( 'NONE', #28294, #23364, #30920 ) ;
#30951 = CIRCLE ( 'NONE', #547, 1.499999999999997780 ) ;
#30952 = VECTOR ( 'NONE', #23014, 1000.000000000000000 ) ;
#30953 = EDGE_CURVE ( 'NONE', #28083, #7551, #10648, .T. ) ;
#30954 = CARTESIAN_POINT ( 'NONE',  ( -40.70335362822509495, 9.387769322903325886, 39.54930799450052348 ) ) ;
#30955 = CARTESIAN_POINT ( 'NONE',  ( 45.96182992765471909, 15.77906836436399374, 44.82232689504101586 ) ) ;
#30956 = DIRECTION ( 'NONE',  ( -1.000000000000000000, -1.101824276508909887E-16, 0.000000000000000000 ) ) ;
#30957 = AXIS2_PLACEMENT_3D ( 'NONE', #10415, #8272, #20409 ) ;
#30958 = EDGE_LOOP ( 'NONE', ( #22351, #23840 ) ) ;
#30959 = CARTESIAN_POINT ( 'NONE',  ( -40.76967387488526384, 8.530668925462080665, 39.44930799450052206 ) ) ;
#30960 = ORIENTED_EDGE ( 'NONE', *, *, #29853, .T. ) ;
#30961 = CARTESIAN_POINT ( 'NONE',  ( 47.09785597605719687, 23.12036939723557083, 47.04930799450080059 ) ) ;
#30962 = FACE_OUTER_BOUND ( 'NONE', #12806, .T. ) ;
#30963 = CARTESIAN_POINT ( 'NONE',  ( -36.86121898886836590, -5.510771003736198992, 79.29205363043402599 ) ) ;
#30964 = DIRECTION ( 'NONE',  ( -1.000000000000000000, 0.000000000000000000, 0.000000000000000000 ) ) ;
#30965 = ORIENTED_EDGE ( 'NONE', *, *, #15719, .F. ) ;
#30966 = CARTESIAN_POINT ( 'NONE',  ( 21.09992658989239089, 29.84143805560861296, 47.04930799450051637 ) ) ;
#30967 = DIRECTION ( 'NONE',  ( 0.000000000000000000, 0.000000000000000000, -1.000000000000000000 ) ) ;
#30968 = DIRECTION ( 'NONE',  ( -1.224646799147353207E-16, -1.349345573449484691E-32, 1.000000000000000000 ) ) ;
#30969 = DIRECTION ( 'NONE',  ( 0.000000000000000000, 1.000000000000000000, 0.000000000000000000 ) ) ;
#30970 = ORIENTED_EDGE ( 'NONE', *, *, #10581, .T. ) ;
#30971 = TOROIDAL_SURFACE ( 'NONE', #16278, 12.40141737965283042, 0.1249999999999995420 ) ;
#30972 = CARTESIAN_POINT ( 'NONE',  ( -41.77464577679393187, 3.808795504615559047, 32.14930799450051779 ) ) ;
#30973 = CARTESIAN_POINT ( 'NONE',  ( 21.09785597605719687, 25.76454579224776964, 15.54930799450051460 ) ) ;
#30974 = DIRECTION ( 'NONE',  ( -1.101824276508909887E-16, 1.000000000000000000, -0.000000000000000000 ) ) ;
#30975 = CARTESIAN_POINT ( 'NONE',  ( 21.09992658989238734, 38.56284415653841791, 47.04930799450051637 ) ) ;
#30976 = ORIENTED_EDGE ( 'NONE', *, *, #31710, .T. ) ;
#30977 = VECTOR ( 'NONE', #10020, 1000.000000000000114 ) ;
#30978 = DIRECTION ( 'NONE',  ( 0.4848096202463627602, 0.8746197071393815303, 0.000000000000000000 ) ) ;
#30979 = CARTESIAN_POINT ( 'NONE',  ( -40.49379808738692788, 7.146223304870686022, 35.15525948572338422 ) ) ;
#30980 = VERTEX_POINT ( 'NONE', #17489 ) ;
#30981 = CIRCLE ( 'NONE', #16799, 12.62506659569710443 ) ;
#30982 = DIRECTION ( 'NONE',  ( -0.9612616959383183390, -0.2756373558170014948, -8.795445018805493151E-19 ) ) ;
#30983 = CIRCLE ( 'NONE', #551, 0.1000000000000004774 ) ;
#30984 = CARTESIAN_POINT ( 'NONE',  ( 48.34748475735720064, 24.70653309617948423, 49.49898713858203791 ) ) ;
#30985 = VERTEX_POINT ( 'NONE', #22897 ) ;
#30986 = ORIENTED_EDGE ( 'NONE', *, *, #30991, .F. ) ;
#30987 = CARTESIAN_POINT ( 'NONE',  ( -11.32029359255892764, -5.395280703882725959, 104.8375434467133118 ) ) ;
#30988 = CIRCLE ( 'NONE', #24676, 12.27641737965288904 ) ;
#30989 = ORIENTED_EDGE ( 'NONE', *, *, #10097, .T. ) ;
#30990 = EDGE_CURVE ( 'NONE', #26992, #11078, #664, .T. ) ;
#30991 = EDGE_CURVE ( 'NONE', #17073, #20369, #24252, .T. ) ;
#30992 = ADVANCED_FACE ( 'NONE', ( #30139 ), #10120, .T. ) ;
#30993 = CIRCLE ( 'NONE', #16823, 0.09999999999999795164 ) ;
#30994 = ORIENTED_EDGE ( 'NONE', *, *, #8618, .T. ) ;
#30995 = TOROIDAL_SURFACE ( 'NONE', #2688, 12.40141737965282687, 0.1250000000000004718 ) ;
#30996 = VERTEX_POINT ( 'NONE', #7652 ) ;
#30997 = DIRECTION ( 'NONE',  ( -0.8746197071393810862, 0.4848096202463637039, 8.676864087101942305E-18 ) ) ;
#30998 = CARTESIAN_POINT ( 'NONE',  ( 21.09785597605719332, 12.06852548259731961, -8.628907523723306383 ) ) ;
#30999 = DIRECTION ( 'NONE',  ( 0.000000000000000000, 1.000000000000000000, 0.000000000000000000 ) ) ;
#31000 = CARTESIAN_POINT ( 'NONE',  ( 49.44739180854976013, 26.63456182964376850, 47.17133137409169308 ) ) ;
#31001 = ORIENTED_EDGE ( 'NONE', *, *, #21474, .F. ) ;
#31002 = ORIENTED_EDGE ( 'NONE', *, *, #13645, .F. ) ;
#31003 = DIRECTION ( 'NONE',  ( -1.000000000000000000, -1.101824276508910010E-16, 0.000000000000000000 ) ) ;
#31004 = AXIS2_PLACEMENT_3D ( 'NONE', #22213, #19425, #29453 ) ;
#31005 = ORIENTED_EDGE ( 'NONE', *, *, #4262, .F. ) ;
#31006 = CARTESIAN_POINT ( 'NONE',  ( 49.66977585544405827, 24.86874180309281712, 46.07579470028509405 ) ) ;
#31007 = DIRECTION ( 'NONE',  ( 0.000000000000000000, 0.000000000000000000, -1.000000000000000000 ) ) ;
#31008 = FACE_OUTER_BOUND ( 'NONE', #17997, .T. ) ;
#31009 = DIRECTION ( 'NONE',  ( -1.000000000000000000, -1.101824276508909887E-16, 0.000000000000000000 ) ) ;
#31010 = CARTESIAN_POINT ( 'NONE',  ( 21.09992658989239089, 30.59143805560860585, 47.04930799450051637 ) ) ;
#31011 = CONTEXT_DEPENDENT_SHAPE_REPRESENTATION ( #27554, #6676 ) ;
#31012 = ORIENTED_EDGE ( 'NONE', *, *, #11440, .T. ) ;
#31013 = PLANE ( 'NONE',  #4006 ) ;
#31014 = CARTESIAN_POINT ( 'NONE',  ( -33.25903338348492611, -2.742229146546061980, 13.28678055525370993 ) ) ;
#31015 = CARTESIAN_POINT ( 'NONE',  ( 21.09785597605719332, 40.56454579224780588, 47.04930799450051637 ) ) ;
#31016 = CIRCLE ( 'NONE', #19992, 0.1250000000000001110 ) ;
#31017 = DIRECTION ( 'NONE',  ( -0.000000000000000000, -1.000000000000000000, -0.000000000000000000 ) ) ;
#31018 = CARTESIAN_POINT ( 'NONE',  ( 48.40186567930497574, 26.11618040159426357, 45.03923535223908203 ) ) ;
#31019 = AXIS2_PLACEMENT_3D ( 'NONE', #26522, #6662, #2057 ) ;
#31020 = EDGE_LOOP ( 'NONE', ( #32017, #9663, #9589, #13668 ) ) ;
#31021 = CARTESIAN_POINT ( 'NONE',  ( 47.09785597605719687, 25.56454579224779877, 47.04930799450042400 ) ) ;
#31022 = CYLINDRICAL_SURFACE ( 'NONE', #15146, 12.36707279061065101 ) ;
#31023 = EDGE_CURVE ( 'NONE', #5687, #10697, #28457, .T. ) ;
#31024 = ORIENTED_EDGE ( 'NONE', *, *, #28841, .F. ) ;
#31025 = CIRCLE ( 'NONE', #6913, 1.000000000001013856 ) ;
#31026 = ADVANCED_FACE ( 'NONE', ( #17316 ), #12747, .T. ) ;
#31027 = EDGE_CURVE ( 'NONE', #3952, #18274, #252, .T. ) ;
#31028 = EDGE_CURVE ( 'NONE', #6052, #26923, #9785, .T. ) ;
#31029 = ORIENTED_EDGE ( 'NONE', *, *, #12386, .F. ) ;
#31030 = ADVANCED_FACE ( 'NONE', ( #10435 ), #2397, .F. ) ;
#31031 = CARTESIAN_POINT ( 'NONE',  ( -39.00632496464983490, 3.646315102566973998, 47.04930799450051637 ) ) ;
#31032 = DIRECTION ( 'NONE',  ( 0.000000000000000000, -1.000000000000000000, 0.000000000000000000 ) ) ;
#31033 = CARTESIAN_POINT ( 'NONE',  ( 48.83059987400639557, 27.68213139976340642, 48.97189179988552610 ) ) ;
#31034 = B_SPLINE_CURVE_WITH_KNOTS ( 'NONE', 3,
 ( #6160, #5523, #20614, #908, #15527, #30961 ),
 .UNSPECIFIED., .F., .F.,
 ( 4, 2, 4 ),
 ( 0.000000000000000000, 0.5000000000000000000, 1.000000000000000000 ),
 .UNSPECIFIED. ) ;
#31035 = ORIENTED_EDGE ( 'NONE', *, *, #22205, .F. ) ;
#31036 = AXIS2_PLACEMENT_3D ( 'NONE', #17957, #25829, #15823 ) ;
#31037 = CARTESIAN_POINT ( 'NONE',  ( -32.92991496113891259, -13.30632128221581567, 32.57800810680159742 ) ) ;
#31038 = CIRCLE ( 'NONE', #2728, 12.62506659569710443 ) ;
#31039 = CARTESIAN_POINT ( 'NONE',  ( 21.09785597605720753, 14.86454579224779948, 47.04930799450052348 ) ) ;
#31040 = DIRECTION ( 'NONE',  ( -0.000000000000000000, -1.000000000000000000, 0.000000000000000000 ) ) ;
#31041 = ORIENTED_EDGE ( 'NONE', *, *, #982, .F. ) ;
#31042 = PLANE ( 'NONE',  #899 ) ;
#31043 = ORIENTED_EDGE ( 'NONE', *, *, #6481, .F. ) ;
#31044 = DIRECTION ( 'NONE',  ( -0.000000000000000000, -1.000000000000000000, 0.000000000000000000 ) ) ;
#31045 = DIRECTION ( 'NONE',  ( -1.000000000000000000, -1.101824276508909887E-16, 0.000000000000000000 ) ) ;
#31046 = FACE_OUTER_BOUND ( 'NONE', #9836, .T. ) ;
#31047 = CARTESIAN_POINT ( 'NONE',  ( 21.09992658989239089, 27.21183152705960495, 47.04930799450051637 ) ) ;
#31048 = ORIENTED_EDGE ( 'NONE', *, *, #30721, .T. ) ;
#31049 = ORIENTED_EDGE ( 'NONE', *, *, #10278, .T. ) ;
#31050 = FACE_OUTER_BOUND ( 'NONE', #17651, .T. ) ;
#31051 = CIRCLE ( 'NONE', #21073, 0.1000000000000016431 ) ;
#31052 = PLANE ( 'NONE',  #8830 ) ;
#31053 = DIRECTION ( 'NONE',  ( -0.000000000000000000, -1.000000000000000000, 0.000000000000000000 ) ) ;
#31054 = CIRCLE ( 'NONE', #16413, 12.62506659569710266 ) ;
#31055 = ORIENTED_EDGE ( 'NONE', *, *, #24979, .T. ) ;
#31056 = DIRECTION ( 'NONE',  ( -1.224646799147353207E-16, -1.349345573449484691E-32, 1.000000000000000000 ) ) ;
#31057 = CARTESIAN_POINT ( 'NONE',  ( 49.32483701613094240, 28.40322093266652104, 45.91328182968236860 ) ) ;
#31058 = ORIENTED_EDGE ( 'NONE', *, *, #23975, .F. ) ;
#31059 = CARTESIAN_POINT ( 'NONE',  ( -43.29662792673756400, 1.063067023446606196, 53.64930799450051779 ) ) ;
#31060 = CARTESIAN_POINT ( 'NONE',  ( 48.46535932150934656, 26.88954579807171186, 49.73005965046827015 ) ) ;
#31061 = EDGE_CURVE ( 'NONE', #1048, #19411, #12250, .T. ) ;
#31062 = EDGE_CURVE ( 'NONE', #29646, #30180, #29806, .T. ) ;
#31063 = AXIS2_PLACEMENT_3D ( 'NONE', #30525, #8041, #2616 ) ;
#31064 = DIRECTION ( 'NONE',  ( 0.000000000000000000, 0.000000000000000000, -1.000000000000000000 ) ) ;
#31065 = CIRCLE ( 'NONE', #16892, 2.500000000000002220 ) ;
#31066 = B_SPLINE_CURVE_WITH_KNOTS ( 'NONE', 3,
 ( #18732, #25816, #3161, #8264, #6119, #20729 ),
 .UNSPECIFIED., .F., .F.,
 ( 4, 2, 4 ),
 ( 0.000000000000000000, 0.5000000000000000000, 1.000000000000000000 ),
 .UNSPECIFIED. ) ;
#31067 = AXIS2_PLACEMENT_3D ( 'NONE', #32263, #27156, #14699 ) ;
#31068 = ORIENTED_EDGE ( 'NONE', *, *, #10838, .F. ) ;
#31069 = ADVANCED_FACE ( 'NONE', ( #15035 ), #19777, .F. ) ;
#31070 = CARTESIAN_POINT ( 'NONE',  ( 8.823509210239585343, 32.09164230456639899, 47.04930799450051637 ) ) ;
#31071 = CARTESIAN_POINT ( 'NONE',  ( 21.09992658989239089, 23.84184655352419213, 47.04930799450051637 ) ) ;
#31072 = ORIENTED_EDGE ( 'NONE', *, *, #22862, .T. ) ;
#31073 = VECTOR ( 'NONE', #15606, 1000.000000000000000 ) ;
#31074 = DIRECTION ( 'NONE',  ( 7.588956326749211550E-18, -4.206627182996911684E-18, 1.000000000000000000 ) ) ;
#31076 = CARTESIAN_POINT ( 'NONE',  ( 45.19785535133951271, 22.86454579224779948, 46.30324912166403806 ) ) ;
#31075 = VECTOR ( 'NONE', #2963, 1000.000000000000114 ) ;
#31077 = CARTESIAN_POINT ( 'NONE',  ( 72.64898409407776114, 3.957035103101694151, 15.81524687697156928 ) ) ;
#31078 = VERTEX_POINT ( 'NONE', #32431 ) ;
#31079 = DIRECTION ( 'NONE',  ( 1.000000000000000000, 0.000000000000000000, -1.110223024625154963E-14 ) ) ;
#31080 = CARTESIAN_POINT ( 'NONE',  ( 21.09785597605719332, 30.56454579224779522, 79.54930799450052348 ) ) ;
#31081 = LINE ( 'NONE', #15968, #6274 ) ;
#31082 = VECTOR ( 'NONE', #8174, 1000.000000000000000 ) ;
#31083 = EDGE_CURVE ( 'NONE', #18497, #321, #12253, .T. ) ;
#31084 = DIRECTION ( 'NONE',  ( -1.000000000000000000, -1.101824276508909887E-16, 0.000000000000000000 ) ) ;
#31085 = FILL_AREA_STYLE_COLOUR ( '', #3441 ) ;
#31086 = ORIENTED_EDGE ( 'NONE', *, *, #15041, .T. ) ;
#31087 = CARTESIAN_POINT ( 'NONE',  ( 33.46699938050303302, 38.56284415653841791, 47.04930799450051637 ) ) ;
#31088 = DIRECTION ( 'NONE',  ( -1.000000000000000000, 0.000000000000000000, 0.000000000000000000 ) ) ;
#31089 = FACE_OUTER_BOUND ( 'NONE', #27895, .T. ) ;
#31090 = EDGE_CURVE ( 'NONE', #231, #11810, #5948, .T. ) ;
#31091 = CARTESIAN_POINT ( 'NONE',  ( 21.09992658989239089, 23.59164230456639544, 47.04930799450051637 ) ) ;
#31092 = CARTESIAN_POINT ( 'NONE',  ( -42.38687957179149635, 4.148162238788000167, 39.04930799450052348 ) ) ;
#31093 = VERTEX_POINT ( 'NONE', #20912 ) ;
#31094 = DIRECTION ( 'NONE',  ( 1.188208965918165239E-16, 1.880121038077813132E-16, 1.000000000000000000 ) ) ;
#31095 = CARTESIAN_POINT ( 'NONE',  ( -40.55202315603386864, 7.223587105649683870, 38.76578233797366835 ) ) ;
#31096 = CARTESIAN_POINT ( 'NONE',  ( -0.4021440239427923058, -5.098646251524523443, 47.04930799450052348 ) ) ;
#31097 = ORIENTED_EDGE ( 'NONE', *, *, #27936, .F. ) ;
#31098 = DIRECTION ( 'NONE',  ( 0.9612616959383221138, 0.2756373558169876170, 0.000000000000000000 ) ) ;
#31099 = DIRECTION ( 'NONE',  ( 0.000000000000000000, 0.000000000000000000, 1.000000000000000000 ) ) ;
#31100 = EDGE_CURVE ( 'NONE', #6039, #5895, #25339, .T. ) ;
#31101 = ADVANCED_FACE ( 'NONE', ( #1057 ), #26903, .F. ) ;
#31102 = CARTESIAN_POINT ( 'NONE',  ( 49.19517401419062708, 28.98655426599985319, 48.40991706654173754 ) ) ;
#31103 = DIRECTION ( 'NONE',  ( -1.000000000000000000, 0.000000000000000000, 0.000000000000000000 ) ) ;
#31104 = EDGE_CURVE ( 'NONE', #2726, #13343, #8565, .T. ) ;
#31105 = CIRCLE ( 'NONE', #16393, 0.9999999999999940048 ) ;
#31106 = ORIENTED_EDGE ( 'NONE', *, *, #6994, .F. ) ;
#31107 = LINE ( 'NONE', #8612, #26137 ) ;
#31108 = ORIENTED_EDGE ( 'NONE', *, *, #1779, .F. ) ;
#31109 = AXIS2_PLACEMENT_3D ( 'NONE', #10666, #30677, #18180 ) ;
#31110 = ORIENTED_EDGE ( 'NONE', *, *, #10814, .T. ) ;
#31111 = TOROIDAL_SURFACE ( 'NONE', #13815, 12.40141737965287128, 0.1249999999999993477 ) ;
#31112 = CIRCLE ( 'NONE', #31625, 0.09999999999999836797 ) ;
#31113 = EDGE_CURVE ( 'NONE', #29641, #4406, #3510, .T. ) ;
#31114 = DIRECTION ( 'NONE',  ( -0.9986540920324801229, -1.233316085972235573E-16, -0.05186525298099663173 ) ) ;
#31115 = CARTESIAN_POINT ( 'NONE',  ( -36.98761417531858342, -5.935454207752198563, 77.87546120947918382 ) ) ;
#31116 = DIRECTION ( 'NONE',  ( -1.101824276508909887E-16, 1.000000000000000000, -0.000000000000000000 ) ) ;
#31117 = VERTEX_POINT ( 'NONE', #25686 ) ;
#31118 = CYLINDRICAL_SURFACE ( 'NONE', #10901, 13.00178401536290806 ) ;
#31119 = EDGE_LOOP ( 'NONE', ( #25253, #5875, #2587, #15708 ) ) ;
#31120 = CIRCLE ( 'NONE', #12793, 71.29999999999996874 ) ;
#31121 = CARTESIAN_POINT ( 'NONE',  ( 21.09992658989239089, 28.71183152705961206, 47.04930799450051637 ) ) ;
#31122 = CARTESIAN_POINT ( 'NONE',  ( 21.09785597605719332, 16.86454579224779948, -1.584744370635042587 ) ) ;
#31123 = EDGE_CURVE ( 'NONE', #31925, #5749, #1741, .T. ) ;
#31124 = DIRECTION ( 'NONE',  ( -0.000000000000000000, -1.000000000000000000, 0.000000000000000000 ) ) ;
#31125 = ORIENTED_EDGE ( 'NONE', *, *, #5396, .F. ) ;
#31126 = CARTESIAN_POINT ( 'NONE',  ( 21.09992658989239089, 27.59184655352419568, 47.04930799450051637 ) ) ;
#31127 = ORIENTED_EDGE ( 'NONE', *, *, #22067, .F. ) ;
#31128 = DIRECTION ( 'NONE',  ( 0.4848096202463645921, 0.8746197071393805311, 0.000000000000000000 ) ) ;
#31129 = FACE_BOUND ( 'NONE', #10768, .T. ) ;
#31130 = ORIENTED_EDGE ( 'NONE', *, *, #28504, .T. ) ;
#31131 = CARTESIAN_POINT ( 'NONE',  ( 21.09785597605719332, 25.56454579224779877, 58.84930799450049221 ) ) ;
#31132 = ADVANCED_FACE ( 'NONE', ( #25998 ), #11703, .T. ) ;
#31133 = CARTESIAN_POINT ( 'NONE',  ( -40.11286833322908052, 2.887657226147511302, 57.04930799450051637 ) ) ;
#31134 = CARTESIAN_POINT ( 'NONE',  ( -40.65487266620045403, 9.475231293617264683, 39.43717596014455040 ) ) ;
#31135 = FACE_OUTER_BOUND ( 'NONE', #19689, .T. ) ;
#31136 = CIRCLE ( 'NONE', #11727, 0.2000000000000005107 ) ;
#31137 = CIRCLE ( 'NONE', #22739, 12.36707279061065101 ) ;
#31138 = ORIENTED_EDGE ( 'NONE', *, *, #19402, .T. ) ;
#31139 = DIRECTION ( 'NONE',  ( -1.000000000000000000, 0.000000000000000000, 0.000000000000000000 ) ) ;
#31140 = CARTESIAN_POINT ( 'NONE',  ( -40.57495275781082711, 7.492308784443611813, 35.33000499469285671 ) ) ;
#31141 = ORIENTED_EDGE ( 'NONE', *, *, #29126, .T. ) ;
#31142 = DIRECTION ( 'NONE',  ( 0.000000000000000000, 0.000000000000000000, 1.000000000000000000 ) ) ;
#31143 = EDGE_CURVE ( 'NONE', #12308, #29171, #10915, .T. ) ;
#31144 = DIRECTION ( 'NONE',  ( -0.000000000000000000, -1.000000000000000000, -0.000000000000000000 ) ) ;
#31145 = EDGE_CURVE ( 'NONE', #8289, #10562, #13065, .T. ) ;
#31146 = VERTEX_POINT ( 'NONE', #20595 ) ;
#31147 = TOROIDAL_SURFACE ( 'NONE', #4395, 12.40141737965287660, 0.1250000000000007772 ) ;
#31148 = ORIENTED_EDGE ( 'NONE', *, *, #23274, .T. ) ;
#31149 = PRODUCT_DEFINITION_CONTEXT ( 'detailed design', #6357, 'design' ) ;
#31150 = ORIENTED_EDGE ( 'NONE', *, *, #1766, .T. ) ;
#31151 = CIRCLE ( 'NONE', #8671, 12.36707279061065101 ) ;
#31152 = ORIENTED_EDGE ( 'NONE', *, *, #31090, .F. ) ;
#31153 = CARTESIAN_POINT ( 'NONE',  ( -43.64073206722599707, 1.267352857069779626, 34.64930799450052490 ) ) ;
#31154 = VERTEX_POINT ( 'NONE', #28476 ) ;
#31155 = CARTESIAN_POINT ( 'NONE',  ( 47.73724253767792192, 22.99884124225578219, 48.30271392650413276 ) ) ;
#31156 = DIRECTION ( 'NONE',  ( 1.000000000000000000, 0.000000000000000000, -1.110223024625154963E-14 ) ) ;
#31157 = CARTESIAN_POINT ( 'NONE',  ( 21.09785597605719332, 25.13358275951983956, 7.413771787092404253 ) ) ;
#31158 = CARTESIAN_POINT ( 'NONE',  ( 45.81741271322955100, 27.10122849631043351, 49.02305402274571122 ) ) ;
#31159 = VERTEX_POINT ( 'NONE', #13232 ) ;
#31160 = ORIENTED_EDGE ( 'NONE', *, *, #12950, .F. ) ;
#31161 = ORIENTED_EDGE ( 'NONE', *, *, #26671, .F. ) ;
#31162 = DIRECTION ( 'NONE',  ( -1.000000000000000000, 0.000000000000000000, 0.000000000000000000 ) ) ;
#31163 = PLANE ( 'NONE',  #7359 ) ;
#31164 = DIRECTION ( 'NONE',  ( 0.2603858710390620779, -0.9080734476337356531, 0.3280271511107128446 ) ) ;
#31165 = CIRCLE ( 'NONE', #29572, 12.62506659569710266 ) ;
#31166 = CIRCLE ( 'NONE', #7047, 12.36707279061065101 ) ;
#31167 = CARTESIAN_POINT ( 'NONE',  ( 21.09992658989238734, 32.09164230456639899, 47.04930799450051637 ) ) ;
#31168 = PLANE ( 'NONE',  #5433 ) ;
#31169 = CIRCLE ( 'NONE', #13873, 0.09999999999999795164 ) ;
#31170 = CONTEXT_DEPENDENT_SHAPE_REPRESENTATION ( #10159, #31844 ) ;
#31171 = ORIENTED_EDGE ( 'NONE', *, *, #23494, .T. ) ;
#31172 = PLANE ( 'NONE',  #29695 ) ;
#31173 = DIRECTION ( 'NONE',  ( 1.000000000000000000, 0.000000000000000000, 0.000000000000000000 ) ) ;
#31174 = TOROIDAL_SURFACE ( 'NONE', #21187, 12.61792373059894068, 0.1249999999999991118 ) ;
#31175 = DIRECTION ( 'NONE',  ( 0.000000000000000000, 0.000000000000000000, 1.000000000000000000 ) ) ;
#31176 = CIRCLE ( 'NONE', #15980, 0.6000000000000033085 ) ;
#31177 = EDGE_CURVE ( 'NONE', #16985, #17658, #13288, .T. ) ;
#31178 = AXIS2_PLACEMENT_3D ( 'NONE', #19382, #24148, #9221 ) ;
#31179 = DIRECTION ( 'NONE',  ( -1.101824276508909887E-16, 1.000000000000000000, -0.000000000000000000 ) ) ;
#31180 = CARTESIAN_POINT ( 'NONE',  ( 8.823509210239564027, 29.59164230456639899, 47.04930799450051637 ) ) ;
#31181 = EDGE_CURVE ( 'NONE', #2384, #7990, #12779, .T. ) ;
#31182 = ORIENTED_EDGE ( 'NONE', *, *, #31895, .T. ) ;
#31183 = DIRECTION ( 'NONE',  ( -1.101824276508909887E-16, 1.000000000000000000, -0.000000000000000000 ) ) ;
#31184 = ORIENTED_EDGE ( 'NONE', *, *, #28166, .F. ) ;
#31185 = CARTESIAN_POINT ( 'NONE',  ( 21.09785597605720042, 25.18020726757345429, 87.53672989447419184 ) ) ;
#31186 = CARTESIAN_POINT ( 'NONE',  ( 21.09785597605719332, 7.264443105416139801, 47.04930799450051637 ) ) ;
#31187 = ORIENTED_EDGE ( 'NONE', *, *, #32280, .T. ) ;
#31188 = AXIS2_PLACEMENT_3D ( 'NONE', #21651, #6724, #16718 ) ;
#31189 = ORIENTED_EDGE ( 'NONE', *, *, #11566, .T. ) ;
#31190 = AXIS2_PLACEMENT_3D ( 'NONE', #24818, #12519, #29745 ) ;
#31191 = DIRECTION ( 'NONE',  ( 1.000000000000000000, 0.000000000000000000, 0.000000000000000000 ) ) ;
#31192 = LINE ( 'NONE', #23472, #31757 ) ;
#31194 = CARTESIAN_POINT ( 'NONE',  ( 21.09992658989239089, 24.34164230456639544, 47.04930799450051637 ) ) ;
#31193 = AXIS2_PLACEMENT_3D ( 'NONE', #24040, #1552, #7141 ) ;
#31195 = AXIS2_PLACEMENT_3D ( 'NONE', #17629, #25023, #27646 ) ;
#31196 = AXIS2_PLACEMENT_3D ( 'NONE', #4259, #26907, #31516 ) ;
#31197 = ORIENTED_EDGE ( 'NONE', *, *, #29810, .F. ) ;
#31198 = DIRECTION ( 'NONE',  ( 0.000000000000000000, 0.000000000000000000, -1.000000000000000000 ) ) ;
#31199 = CARTESIAN_POINT ( 'NONE',  ( -35.17013276111289599, 11.90988849664400284, 40.33535627974906390 ) ) ;
#31200 = DIRECTION ( 'NONE',  ( -1.101824276508909887E-16, 1.000000000000000000, -0.000000000000000000 ) ) ;
#31201 = EDGE_LOOP ( 'NONE', ( #6194, #7726, #6845, #27631 ) ) ;
#31202 = CYLINDRICAL_SURFACE ( 'NONE', #1272, 12.62506659569710443 ) ;
#31203 = ORIENTED_EDGE ( 'NONE', *, *, #20964, .T. ) ;
#31204 = CARTESIAN_POINT ( 'NONE',  ( -33.00214402394279745, 14.36454579224779948, 47.04930799450052348 ) ) ;
#31205 = CARTESIAN_POINT ( 'NONE',  ( 48.22039229833278995, 29.17080963813146965, 44.81246039718205765 ) ) ;
#31206 = CARTESIAN_POINT ( 'NONE',  ( -40.69616936570353971, 6.785751122969994498, 34.64127309652835152 ) ) ;
#31207 = EDGE_LOOP ( 'NONE', ( #17373, #18818, #1846, #20158 ) ) ;
#31208 = ORIENTED_EDGE ( 'NONE', *, *, #17114, .T. ) ;
#31209 = CARTESIAN_POINT ( 'NONE',  ( 28.40365102626035565, -13.30632128221581034, 102.5023864623932894 ) ) ;
#31210 = DIRECTION ( 'NONE',  ( 1.000000000000000000, -0.000000000000000000, -0.000000000000000000 ) ) ;
#31211 = EDGE_CURVE ( 'NONE', #8513, #17105, #22040, .T. ) ;
#31212 = EDGE_CURVE ( 'NONE', #10074, #21925, #22185, .T. ) ;
#31213 = CARTESIAN_POINT ( 'NONE',  ( 21.09992658989239089, 24.46664230456639899, 47.04930799450051637 ) ) ;
#31214 = ADVANCED_FACE ( 'NONE', ( #14346 ), #31111, .T. ) ;
#31215 = AXIS2_PLACEMENT_3D ( 'NONE', #1112, #3734, #8669 ) ;
#31216 = EDGE_CURVE ( 'NONE', #29624, #2645, #16395, .T. ) ;
#31217 = ORIENTED_EDGE ( 'NONE', *, *, #24865, .F. ) ;
#31218 = FACE_OUTER_BOUND ( 'NONE', #9510, .T. ) ;
#31219 = DIRECTION ( 'NONE',  ( -6.722685822323786766E-17, 1.000000000000000000, -0.000000000000000000 ) ) ;
#31220 = EDGE_CURVE ( 'NONE', #27541, #10718, #3310, .T. ) ;
#31221 = EDGE_LOOP ( 'NONE', ( #3455, #26558, #6792, #8293 ) ) ;
#31223 = AXIS2_PLACEMENT_3D ( 'NONE', #19315, #3904, #29340 ) ;
#31222 = CARTESIAN_POINT ( 'NONE',  ( 21.09785597605720042, -16.93545420775220478, 47.04930799450051637 ) ) ;
#31224 = ADVANCED_FACE ( 'NONE', ( #9586 ), #30060, .T. ) ;
#31225 = CARTESIAN_POINT ( 'NONE',  ( 50.10320668408830613, 28.40621246473837402, 47.20539118556276037 ) ) ;
#31226 = CIRCLE ( 'NONE', #29622, 84.30000000000001137 ) ;
#31227 = CARTESIAN_POINT ( 'NONE',  ( 21.09992658989239089, 27.47145308207318593, 47.04930799450051637 ) ) ;
#31228 = CIRCLE ( 'NONE', #2913, 12.36707279061065279 ) ;
#31229 = CIRCLE ( 'NONE', #9750, 0.1249999999999983763 ) ;
#31230 = ORIENTED_EDGE ( 'NONE', *, *, #26049, .T. ) ;
#31231 = LINE ( 'NONE', #862, #29255 ) ;
#31232 = CARTESIAN_POINT ( 'NONE',  ( -43.73393778030726509, 1.305471833569777695, 60.54930799450051637 ) ) ;
#31233 = DIRECTION ( 'NONE',  ( -1.101824276508909887E-16, 1.000000000000000000, -0.000000000000000000 ) ) ;
#31234 = ORIENTED_EDGE ( 'NONE', *, *, #26593, .T. ) ;
#31235 = DIRECTION ( 'NONE',  ( -1.101824276508909887E-16, 1.000000000000000000, -0.000000000000000000 ) ) ;
#31236 = CARTESIAN_POINT ( 'NONE',  ( -41.04804154345566758, 9.288931653684134204, 34.54930799450051637 ) ) ;
#31237 = EDGE_CURVE ( 'NONE', #24256, #6225, #7520, .T. ) ;
#31238 = DIRECTION ( 'NONE',  ( 0.4832773644131139190, 0.8718554444429506001, -0.07944226231106060743 ) ) ;
#31239 = AXIS2_PLACEMENT_3D ( 'NONE', #4101, #21662, #3950 ) ;
#31240 = ORIENTED_EDGE ( 'NONE', *, *, #23309, .F. ) ;
#31241 = CARTESIAN_POINT ( 'NONE',  ( 33.50134396954525329, 26.09164230456639899, 47.04930799450051637 ) ) ;
#31242 = CARTESIAN_POINT ( 'NONE',  ( -40.60330327974818232, 7.565477138576674143, 53.88146687024394055 ) ) ;
#31243 = DIRECTION ( 'NONE',  ( -0.000000000000000000, -1.000000000000000000, 0.000000000000000000 ) ) ;
#31244 = CARTESIAN_POINT ( 'NONE',  ( 48.23388202445966044, 25.55087065737811969, 49.27628909396054979 ) ) ;
#31245 = CARTESIAN_POINT ( 'NONE',  ( -40.57832940339291383, 7.446916344587776848, 60.29072935073781991 ) ) ;
#31246 = ORIENTED_EDGE ( 'NONE', *, *, #28888, .F. ) ;
#31247 = DIRECTION ( 'NONE',  ( -1.000000000000000000, 0.000000000000000000, 0.000000000000000000 ) ) ;
#31248 = CARTESIAN_POINT ( 'NONE',  ( 47.20547626766765603, 27.48791119454915233, 44.97710074790751378 ) ) ;
#31249 = CARTESIAN_POINT ( 'NONE',  ( 21.09785597605720397, -16.63545420775219696, 131.2593585008393973 ) ) ;
#31250 = CARTESIAN_POINT ( 'NONE',  ( -40.11096502192368263, 6.858424625636979854, 34.59247500421662380 ) ) ;
#31251 = AXIS2_PLACEMENT_3D ( 'NONE', #11096, #21080, #24515 ) ;
#31252 = FACE_OUTER_BOUND ( 'NONE', #23737, .T. ) ;
#31253 = EDGE_LOOP ( 'NONE', ( #25857, #779 ) ) ;
#31254 = LINE ( 'NONE', #13530, #11902 ) ;
#31255 = DIRECTION ( 'NONE',  ( 1.000000000000000000, -0.000000000000000000, -0.000000000000000000 ) ) ;
#31256 = DIRECTION ( 'NONE',  ( -1.000000000000000000, 0.000000000000000000, 0.000000000000000000 ) ) ;
#31257 = ORIENTED_EDGE ( 'NONE', *, *, #7905, .T. ) ;
#31258 = ADVANCED_FACE ( 'NONE', ( #29445 ), #15357, .F. ) ;
#31259 = DIRECTION ( 'NONE',  ( -1.101824276508909887E-16, 1.000000000000000000, -0.000000000000000000 ) ) ;
#31260 = CARTESIAN_POINT ( 'NONE',  ( 21.09785597605719332, 11.78014697381582643, 102.6448323059792358 ) ) ;
#31261 = CARTESIAN_POINT ( 'NONE',  ( 21.09785597605719332, 14.56957104541719694, 47.04930799450051637 ) ) ;
#31262 = ORIENTED_EDGE ( 'NONE', *, *, #26421, .T. ) ;
#31263 = CARTESIAN_POINT ( 'NONE',  ( 48.14727188781975542, 22.80400562401890241, 49.10650501410607660 ) ) ;
#31264 = ORIENTED_EDGE ( 'NONE', *, *, #20818, .T. ) ;
#31265 = CIRCLE ( 'NONE', #6606, 1.624998423334082620 ) ;
#31266 = ORIENTED_EDGE ( 'NONE', *, *, #21426, .F. ) ;
#31267 = EDGE_CURVE ( 'NONE', #13235, #12313, #16933, .T. ) ;
#31268 = ADVANCED_FACE ( 'NONE', ( #4160 ), #3849, .T. ) ;
#31269 = AXIS2_PLACEMENT_3D ( 'NONE', #25168, #2838, #27793 ) ;
#31270 = LINE ( 'NONE', #25698, #18118 ) ;
#31271 = CARTESIAN_POINT ( 'NONE',  ( -33.01793443960422536, -2.346508597185796852, 80.78329740893839528 ) ) ;
#31272 = DIRECTION ( 'NONE',  ( -0.000000000000000000, -1.000000000000000000, 0.000000000000000000 ) ) ;
#31273 = EDGE_CURVE ( 'NONE', #30896, #163, #8923, .T. ) ;
#31274 = EDGE_CURVE ( 'NONE', #2185, #26286, #21120, .T. ) ;
#31275 = ORIENTED_EDGE ( 'NONE', *, *, #9227, .F. ) ;
#31276 = CARTESIAN_POINT ( 'NONE',  ( -40.61704948737776277, 6.826301864398534036, 34.55791711734467953 ) ) ;
#31277 = ORIENTED_EDGE ( 'NONE', *, *, #17859, .T. ) ;
#31278 = DIRECTION ( 'NONE',  ( -1.000000000000000000, -1.101824276508909887E-16, 0.000000000000000000 ) ) ;
#31279 = CARTESIAN_POINT ( 'NONE',  ( 33.46699938050304013, 30.22145308207317527, 47.04930799450050927 ) ) ;
#31280 = EDGE_LOOP ( 'NONE', ( #143, #4083, #7670, #16472 ) ) ;
#31281 = DIRECTION ( 'NONE',  ( -1.101824276508909887E-16, 1.000000000000000000, -0.000000000000000000 ) ) ;
#31282 = FACE_OUTER_BOUND ( 'NONE', #19004, .T. ) ;
#31283 = DIRECTION ( 'NONE',  ( -0.000000000000000000, -1.000000000000000000, 0.000000000000000000 ) ) ;
#31285 = SURFACE_SIDE_STYLE ('',( #26840 ) ) ;
#31284 = VECTOR ( 'NONE', #481, 1000.000000000000000 ) ;
#31286 = ORIENTED_EDGE ( 'NONE', *, *, #20572, .T. ) ;
#31287 = CARTESIAN_POINT ( 'NONE',  ( 48.23388202445966755, 27.52822092656774089, 49.27628909396054979 ) ) ;
#31288 = DIRECTION ( 'NONE',  ( -1.224646799147353207E-16, -1.349345573449484691E-32, 1.000000000000000000 ) ) ;
#31289 = CARTESIAN_POINT ( 'NONE',  ( 8.474859994195282908, 38.56284415653841791, 47.04930799450051637 ) ) ;
#31290 = CARTESIAN_POINT ( 'NONE',  ( 21.09785597605720753, 13.86454579224779948, 47.04930799450052348 ) ) ;
#31291 = DIRECTION ( 'NONE',  ( -0.000000000000000000, -1.000000000000000000, -0.000000000000000000 ) ) ;
#31292 = ORIENTED_EDGE ( 'NONE', *, *, #1108, .T. ) ;
#31293 = CARTESIAN_POINT ( 'NONE',  ( 21.09992658989239089, 24.22145308207319303, 47.04930799450051637 ) ) ;
#31294 = CARTESIAN_POINT ( 'NONE',  ( -40.70098307446937014, 6.778209214779045588, 34.68768967974548190 ) ) ;
#31295 = ORIENTED_EDGE ( 'NONE', *, *, #22444, .T. ) ;
#31296 = ADVANCED_FACE ( 'NONE', ( #26490 ), #10144, .F. ) ;
#31297 = CARTESIAN_POINT ( 'NONE',  ( -43.49322394822878834, -4.178071014601207445, 42.04930799450081480 ) ) ;
#31298 = B_SPLINE_CURVE_WITH_KNOTS ( 'NONE', 3,
 ( #5765, #674, #15772, #3451, #5284, #20848, #3289, #343, #8547, #25302, #23478, #13326 ),
 .UNSPECIFIED., .F., .F.,
 ( 4, 2, 2, 2, 2, 4 ),
 ( 0.0003078418816949101658, 0.0003848023521186742855, 0.0004232825873305365045, 0.0004617628225423987235, 0.0005387232929661524890, 0.0006156837633899062004 ),
 .UNSPECIFIED. ) ;
#31299 = AXIS2_PLACEMENT_3D ( 'NONE', #20523, #22824, #30554 ) ;
#31300 = LINE ( 'NONE', #3236, #25825 ) ;
#31301 = ORIENTED_EDGE ( 'NONE', *, *, #15561, .F. ) ;
#31302 = ORIENTED_EDGE ( 'NONE', *, *, #7680, .F. ) ;
#31303 = ORIENTED_EDGE ( 'NONE', *, *, #22654, .T. ) ;
#31304 = EDGE_CURVE ( 'NONE', #10913, #19411, #28869, .T. ) ;
#31305 = VECTOR ( 'NONE', #22433, 1000.000000000000114 ) ;
#31306 = ADVANCED_FACE ( 'NONE', ( #2684 ), #29535, .T. ) ;
#31307 = VERTEX_POINT ( 'NONE', #12541 ) ;
#31308 = CARTESIAN_POINT ( 'NONE',  ( -39.59300248568538194, 7.744584186742828891, 61.94930799450052206 ) ) ;
#31309 = ADVANCED_FACE ( 'NONE', ( #9751 ), #19560, .T. ) ;
#31310 = ORIENTED_EDGE ( 'NONE', *, *, #7457, .T. ) ;
#31311 = CARTESIAN_POINT ( 'NONE',  ( -41.23380787120766655, 11.23768311167744294, 37.04930799450052348 ) ) ;
#31312 = EDGE_CURVE ( 'NONE', #16068, #28989, #218, .T. ) ;
#31313 = CARTESIAN_POINT ( 'NONE',  ( 47.35361591473682097, 23.10527845304106265, 47.55068078453451363 ) ) ;
#31314 =( BOUNDED_CURVE ( )  B_SPLINE_CURVE ( 3, ( #18201, #6226, #25765, #23625 ),
 .UNSPECIFIED., .F., .F. ) 
 B_SPLINE_CURVE_WITH_KNOTS ( ( 4, 4 ),
 ( 0.6077475352746632975, 1.139624073389847503 ),
 .UNSPECIFIED. ) 
 CURVE ( )  GEOMETRIC_REPRESENTATION_ITEM ( )  RATIONAL_B_SPLINE_CURVE ( ( 1.000000000000000000, 0.9765642231641280535, 0.9765642231641280535, 1.000000000000000000 ) ) 
 REPRESENTATION_ITEM ( '' )  );
#31315 = CARTESIAN_POINT ( 'NONE',  ( -42.73182147790732444, -0.8057266458565844891, 61.94930799450052206 ) ) ;
#31316 = CARTESIAN_POINT ( 'NONE',  ( 45.18933221474103590, 24.76454579224779806, 43.30797974740836764 ) ) ;
#31317 = CARTESIAN_POINT ( 'NONE',  ( 49.44739180854976013, 27.37786309983298239, 47.17133137409169308 ) ) ;
#31318 = ORIENTED_EDGE ( 'NONE', *, *, #27698, .F. ) ;
#31319 = ORIENTED_EDGE ( 'NONE', *, *, #17407, .F. ) ;
#31320 = CARTESIAN_POINT ( 'NONE',  ( -40.02540636251514172, 2.839176264122877047, 55.04930799450051637 ) ) ;
#31321 = VERTEX_POINT ( 'NONE', #25167 ) ;
#31322 = CARTESIAN_POINT ( 'NONE',  ( 21.09785597605719332, -16.43042895458278352, 47.04930799450051637 ) ) ;
#31323 = CARTESIAN_POINT ( 'NONE',  ( -40.68283709840997631, 6.807248601136921984, 39.30095348056342885 ) ) ;
#31324 = CARTESIAN_POINT ( 'NONE',  ( -40.52510752649232728, 7.677764709599122384, 34.54930799450052348 ) ) ;
#31325 = FACE_OUTER_BOUND ( 'NONE', #23740, .T. ) ;
#31326 = CARTESIAN_POINT ( 'NONE',  ( -30.88361648749964772, 11.92558985988973141, 26.60346110398183583 ) ) ;
#31327 = FACE_OUTER_BOUND ( 'NONE', #620, .T. ) ;
#31328 = ORIENTED_EDGE ( 'NONE', *, *, #4706, .T. ) ;
#31329 = DIRECTION ( 'NONE',  ( -2.779292025043186357E-18, 1.288349127009862211E-17, -1.000000000000000000 ) ) ;
#31330 = DIRECTION ( 'NONE',  ( -1.101824276508909887E-16, 1.000000000000000000, -0.000000000000000000 ) ) ;
#31331 = CIRCLE ( 'NONE', #12990, 12.27641737965280200 ) ;
#31332 = CYLINDRICAL_SURFACE ( 'NONE', #31400, 12.36707279061065101 ) ;
#31333 = TOROIDAL_SURFACE ( 'NONE', #14631, 12.40141737965285174, 0.1249999999999993200 ) ;
#31334 = DIRECTION ( 'NONE',  ( -1.000000000000000000, -1.101824276508909887E-16, 0.000000000000000000 ) ) ;
#31335 = CARTESIAN_POINT ( 'NONE',  ( -40.99628586177130529, 8.927770518203464789, 56.04611646155296256 ) ) ;
#31336 = ORIENTED_EDGE ( 'NONE', *, *, #21401, .F. ) ;
#31337 = CARTESIAN_POINT ( 'NONE',  ( 21.09992658989238734, 38.56284415653841791, 47.04930799450051637 ) ) ;
#31338 = VECTOR ( 'NONE', #18117, 1000.000000000000000 ) ;
#31339 = EDGE_LOOP ( 'NONE', ( #2919, #28015, #905, #8628 ) ) ;
#31340 = DIRECTION ( 'NONE',  ( -1.101824276508909887E-16, 1.000000000000000000, -0.000000000000000000 ) ) ;
#31341 = CARTESIAN_POINT ( 'NONE',  ( 62.59785597605721819, 14.86454579224779948, 47.04930799450051637 ) ) ;
#31342 = AXIS2_PLACEMENT_3D ( 'NONE', #16804, #1875, #11890 ) ;
#31343 = VERTEX_POINT ( 'NONE', #29769 ) ;
#31344 = EDGE_CURVE ( 'NONE', #25267, #2286, #9909, .T. ) ;
#31345 = EDGE_CURVE ( 'NONE', #26091, #294, #19010, .T. ) ;
#31346 = ORIENTED_EDGE ( 'NONE', *, *, #23203, .T. ) ;
#31347 = CARTESIAN_POINT ( 'NONE',  ( 48.23388202445966755, 15.77906836436399374, 49.27628909396055690 ) ) ;
#31348 = AXIS2_PLACEMENT_3D ( 'NONE', #3432, #21142, #10515 ) ;
#31349 = CYLINDRICAL_SURFACE ( 'NONE', #17058, 0.09999999999999945044 ) ;
#31350 = DIRECTION ( 'NONE',  ( 0.000000000000000000, 0.000000000000000000, -1.000000000000000000 ) ) ;
#31351 = CIRCLE ( 'NONE', #17187, 12.52641737965279489 ) ;
#31352 = EDGE_CURVE ( 'NONE', #10115, #24757, #4891, .T. ) ;
#31353 = EDGE_LOOP ( 'NONE', ( #16368, #16392, #16409, #13128 ) ) ;
#31354 = AXIS2_PLACEMENT_3D ( 'NONE', #15825, #10424, #23043 ) ;
#31355 = CARTESIAN_POINT ( 'NONE',  ( 21.09992658989238734, 32.22145308207317527, 47.04930799450051637 ) ) ;
#31356 = AXIS2_PLACEMENT_3D ( 'NONE', #28550, #25152, #50 ) ;
#31357 = CARTESIAN_POINT ( 'NONE',  ( 21.09785597605719332, -15.93545420775219945, 47.04930799450051637 ) ) ;
#31358 = CARTESIAN_POINT ( 'NONE',  ( -40.11729073372970333, 6.802967823440400963, 39.44930799450052206 ) ) ;
#31359 = EDGE_LOOP ( 'NONE', ( #17535, #3348, #31669, #19984, #16875 ) ) ;
#31360 = CARTESIAN_POINT ( 'NONE',  ( -41.41619974353107381, 10.78537257809431615, 36.23067884439899444 ) ) ;
#31361 = ORIENTED_EDGE ( 'NONE', *, *, #19783, .T. ) ;
#31362 = CIRCLE ( 'NONE', #15633, 2.500000000000002220 ) ;
#31363 = FACE_BOUND ( 'NONE', #12830, .T. ) ;
#31364 = CARTESIAN_POINT ( 'NONE',  ( 21.09785597605719332, 30.56454579224779522, 47.04930799450051637 ) ) ;
#31365 = DIRECTION ( 'NONE',  ( 0.2756373558170082672, -0.9612616959383162296, -6.938893903907184201E-14 ) ) ;
#31366 = ORIENTED_EDGE ( 'NONE', *, *, #4038, .F. ) ;
#31367 = ORIENTED_EDGE ( 'NONE', *, *, #931, .F. ) ;
#31368 = CARTESIAN_POINT ( 'NONE',  ( 21.09992658989239089, 29.59184655352418858, 47.04930799450051637 ) ) ;
#31369 = LINE ( 'NONE', #18231, #17761 ) ;
#31370 = DIRECTION ( 'NONE',  ( -1.101824276508909887E-16, 1.000000000000000000, -0.000000000000000000 ) ) ;
#31371 = ORIENTED_EDGE ( 'NONE', *, *, #23668, .F. ) ;
#31372 = CARTESIAN_POINT ( 'NONE',  ( 0.6836613156275053171, 11.92558985988973497, -37.95069200549950494 ) ) ;
#31373 = CARTESIAN_POINT ( 'NONE',  ( 21.09992658989238734, 31.34164230456639544, 47.04930799450051637 ) ) ;
#31374 = EDGE_LOOP ( 'NONE', ( #18930, #31055, #16852, #29726 ) ) ;
#31375 = CARTESIAN_POINT ( 'NONE',  ( -40.51045226066063520, 7.589116544599141534, 60.22001867261916885 ) ) ;
#31376 = CARTESIAN_POINT ( 'NONE',  ( 44.09250526802607340, 28.05621246473836905, 46.89322480343881949 ) ) ;
#31377 = AXIS2_PLACEMENT_3D ( 'NONE', #28281, #20724, #18721 ) ;
#31378 = CONICAL_SURFACE ( 'NONE', #29282, 1.003191532947550701, 0.7853981633974447263 ) ;
#31379 = CIRCLE ( 'NONE', #16154, 0.1250000000000001110 ) ;
#31380 = CARTESIAN_POINT ( 'NONE',  ( -40.99469220063296859, 10.73619040060270002, 57.17865484131924347 ) ) ;
#31381 = VECTOR ( 'NONE', #13493, 1000.000000000000000 ) ;
#31382 = AXIS2_PLACEMENT_3D ( 'NONE', #11189, #28915, #8877 ) ;
#31383 = ORIENTED_EDGE ( 'NONE', *, *, #17705, .F. ) ;
#31384 = DIRECTION ( 'NONE',  ( -1.101824276508909887E-16, 1.000000000000000000, -0.000000000000000000 ) ) ;
#31385 = CARTESIAN_POINT ( 'NONE',  ( 52.07598464021349116, -5.935454078358230134, -13.51145360256171557 ) ) ;
#31386 = CARTESIAN_POINT ( 'NONE',  ( 33.46699938050304013, 30.71183152705961916, 47.04930799450051637 ) ) ;
#31387 = CARTESIAN_POINT ( 'NONE',  ( 46.99218062947583974, 25.80286309983299375, 49.08406571254116102 ) ) ;
#31388 = ADVANCED_FACE ( 'NONE', ( #22860 ), #22367, .T. ) ;
#31389 = ORIENTED_EDGE ( 'NONE', *, *, #6346, .F. ) ;
#31390 = EDGE_CURVE ( 'NONE', #22149, #27481, #9622, .T. ) ;
#31391 = EDGE_CURVE ( 'NONE', #12749, #1400, #10160, .T. ) ;
#31392 = EDGE_CURVE ( 'NONE', #21311, #26286, #4380, .T. ) ;
#31393 = DIRECTION ( 'NONE',  ( -0.8746197071393877476, 0.4848096202463514359, 0.000000000000000000 ) ) ;
#31394 = FACE_OUTER_BOUND ( 'NONE', #24955, .T. ) ;
#31395 = EDGE_CURVE ( 'NONE', #2133, #3392, #7453, .T. ) ;
#31396 = CARTESIAN_POINT ( 'NONE',  ( -42.48178708409979265, 14.60617548783703690, 60.54930799450051637 ) ) ;
#31397 = AXIS2_PLACEMENT_3D ( 'NONE', #3080, #634, #8341 ) ;
#31398 = AXIS2_PLACEMENT_3D ( 'NONE', #6144, #29118, #21226 ) ;
#31399 = CARTESIAN_POINT ( 'NONE',  ( 48.23388202445966755, 26.82822092656774515, 49.27628909396054979 ) ) ;
#31400 = AXIS2_PLACEMENT_3D ( 'NONE', #10837, #13614, #18677 ) ;
#31401 = DIRECTION ( 'NONE',  ( -1.000000000000000000, 0.000000000000000000, 0.000000000000000000 ) ) ;
#31402 = CARTESIAN_POINT ( 'NONE',  ( 21.09785597605720753, -14.03534765547855656, 106.8589376701495581 ) ) ;
#31403 = CARTESIAN_POINT ( 'NONE',  ( 21.09785597605720753, -5.098646251524523443, 47.04930799450052348 ) ) ;
#31404 = ORIENTED_EDGE ( 'NONE', *, *, #18843, .F. ) ;
#31405 = DIRECTION ( 'NONE',  ( 0.2756373558169958327, -0.9612616959383198934, 0.000000000000000000 ) ) ;
#31406 = CARTESIAN_POINT ( 'NONE',  ( 49.49063479933183629, 26.61291119454915233, 47.17357720316391578 ) ) ;
#31407 = CARTESIAN_POINT ( 'NONE',  ( 81.60489042199095877, -5.935454337261173663, 78.02742988628502019 ) ) ;
#31408 = DIRECTION ( 'NONE',  ( -1.000000000000000000, -1.101824276508909887E-16, 0.000000000000000000 ) ) ;
#31409 = AXIS2_PLACEMENT_3D ( 'NONE', #16386, #21461, #15910 ) ;
#31410 = LINE ( 'NONE', #21863, #19426 ) ;
#31411 = EDGE_LOOP ( 'NONE', ( #23120, #13592, #30195, #4657 ) ) ;
#31412 = CYLINDRICAL_SURFACE ( 'NONE', #15577, 0.1000000000000007272 ) ;
#31413 = AXIS2_PLACEMENT_3D ( 'NONE', #27745, #10517, #3101 ) ;
#31414 = CARTESIAN_POINT ( 'NONE',  ( -45.06166779280744095, -5.721341737285086992, 40.94964444931001424 ) ) ;
#31415 = LINE ( 'NONE', #16785, #27778 ) ;
#31416 = EDGE_LOOP ( 'NONE', ( #5177, #4839, #3653, #22283 ) ) ;
#31417 = CARTESIAN_POINT ( 'NONE',  ( -40.02540636251513462, 2.839176264122873050, 35.84930799450052064 ) ) ;
#31418 = DIRECTION ( 'NONE',  ( -1.000000000000000000, -1.101824276508909764E-16, 0.000000000000000000 ) ) ;
#31419 = DIRECTION ( 'NONE',  ( -1.000000000000000000, 0.000000000000000000, 0.000000000000000000 ) ) ;
#31420 = CARTESIAN_POINT ( 'NONE',  ( 21.09992658989238734, 31.59164230456639544, 47.04930799450051637 ) ) ;
#31421 = ORIENTED_EDGE ( 'NONE', *, *, #30990, .T. ) ;
#31422 = CARTESIAN_POINT ( 'NONE',  ( 47.82620649179236949, 29.44832000455004462, 49.14791808304156717 ) ) ;
#31423 = ORIENTED_EDGE ( 'NONE', *, *, #27316, .T. ) ;
#31424 = EDGE_CURVE ( 'NONE', #23543, #22288, #17280, .T. ) ;
#31425 = AXIS2_PLACEMENT_3D ( 'NONE', #6810, #8945, #16969 ) ;
#31426 = AXIS2_PLACEMENT_3D ( 'NONE', #2715, #23381, #7649 ) ;
#31427 = VERTEX_POINT ( 'NONE', #4654 ) ;
#31428 = AXIS2_PLACEMENT_3D ( 'NONE', #31373, #29398, #24303 ) ;
#31429 = AXIS2_PLACEMENT_3D ( 'NONE', #17610, #5314, #217 ) ;
#31430 = EDGE_CURVE ( 'NONE', #16793, #9226, #23258, .T. ) ;
#31431 = EDGE_CURVE ( 'NONE', #13965, #14963, #31137, .T. ) ;
#31432 = EDGE_CURVE ( 'NONE', #3559, #11753, #5964, .T. ) ;
#31433 = AXIS2_PLACEMENT_3D ( 'NONE', #140, #10482, #8020 ) ;
#31434 = DIRECTION ( 'NONE',  ( 0.000000000000000000, -1.000000000000000000, 0.000000000000000000 ) ) ;
#31435 = FACE_OUTER_BOUND ( 'NONE', #7530, .T. ) ;
#31436 = DIRECTION ( 'NONE',  ( 0.000000000000000000, 1.517883041479704827E-15, -1.000000000000000000 ) ) ;
#31437 = ADVANCED_FACE ( 'NONE', ( #27628 ), #22702, .F. ) ;
#31438 = AXIS2_PLACEMENT_3D ( 'NONE', #27828, #404, #30291 ) ;
#31439 = ORIENTED_EDGE ( 'NONE', *, *, #22901, .F. ) ;
#31440 = DIRECTION ( 'NONE',  ( 0.000000000000000000, -0.000000000000000000, -1.000000000000000000 ) ) ;
#31441 = ORIENTED_EDGE ( 'NONE', *, *, #1580, .T. ) ;
#31442 = CARTESIAN_POINT ( 'NONE',  ( 49.65101332465108186, 24.93501648625822398, 46.52608845888364186 ) ) ;
#31443 = PRESENTATION_STYLE_ASSIGNMENT (( #21400 ) ) ;
#31444 = ORIENTED_EDGE ( 'NONE', *, *, #27757, .F. ) ;
#31445 = CARTESIAN_POINT ( 'NONE',  ( 33.72499318558949000, 38.56284415653841791, 47.04930799450051637 ) ) ;
#31446 = CARTESIAN_POINT ( 'NONE',  ( 21.09992658989239089, 30.59143805560860585, 47.04930799450051637 ) ) ;
#31447 = DIRECTION ( 'NONE',  ( 0.4848096202463405002, 0.8746197071393938538, 0.000000000000000000 ) ) ;
#31448 = AXIS2_PLACEMENT_3D ( 'NONE', #9439, #4672, #9925 ) ;
#31449 = ORIENTED_EDGE ( 'NONE', *, *, #26386, .F. ) ;
#31450 = CARTESIAN_POINT ( 'NONE',  ( 21.09785597605720753, 13.86454579224779948, 47.04930799450052348 ) ) ;
#31451 = DIRECTION ( 'NONE',  ( -1.000000000000000000, 0.000000000000000000, 0.000000000000000000 ) ) ;
#31452 = DIRECTION ( 'NONE',  ( -6.722685822323786766E-17, 1.000000000000000000, -0.000000000000000000 ) ) ;
#31453 = CARTESIAN_POINT ( 'NONE',  ( 8.474859994195281132, 38.56284415653841791, 47.04930799450051637 ) ) ;
#31454 = DIRECTION ( 'NONE',  ( -1.000000000000000000, 0.000000000000000000, 0.000000000000000000 ) ) ;
#31455 = EDGE_LOOP ( 'NONE', ( #15265, #21303, #25879, #22698 ) ) ;
#31456 = CARTESIAN_POINT ( 'NONE',  ( -40.07989290236490376, 6.890692649785586710, 34.91305977274481620 ) ) ;
#31457 = DIRECTION ( 'NONE',  ( -1.000000000000000000, 0.000000000000000000, 0.000000000000000000 ) ) ;
#31458 = ORIENTED_EDGE ( 'NONE', *, *, #20879, .F. ) ;
#31459 = CARTESIAN_POINT ( 'NONE',  ( 21.09992658989238734, 38.56284415653841791, 47.04930799450051637 ) ) ;
#31460 = AXIS2_PLACEMENT_3D ( 'NONE', #1795, #1304, #6564 ) ;
#31461 = CARTESIAN_POINT ( 'NONE',  ( -41.94956971822180947, 3.905757428664829334, 45.14930799450051779 ) ) ;
#31462 = ORIENTED_EDGE ( 'NONE', *, *, #1926, .T. ) ;
#31463 = ORIENTED_EDGE ( 'NONE', *, *, #9160, .T. ) ;
#31464 = AXIS2_PLACEMENT_3D ( 'NONE', #23812, #30897, #18713 ) ;
#31465 = EDGE_CURVE ( 'NONE', #23296, #1152, #28459, .T. ) ;
#31466 = EDGE_CURVE ( 'NONE', #13013, #11449, #5454, .T. ) ;
#31467 = ORIENTED_EDGE ( 'NONE', *, *, #18523, .F. ) ;
#31468 = AXIS2_PLACEMENT_3D ( 'NONE', #15608, #28256, #351 ) ;
#31469 = CARTESIAN_POINT ( 'NONE',  ( 21.09785597605719332, 40.56454579224779877, 47.04930799450051637 ) ) ;
#31470 = EDGE_CURVE ( 'NONE', #18870, #23253, #30900, .T. ) ;
#31471 = AXIS2_PLACEMENT_3D ( 'NONE', #14597, #28003, #10289 ) ;
#31472 = EDGE_LOOP ( 'NONE', ( #26894, #29165 ) ) ;
#31473 = CARTESIAN_POINT ( 'NONE',  ( 21.09785597605720042, -52.14605111273580462, 47.04930799450051637 ) ) ;
#31474 = CARTESIAN_POINT ( 'NONE',  ( 21.09992658989238734, 38.56284415653841791, 47.04930799450051637 ) ) ;
#31475 = CIRCLE ( 'NONE', #20465, 31.50000000000000000 ) ;
#31476 = CARTESIAN_POINT ( 'NONE',  ( 45.38854177497844944, 28.36952976649964597, 45.94041160078741370 ) ) ;
#31477 = CIRCLE ( 'NONE', #10524, 0.1250000000000001110 ) ;
#31478 = AXIS2_PLACEMENT_3D ( 'NONE', #20675, #15274, #656 ) ;
#31479 = ORIENTED_EDGE ( 'NONE', *, *, #1777, .T. ) ;
#31480 = ORIENTED_EDGE ( 'NONE', *, *, #9907, .F. ) ;
#31481 = CARTESIAN_POINT ( 'NONE',  ( -8.048943652745618849, 7.198184577528760286, -3.649531620208970484 ) ) ;
#31482 = AXIS2_PLACEMENT_3D ( 'NONE', #6174, #18635, #25722 ) ;
#31483 = ORIENTED_EDGE ( 'NONE', *, *, #4706, .F. ) ;
#31484 = DIRECTION ( 'NONE',  ( 2.779292025043186357E-18, -1.288349127009862211E-17, 1.000000000000000000 ) ) ;
#31485 = DIRECTION ( 'NONE',  ( -1.101824276508909887E-16, 1.000000000000000000, -0.000000000000000000 ) ) ;
#31486 = CARTESIAN_POINT ( 'NONE',  ( -40.56019413908494187, 7.186695055020557277, 38.80167063144872230 ) ) ;
#31487 = CYLINDRICAL_SURFACE ( 'NONE', #12137, 12.36707279061065101 ) ;
#31488 = PLANE ( 'NONE',  #1181 ) ;
#31489 = CARTESIAN_POINT ( 'NONE',  ( 45.73035263060504718, 25.83954579807171115, 44.36855633853329550 ) ) ;
#31490 = CARTESIAN_POINT ( 'NONE',  ( -41.40774006177731081, 10.72547736613775626, 57.28220823191252720 ) ) ;
#31491 = CARTESIAN_POINT ( 'NONE',  ( -40.46271621608484281, 3.081581074246048768, 38.54930799450052348 ) ) ;
#31492 = ADVANCED_FACE ( 'NONE', ( #23505 ), #8414, .F. ) ;
#31493 = ORIENTED_EDGE ( 'NONE', *, *, #30550, .F. ) ;
#31494 = CARTESIAN_POINT ( 'NONE',  ( 21.09785597605719332, 17.36451738380053555, 47.04930799450051637 ) ) ;
#31495 = CARTESIAN_POINT ( 'NONE',  ( 21.09785597605720753, 13.86454579224779948, 47.04930799450052348 ) ) ;
#31496 = CIRCLE ( 'NONE', #26775, 0.1999999999999987899 ) ;
#31497 = CARTESIAN_POINT ( 'NONE',  ( -39.59792565122570096, 7.943629834091020747, 34.54930799450052348 ) ) ;
#31498 = EDGE_CURVE ( 'NONE', #12308, #7388, #25648, .T. ) ;
#31499 = DIRECTION ( 'NONE',  ( -7.588956326749211550E-18, 4.206627182996911684E-18, -1.000000000000000000 ) ) ;
#31500 = CARTESIAN_POINT ( 'NONE',  ( 21.09992658989238734, 38.56284415653841791, 47.04930799450051637 ) ) ;
#31501 = ORIENTED_EDGE ( 'NONE', *, *, #842, .T. ) ;
#31502 = DIRECTION ( 'NONE',  ( -0.8746197071393926326, 0.4848096202463430537, 8.676864087101709653E-18 ) ) ;
#31503 = VERTEX_POINT ( 'NONE', #18410 ) ;
#31504 = LINE ( 'NONE', #3762, #7378 ) ;
#31505 = DIRECTION ( 'NONE',  ( 0.000000000000000000, 0.000000000000000000, -1.000000000000000000 ) ) ;
#31506 = ADVANCED_FACE ( 'NONE', ( #18563 ), #28593, .F. ) ;
#31507 = EDGE_CURVE ( 'NONE', #25220, #663, #21151, .T. ) ;
#31508 = AXIS2_PLACEMENT_3D ( 'NONE', #4357, #21902, #4517 ) ;
#31509 = EDGE_CURVE ( 'NONE', #9808, #19261, #26127, .T. ) ;
#31510 = ORIENTED_EDGE ( 'NONE', *, *, #23456, .F. ) ;
#31511 = AXIS2_PLACEMENT_3D ( 'NONE', #2332, #29582, #14158 ) ;
#31512 = VECTOR ( 'NONE', #599, 1000.000000000000000 ) ;
#31513 = CIRCLE ( 'NONE', #29947, 12.62506659569710266 ) ;
#31514 =( BOUNDED_CURVE ( )  B_SPLINE_CURVE ( 2, ( #30151, #7661, #22251, #17654, #27673, #5194, #25218, #2730, #20923 ),
 .UNSPECIFIED., .F., .F. ) 
 B_SPLINE_CURVE_WITH_KNOTS ( ( 3, 2, 2, 2, 3 ),
 ( 0.1071428559815845449, 0.1190476190476190688, 0.1428571428571429047, 0.1666666666666666297, 0.1785714274101558585 ),
 .UNSPECIFIED. ) 
 CURVE ( )  GEOMETRIC_REPRESENTATION_ITEM ( )  RATIONAL_B_SPLINE_CURVE ( ( 0.9330127018922200755, 0.9330126953578161686, 1.000000000000000000, 0.8660254037844387076, 1.000000000000000000, 0.8660254037844387076, 1.000000000000000000, 0.9330127084266230941, 0.9330127018922200755 ) ) 
 REPRESENTATION_ITEM ( '' )  );
#31515 = ORIENTED_EDGE ( 'NONE', *, *, #23439, .F. ) ;
#31516 = DIRECTION ( 'NONE',  ( 0.000000000000000000, 0.000000000000000000, -1.000000000000000000 ) ) ;
#31517 = EDGE_CURVE ( 'NONE', #756, #9462, #18530, .T. ) ;
#31518 = LINE ( 'NONE', #13793, #18849 ) ;
#31519 = AXIS2_PLACEMENT_3D ( 'NONE', #32460, #19972, #2033 ) ;
#31520 = ORIENTED_EDGE ( 'NONE', *, *, #16257, .T. ) ;
#31521 = CARTESIAN_POINT ( 'NONE',  ( 47.09785597605719687, 24.86454579224779593, 47.04930799450078638 ) ) ;
#31522 = CARTESIAN_POINT ( 'NONE',  ( -35.89521036423793987, 10.88979515353705807, 41.81960461513401839 ) ) ;
#31523 = CARTESIAN_POINT ( 'NONE',  ( 72.46310410352296572, 9.702389020015065313, 20.34850893876554778 ) ) ;
#31524 = EDGE_LOOP ( 'NONE', ( #24300, #10679, #7130, #25258 ) ) ;
#31525 = ORIENTED_EDGE ( 'NONE', *, *, #18767, .T. ) ;
#31526 = AXIS2_PLACEMENT_3D ( 'NONE', #8314, #30969, #13089 ) ;
#31527 = FACE_OUTER_BOUND ( 'NONE', #3304, .T. ) ;
#31528 = CARTESIAN_POINT ( 'NONE',  ( 33.50134396954523908, 27.59164230456639544, 47.04930799450051637 ) ) ;
#31529 = AXIS2_PLACEMENT_3D ( 'NONE', #29801, #30287, #17639 ) ;
#31530 = DIRECTION ( 'NONE',  ( -0.000000000000000000, -1.000000000000000000, -0.000000000000000000 ) ) ;
#31531 = EDGE_CURVE ( 'NONE', #30980, #23798, #26040, .T. ) ;
#31532 = CIRCLE ( 'NONE', #27851, 0.1000000000000028644 ) ;
#31533 = DIRECTION ( 'NONE',  ( 1.000000000000000000, 0.000000000000000000, 0.000000000000000000 ) ) ;
#31534 = ORIENTED_EDGE ( 'NONE', *, *, #16072, .F. ) ;
#31535 = ORIENTED_EDGE ( 'NONE', *, *, #933, .T. ) ;
#31536 = DIRECTION ( 'NONE',  ( -1.000000000000000000, 0.000000000000000000, 0.000000000000000000 ) ) ;
#31537 = DIRECTION ( 'NONE',  ( 0.8746197071393926326, -0.4848096202463430537, -8.676864087101709653E-18 ) ) ;
#31538 = EDGE_CURVE ( 'NONE', #21064, #21045, #24301, .T. ) ;
#31539 = ORIENTED_EDGE ( 'NONE', *, *, #27488, .F. ) ;
#31540 = DIRECTION ( 'NONE',  ( -0.4544104193609905806, -5.611869858668448142E-17, -0.8907924397839087627 ) ) ;
#31541 = CARTESIAN_POINT ( 'NONE',  ( 64.96297466771235918, -13.74047052604243646, 8.573397087748993783 ) ) ;
#31542 = ORIENTED_EDGE ( 'NONE', *, *, #1932, .T. ) ;
#31543 = CARTESIAN_POINT ( 'NONE',  ( 21.09785597605719332, 25.56454579224779167, 70.54930799450050927 ) ) ;
#31544 = CARTESIAN_POINT ( 'NONE',  ( 46.96268396749378127, 28.93121246473836905, 49.65201805493727960 ) ) ;
#31545 = AXIS2_PLACEMENT_3D ( 'NONE', #26187, #28506, #1727 ) ;
#31546 = EDGE_CURVE ( 'NONE', #32110, #7248, #21180, .T. ) ;
#31547 = DIRECTION ( 'NONE',  ( -1.000000000000000000, 0.000000000000000000, 0.000000000000000000 ) ) ;
#31548 = ADVANCED_FACE ( 'NONE', ( #1334 ), #6914, .F. ) ;
#31549 = EDGE_LOOP ( 'NONE', ( #2530, #10846 ) ) ;
#31550 = AXIS2_PLACEMENT_3D ( 'NONE', #29299, #26349, #28818 ) ;
#31551 = AXIS2_PLACEMENT_3D ( 'NONE', #5502, #25517, #25835 ) ;
#31552 = CARTESIAN_POINT ( 'NONE',  ( 8.823509210239581790, 31.59164230456639544, 47.04930799450051637 ) ) ;
#31553 = FACE_OUTER_BOUND ( 'NONE', #5679, .T. ) ;
#31554 = DIRECTION ( 'NONE',  ( 0.000000000000000000, 0.000000000000000000, -1.000000000000000000 ) ) ;
#31555 = CARTESIAN_POINT ( 'NONE',  ( 46.99218062947583974, 25.10286309983299091, 49.08406571254116102 ) ) ;
#31556 = ORIENTED_EDGE ( 'NONE', *, *, #16887, .F. ) ;
#31557 = DIRECTION ( 'NONE',  ( 0.4114095458597723520, -0.6546536707079779749, -0.6341693441061513337 ) ) ;
#31558 = CARTESIAN_POINT ( 'NONE',  ( 8.732853799281738105, 29.71183152705961561, 47.04930799450051637 ) ) ;
#31559 = CIRCLE ( 'NONE', #16347, 1.899999999999999023 ) ;
#31560 = DIRECTION ( 'NONE',  ( -1.101824276508909887E-16, 1.000000000000000000, -0.000000000000000000 ) ) ;
#31561 = DIRECTION ( 'NONE',  ( -1.000000000000000000, 0.000000000000000000, 0.000000000000000000 ) ) ;
#31562 = CARTESIAN_POINT ( 'NONE',  ( 45.77813520618632737, 19.86454579224779948, 49.08359831045164157 ) ) ;
#31563 = CARTESIAN_POINT ( 'NONE',  ( -14.41812891119675122, -13.74047052604243646, 93.34357519277924098 ) ) ;
#31564 = LINE ( 'NONE', #9070, #8417 ) ;
#31565 = AXIS2_PLACEMENT_3D ( 'NONE', #15688, #25707, #910 ) ;
#31566 = FACE_OUTER_BOUND ( 'NONE', #31374, .T. ) ;
#31567 =( NAMED_UNIT ( * ) SI_UNIT ( $, .STERADIAN. ) SOLID_ANGLE_UNIT ( ) );
#31568 = ORIENTED_EDGE ( 'NONE', *, *, #19784, .T. ) ;
#31569 = CARTESIAN_POINT ( 'NONE',  ( 45.42945060211348363, 22.93328494799376216, 46.63886900051237916 ) ) ;
#31570 = CARTESIAN_POINT ( 'NONE',  ( 48.40186567930497574, 26.02957786121582373, 45.03923535223908203 ) ) ;
#31571 = CYLINDRICAL_SURFACE ( 'NONE', #24524, 2.500000000000002220 ) ;
#31572 = AXIS2_PLACEMENT_3D ( 'NONE', #19842, #1266, #10825 ) ;
#31573 = CARTESIAN_POINT ( 'NONE',  ( 21.09785597605719332, 77.37245976740706510, 47.04930799450051637 ) ) ;
#31574 = DIRECTION ( 'NONE',  ( -0.000000000000000000, -1.000000000000000000, -0.000000000000000000 ) ) ;
#31575 = ORIENTED_EDGE ( 'NONE', *, *, #17570, .F. ) ;
#31576 = AXIS2_PLACEMENT_3D ( 'NONE', #10152, #12943, #29850 ) ;
#31577 = CARTESIAN_POINT ( 'NONE',  ( -39.56501946919145496, -5.936124025396923187, 77.93580931442834014 ) ) ;
#31578 = CARTESIAN_POINT ( 'NONE',  ( 46.58637386172244277, 23.04411619146718238, 46.04663644226216945 ) ) ;
#31579 = DIRECTION ( 'NONE',  ( -0.4848096202463774151, -0.8746197071393733147, 0.000000000000000000 ) ) ;
#31580 = VERTEX_POINT ( 'NONE', #16748 ) ;
#31581 = DIRECTION ( 'NONE',  ( -0.2756373558169932236, 0.9612616959383205595, -1.479773560108267395E-16 ) ) ;
#31582 = DIRECTION ( 'NONE',  ( 1.234978253042719660E-16, -1.000000000000000000, -1.109335647967047851E-31 ) ) ;
#31583 = FACE_OUTER_BOUND ( 'NONE', #16554, .T. ) ;
#31584 = EDGE_CURVE ( 'NONE', #18455, #19824, #6748, .T. ) ;
#31585 = DIRECTION ( 'NONE',  ( 0.9612616959383313286, 0.2756373558169555871, 0.000000000000000000 ) ) ;
#31586 = ADVANCED_FACE ( 'NONE', ( #21339 ), #16915, .T. ) ;
#31587 = ORIENTED_EDGE ( 'NONE', *, *, #16516, .F. ) ;
#31588 = DIRECTION ( 'NONE',  ( 0.000000000000000000, 1.000000000000000000, -0.000000000000000000 ) ) ;
#31589 = VERTEX_POINT ( 'NONE', #19046 ) ;
#31590 = EDGE_LOOP ( 'NONE', ( #22760, #29792, #6223, #14554 ) ) ;
#31591 = VECTOR ( 'NONE', #24289, 1000.000000000000000 ) ;
#31592 = CIRCLE ( 'NONE', #9047, 0.09999999999999845124 ) ;
#31593 = VECTOR ( 'NONE', #19637, 1000.000000000000114 ) ;
#31594 = AXIS2_PLACEMENT_3D ( 'NONE', #4527, #21591, #9458 ) ;
#31595 = CARTESIAN_POINT ( 'NONE',  ( 21.09785597605720042, -17.03545420775220265, 47.04930799450051637 ) ) ;
#31596 = DIRECTION ( 'NONE',  ( 0.000000000000000000, 0.000000000000000000, -1.000000000000000000 ) ) ;
#31597 = CARTESIAN_POINT ( 'NONE',  ( 81.79977007715724824, -5.936747322758277434, 77.92211803829925998 ) ) ;
#31598 = EDGE_LOOP ( 'NONE', ( #6007, #24903, #30600, #4026 ) ) ;
#31599 = CARTESIAN_POINT ( 'NONE',  ( 33.72499318558949710, 31.34143805560860585, 47.04930799450051637 ) ) ;
#31600 = ORIENTED_EDGE ( 'NONE', *, *, #30945, .F. ) ;
#31601 = CARTESIAN_POINT ( 'NONE',  ( 21.09785597605719332, 28.56454579224779877, 47.04930799450051637 ) ) ;
#31602 = CARTESIAN_POINT ( 'NONE',  ( -41.63422246745999189, 11.51531537899137447, 57.04930799450051637 ) ) ;
#31603 = ORIENTED_EDGE ( 'NONE', *, *, #7350, .T. ) ;
#31604 = FACE_OUTER_BOUND ( 'NONE', #9945, .T. ) ;
#31605 = CARTESIAN_POINT ( 'NONE',  ( 64.59785597605720397, -5.098646251524523443, 47.04930799450051637 ) ) ;
#31606 = DIRECTION ( 'NONE',  ( 6.722685822323786766E-17, -1.000000000000000000, 0.000000000000000000 ) ) ;
#31607 = ORIENTED_EDGE ( 'NONE', *, *, #9759, .F. ) ;
#31608 = CARTESIAN_POINT ( 'NONE',  ( 46.86492225703624825, 23.03451764446789696, 45.86279067552989375 ) ) ;
#31609 = LINE ( 'NONE', #30973, #27341 ) ;
#31610 = DIRECTION ( 'NONE',  ( 0.000000000000000000, 0.000000000000000000, 1.000000000000000000 ) ) ;
#31611 = AXIS2_PLACEMENT_3D ( 'NONE', #15064, #2428, #22272 ) ;
#31612 =( NAMED_UNIT ( * ) PLANE_ANGLE_UNIT ( ) SI_UNIT ( $, .RADIAN. ) );
#31613 = VERTEX_POINT ( 'NONE', #1172 ) ;
#31614 = FACE_OUTER_BOUND ( 'NONE', #26984, .T. ) ;
#31615 = CARTESIAN_POINT ( 'NONE',  ( 8.732853799281734553, 38.56284415653841791, 47.04930799450051637 ) ) ;
#31616 = CIRCLE ( 'NONE', #26372, 0.1249999999999983763 ) ;
#31617 = ORIENTED_EDGE ( 'NONE', *, *, #10614, .F. ) ;
#31618 = DIRECTION ( 'NONE',  ( -1.101824276508909887E-16, 1.000000000000000000, -0.000000000000000000 ) ) ;
#31619 = CARTESIAN_POINT ( 'NONE',  ( -42.38474149870877028, 15.25146566812707505, 38.54930799450052348 ) ) ;
#31620 = EDGE_CURVE ( 'NONE', #104, #29220, #13313, .T. ) ;
#31621 = EDGE_CURVE ( 'NONE', #14823, #32191, #25369, .T. ) ;
#31622 = ORIENTED_EDGE ( 'NONE', *, *, #24805, .F. ) ;
#31623 = EDGE_CURVE ( 'NONE', #17347, #2789, #31860, .T. ) ;
#31624 = VECTOR ( 'NONE', #5024, 1000.000000000000000 ) ;
#31625 = AXIS2_PLACEMENT_3D ( 'NONE', #21456, #18828, #13609 ) ;
#31626 = VERTEX_POINT ( 'NONE', #18715 ) ;
#31627 = EDGE_CURVE ( 'NONE', #4349, #5375, #11355, .T. ) ;
#31628 = EDGE_CURVE ( 'NONE', #16708, #9505, #29564, .T. ) ;
#31629 = EDGE_LOOP ( 'NONE', ( #5019, #15533, #30337, #10894 ) ) ;
#31630 = TOROIDAL_SURFACE ( 'NONE', #29531, 12.40141737965281088, 0.1249999999999987788 ) ;
#31631 = CIRCLE ( 'NONE', #15913, 12.27641737965284108 ) ;
#31632 = B_SPLINE_CURVE_WITH_KNOTS ( 'NONE', 3,
 ( #10964, #23103, #3555, #23269, #25734, #3239, #13585, #13276, #8333, #621, #15715, #15886, #10651, #8180, #18171, #20955, #5882, #16035, #780, #28523, #20802, #3396, #28363, #23428, #935, #30821, #25890, #30987, #8497, #5332 ),
 .UNSPECIFIED., .F., .F.,
 ( 4, 2, 2, 2, 2, 2, 2, 2, 2, 2, 2, 2, 2, 2, 4 ),
 ( 0.000000000000000000, 0.001249755272498796928, 0.002499510544997593856, 0.003749265817496392952, 0.004999021089995192048, 0.007498531634992787638, 0.009998042179990382361, 0.01249755272498797795, 0.01374730799748676707, 0.01499706326998555272, 0.01562194090623493514, 0.01624681854248431756, 0.01749657381498308586, 0.01874632908748184723, 0.01999608435998061207 ),
 .UNSPECIFIED. ) ;
#31633 = DIRECTION ( 'NONE',  ( -0.000000000000000000, 1.000000000000000000, -0.000000000000000000 ) ) ;
#31634 = ORIENTED_EDGE ( 'NONE', *, *, #28648, .T. ) ;
#31635 = DIRECTION ( 'NONE',  ( -0.9612616959383200044, -0.2756373558169954996, 1.660411357259285896E-16 ) ) ;
#31636 = AXIS2_PLACEMENT_3D ( 'NONE', #21062, #21219, #23699 ) ;
#31637 = AXIS2_PLACEMENT_3D ( 'NONE', #800, #15902, #31003 ) ;
#31638 = CARTESIAN_POINT ( 'NONE',  ( -4.902144023942810236, 24.86454579224779948, 47.04930799450078638 ) ) ;
#31639 = AXIS2_PLACEMENT_3D ( 'NONE', #2836, #373, #29940 ) ;
#31640 = AXIS2_PLACEMENT_3D ( 'NONE', #3231, #23577, #26033 ) ;
#31641 = CARTESIAN_POINT ( 'NONE',  ( 21.09785597605719332, 43.56454579224774193, 17.04930799450051637 ) ) ;
#31642 = CARTESIAN_POINT ( 'NONE',  ( 45.28286642839709231, 27.08619643316632519, 47.97516931882780966 ) ) ;
#31643 = EDGE_CURVE ( 'NONE', #12487, #27983, #31703, .T. ) ;
#31644 = VERTEX_POINT ( 'NONE', #1492 ) ;
#31645 = CARTESIAN_POINT ( 'NONE',  ( -38.57070939289658895, -5.937181781424613725, 77.94502167843351970 ) ) ;
#31646 = EDGE_LOOP ( 'NONE', ( #495, #16936, #24929, #12371 ) ) ;
#31647 = CARTESIAN_POINT ( 'NONE',  ( -40.48129536610376533, 8.613360132207176889, 39.44930799450052206 ) ) ;
#31648 = EDGE_CURVE ( 'NONE', #5653, #3892, #198, .T. ) ;
#31649 = VERTEX_POINT ( 'NONE', #8887 ) ;
#31650 = CARTESIAN_POINT ( 'NONE',  ( -41.59221397235413775, 0.6853201964616114639, 42.04930799450051637 ) ) ;
#31651 = DIRECTION ( 'NONE',  ( 1.000000000000000000, 0.000000000000000000, 0.000000000000000000 ) ) ;
#31652 = CARTESIAN_POINT ( 'NONE',  ( -40.61337426079425228, 6.957937756952573771, 39.01901553589728167 ) ) ;
#31653 = CYLINDRICAL_SURFACE ( 'NONE', #22817, 13.00178401536290806 ) ;
#31654 = CARTESIAN_POINT ( 'NONE',  ( -40.52669582637187773, 7.652910973922034010, 60.15421819779514578 ) ) ;
#31655 = CARTESIAN_POINT ( 'NONE',  ( 44.77625694075215534, 26.01454579807171186, 48.23360063142255427 ) ) ;
#31656 = CARTESIAN_POINT ( 'NONE',  ( 47.02134891529708938, 22.98765316579146756, 48.52243470084199117 ) ) ;
#31657 = DIRECTION ( 'NONE',  ( 0.4544104193609903586, 0.000000000000000000, 0.8907924397839087627 ) ) ;
#31658 = ORIENTED_EDGE ( 'NONE', *, *, #29081, .T. ) ;
#31659 = DIRECTION ( 'NONE',  ( -0.3958453973320084640, -0.7141240004913232964, 0.5773502691896251759 ) ) ;
#31660 = CARTESIAN_POINT ( 'NONE',  ( 21.09992658989239089, 25.21664230456640254, 47.04930799450051637 ) ) ;
#31661 = DIRECTION ( 'NONE',  ( 0.000000000000000000, -1.000000000000000000, 0.000000000000000000 ) ) ;
#31662 = FACE_OUTER_BOUND ( 'NONE', #4291, .T. ) ;
#31663 = DIRECTION ( 'NONE',  ( -1.000000000000000000, 0.000000000000000000, 0.000000000000000000 ) ) ;
#31664 = ORIENTED_EDGE ( 'NONE', *, *, #8023, .F. ) ;
#31665 = FACE_OUTER_BOUND ( 'NONE', #21584, .T. ) ;
#31666 = ORIENTED_EDGE ( 'NONE', *, *, #29805, .T. ) ;
#31667 = CARTESIAN_POINT ( 'NONE',  ( 21.09992658989239089, 27.84164230456639544, 47.04930799450051637 ) ) ;
#31668 = EDGE_CURVE ( 'NONE', #6508, #5510, #14357, .T. ) ;
#31669 = ORIENTED_EDGE ( 'NONE', *, *, #10821, .F. ) ;
#31670 = ORIENTED_EDGE ( 'NONE', *, *, #8586, .F. ) ;
#31671 = ADVANCED_FACE ( 'NONE', ( #28923 ), #26446, .T. ) ;
#31672 = FACE_BOUND ( 'NONE', #2847, .T. ) ;
#31673 = DIRECTION ( 'NONE',  ( -0.3958453973319808195, -0.7141240004913296247, -0.5773502691896363892 ) ) ;
#31674 = DIRECTION ( 'NONE',  ( -0.000000000000000000, 1.000000000000000000, 0.000000000000000000 ) ) ;
#31675 = EDGE_CURVE ( 'NONE', #5398, #3842, #9548, .T. ) ;
#31676 = ORIENTED_EDGE ( 'NONE', *, *, #22568, .F. ) ;
#31677 = TOROIDAL_SURFACE ( 'NONE', #234, 54.10000000000000142, 0.1999999999999993727 ) ;
#31678 = CARTESIAN_POINT ( 'NONE',  ( -40.05987053574653345, 7.506472619680471858, 34.64930799450051779 ) ) ;
#31679 = FACE_OUTER_BOUND ( 'NONE', #966, .T. ) ;
#31680 = CARTESIAN_POINT ( 'NONE',  ( 74.49868417184303837, 1.147918989839205040, 14.32049971022470558 ) ) ;
#31681 = AXIS2_PLACEMENT_3D ( 'NONE', #9394, #19554, #25862 ) ;
#31682 = EDGE_CURVE ( 'NONE', #14178, #11078, #712, .T. ) ;
#31683 = EDGE_LOOP ( 'NONE', ( #12696, #9292, #12579, #10111 ) ) ;
#31684 = AXIS2_PLACEMENT_3D ( 'NONE', #6282, #4137, #31561 ) ;
#31685 = EDGE_CURVE ( 'NONE', #1229, #12851, #10238, .T. ) ;
#31686 = ORIENTED_EDGE ( 'NONE', *, *, #10285, .F. ) ;
#31687 = AXIS2_PLACEMENT_3D ( 'NONE', #14314, #11849, #24313 ) ;
#31688 = FACE_OUTER_BOUND ( 'NONE', #18290, .T. ) ;
#31689 = FACE_OUTER_BOUND ( 'NONE', #29173, .T. ) ;
#31690 = CARTESIAN_POINT ( 'NONE',  ( 21.09785597605719687, 42.30003263981368633, 17.04930799450051637 ) ) ;
#31691 = ORIENTED_EDGE ( 'NONE', *, *, #10669, .T. ) ;
#31692 = ORIENTED_EDGE ( 'NONE', *, *, #13470, .T. ) ;
#31693 = DIRECTION ( 'NONE',  ( -1.000000000000000000, 0.000000000000000000, 0.000000000000000000 ) ) ;
#31694 = DIRECTION ( 'NONE',  ( 2.779292025043186357E-18, -1.288349127009862211E-17, 1.000000000000000000 ) ) ;
#31695 = DIRECTION ( 'NONE',  ( 0.8746197071393926326, -0.4848096202463430537, -8.676864087101709653E-18 ) ) ;
#31696 = ORIENTED_EDGE ( 'NONE', *, *, #13621, .F. ) ;
#31697 = CARTESIAN_POINT ( 'NONE',  ( -11.80969419479644777, -4.922489993312313850, -10.15873547626677365 ) ) ;
#31698 = CARTESIAN_POINT ( 'NONE',  ( 71.62639656063521443, -13.74047052604243824, 76.22825493111783146 ) ) ;
#31699 = EDGE_LOOP ( 'NONE', ( #1307, #7226, #3546, #27292 ) ) ;
#31700 = CARTESIAN_POINT ( 'NONE',  ( 21.09785597605719332, 17.16451738380053627, 34.56516646732340092 ) ) ;
#31701 = DIRECTION ( 'NONE',  ( 1.000000000000000000, 0.000000000000000000, 0.000000000000000000 ) ) ;
#31702 = EDGE_CURVE ( 'NONE', #15339, #18438, #28039, .T. ) ;
#31703 = LINE ( 'NONE', #9214, #1755 ) ;
#31704 = AXIS2_PLACEMENT_3D ( 'NONE', #17744, #4628, #4796 ) ;
#31705 = AXIS2_PLACEMENT_3D ( 'NONE', #24242, #6686, #7013 ) ;
#31706 = TOROIDAL_SURFACE ( 'NONE', #11250, 12.40141737965279667, 0.1249999999999991951 ) ;
#31707 = CIRCLE ( 'NONE', #21733, 12.27641737965280200 ) ;
#31708 = ORIENTED_EDGE ( 'NONE', *, *, #31682, .F. ) ;
#31709 = PLANE ( 'NONE',  #1289 ) ;
#31710 = EDGE_CURVE ( 'NONE', #11885, #14867, #24889, .T. ) ;
#31711 = LINE ( 'NONE', #4616, #2865 ) ;
#31712 = CARTESIAN_POINT ( 'NONE',  ( 21.09785597605720042, -9.935454207752199451, 115.0493079945004951 ) ) ;
#31713 = CARTESIAN_POINT ( 'NONE',  ( 49.49063479933183629, 29.49951373492758933, 47.17357720316391578 ) ) ;
#31714 = ORIENTED_EDGE ( 'NONE', *, *, #19565, .T. ) ;
#31715 = CARTESIAN_POINT ( 'NONE',  ( 8.732853799281731000, 28.72145308207318237, 47.04930799450051637 ) ) ;
#31716 = DIRECTION ( 'NONE',  ( 1.188208965918165239E-16, 1.880121038077813132E-16, 1.000000000000000000 ) ) ;
#31717 = DIRECTION ( 'NONE',  ( 0.2756373558169931126, -0.9612616959383206705, 1.479773560108267642E-16 ) ) ;
#31718 = ADVANCED_FACE ( 'NONE', ( #12169 ), #2477, .T. ) ;
#31719 = CARTESIAN_POINT ( 'NONE',  ( 21.09785597605720397, -19.93545420775220123, -37.25069200549950210 ) ) ;
#31720 = EDGE_CURVE ( 'NONE', #19781, #28214, #23319, .T. ) ;
#31721 = DIRECTION ( 'NONE',  ( -1.101824276508909887E-16, 1.000000000000000000, -0.000000000000000000 ) ) ;
#31722 = CARTESIAN_POINT ( 'NONE',  ( 21.09785597605719332, -13.74048473023143835, 105.2732083928529221 ) ) ;
#31723 = CYLINDRICAL_SURFACE ( 'NONE', #20987, 1.199999999999999734 ) ;
#31724 = AXIS2_PLACEMENT_3D ( 'NONE', #14770, #29703, #19513 ) ;
#31725 = DIRECTION ( 'NONE',  ( 0.000000000000000000, 0.000000000000000000, -1.000000000000000000 ) ) ;
#31726 = AXIS2_PLACEMENT_3D ( 'NONE', #18701, #16250, #14124 ) ;
#31727 = VERTEX_POINT ( 'NONE', #9866 ) ;
#31728 = DIRECTION ( 'NONE',  ( -1.101824276508909887E-16, 1.000000000000000000, -0.000000000000000000 ) ) ;
#31729 = CIRCLE ( 'NONE', #288, 66.44011198581388555 ) ;
#31730 = CIRCLE ( 'NONE', #17575, 12.36707279061065279 ) ;
#31731 = CARTESIAN_POINT ( 'NONE',  ( 47.25393916711946218, 25.08121246473836763, 44.04395728646968422 ) ) ;
#31732 = CARTESIAN_POINT ( 'NONE',  ( -30.88361648749964772, 11.92558985988973141, 26.60346110398183583 ) ) ;
#31733 = TOROIDAL_SURFACE ( 'NONE', #19671, 12.61792373059861028, 0.1250000000000006106 ) ;
#31734 = CARTESIAN_POINT ( 'NONE',  ( 46.55854765242723659, 26.44696019071911053, 44.51792966461573542 ) ) ;
#31735 = ORIENTED_EDGE ( 'NONE', *, *, #16585, .F. ) ;
#31736 = DIRECTION ( 'NONE',  ( -1.000000000000000000, 0.000000000000000000, 0.000000000000000000 ) ) ;
#31737 = CARTESIAN_POINT ( 'NONE',  ( -44.16105795751995799, -3.935454207752190126, 42.04930799450051637 ) ) ;
#31738 = CARTESIAN_POINT ( 'NONE',  ( -40.11286833322908052, 2.887657226147509970, 55.84930799450052064 ) ) ;
#31739 = VERTEX_POINT ( 'NONE', #21996 ) ;
#31740 = VERTEX_POINT ( 'NONE', #17405 ) ;
#31741 = DIRECTION ( 'NONE',  ( -1.000000000000000000, -1.101824276508909887E-16, 0.000000000000000000 ) ) ;
#31742 = FACE_OUTER_BOUND ( 'NONE', #6573, .T. ) ;
#31743 = DIRECTION ( 'NONE',  ( -1.224646799147353207E-16, -1.349345573449484691E-32, 1.000000000000000000 ) ) ;
#31744 = CARTESIAN_POINT ( 'NONE',  ( 46.90849534498374140, 22.91413368675619111, 45.25622507561872965 ) ) ;
#31745 = VERTEX_POINT ( 'NONE', #24634 ) ;
#31746 = CARTESIAN_POINT ( 'NONE',  ( -40.59290689585611744, 7.518854022824533523, 60.12740069859619751 ) ) ;
#31747 = ORIENTED_EDGE ( 'NONE', *, *, #7127, .T. ) ;
#31748 = ORIENTED_EDGE ( 'NONE', *, *, #9852, .F. ) ;
#31749 = ADVANCED_FACE ( 'NONE', ( #27427 ), #31706, .T. ) ;
#31750 = CARTESIAN_POINT ( 'NONE',  ( -42.37913764077812573, 15.23192269303852875, 38.44930799450052206 ) ) ;
#31751 = AXIS2_PLACEMENT_3D ( 'NONE', #6455, #26628, #16454 ) ;
#31752 = COLOUR_RGB ( '',0.7921568627450980005, 0.8196078431372548767, 0.9333333333333333481 ) ;
#31753 = DIRECTION ( 'NONE',  ( -1.101824276508909887E-16, 1.000000000000000000, -0.000000000000000000 ) ) ;
#31754 = CARTESIAN_POINT ( 'NONE',  ( -31.82365885725337051, -0.03213146785430506802, 80.27334318690746784 ) ) ;
#31755 = FACE_OUTER_BOUND ( 'NONE', #29949, .T. ) ;
#31756 = ADVANCED_FACE ( 'NONE', ( #22167 ), #14957, .T. ) ;
#31757 = VECTOR ( 'NONE', #14112, 1000.000000000000000 ) ;
#31758 = ORIENTED_EDGE ( 'NONE', *, *, #22831, .F. ) ;
#31759 = DIRECTION ( 'NONE',  ( 0.000000000000000000, -1.000000000000000000, 0.000000000000000000 ) ) ;
#31760 = VERTEX_POINT ( 'NONE', #17725 ) ;
#31761 = DIRECTION ( 'NONE',  ( -1.000000000000000000, 0.000000000000000000, 0.000000000000000000 ) ) ;
#31762 = DIRECTION ( 'NONE',  ( 0.8746197071393926326, -0.4848096202463430537, -8.676864087101709653E-18 ) ) ;
#31763 = DIRECTION ( 'NONE',  ( -1.000000000000000000, 0.000000000000000000, 0.000000000000000000 ) ) ;
#31764 = ORIENTED_EDGE ( 'NONE', *, *, #7256, .F. ) ;
#31765 = DIRECTION ( 'NONE',  ( -1.000000000000000000, -1.101824276508909887E-16, 0.000000000000000000 ) ) ;
#31766 = CARTESIAN_POINT ( 'NONE',  ( 8.732853799281734553, 29.22145308207318237, 47.04930799450051637 ) ) ;
#31767 = DIRECTION ( 'NONE',  ( -0.2756373558170034377, 0.9612616959383176729, -3.701728707981190596E-16 ) ) ;
#31768 = DIRECTION ( 'NONE',  ( -1.000000000000000000, 0.000000000000000000, 0.000000000000000000 ) ) ;
#31769 = CARTESIAN_POINT ( 'NONE',  ( 48.35473289974373756, 19.96454579224779380, 45.11188864597615833 ) ) ;
#31770 = CARTESIAN_POINT ( 'NONE',  ( -40.12057988072736947, 7.355395738388389226, 35.24232147887364874 ) ) ;
#31771 = CARTESIAN_POINT ( 'NONE',  ( 21.09992658989239089, 28.47145308207318237, 47.04930799450051637 ) ) ;
#31772 = EDGE_LOOP ( 'NONE', ( #996, #1256, #19146, #12069 ) ) ;
#31773 = CARTESIAN_POINT ( 'NONE',  ( 21.09785597605721108, -52.14605111273580462, 125.5493079945005093 ) ) ;
#31774 = ORIENTED_EDGE ( 'NONE', *, *, #18415, .T. ) ;
#31775 = CARTESIAN_POINT ( 'NONE',  ( -44.31161278331510545, -5.876499408311634198, 40.60422303027608848 ) ) ;
#31776 = VECTOR ( 'NONE', #32497, 1000.000000000000000 ) ;
#31777 = CARTESIAN_POINT ( 'NONE',  ( 21.09785597605719332, 25.76454579224776964, 15.54930799450051460 ) ) ;
#31778 = ORIENTED_EDGE ( 'NONE', *, *, #782, .T. ) ;
#31779 = ORIENTED_EDGE ( 'NONE', *, *, #32139, .T. ) ;
#31780 = PRODUCT_DEFINITION ( 'UNKNOWN', '', #26538, #18646 ) ;
#31781 = AXIS2_PLACEMENT_3D ( 'NONE', #4011, #31434, #16317 ) ;
#31782 = ORIENTED_EDGE ( 'NONE', *, *, #6405, .F. ) ;
#31783 = CARTESIAN_POINT ( 'NONE',  ( 64.09785597605720397, -5.098646251524523443, 47.04930799450051637 ) ) ;
#31784 = AXIS2_PLACEMENT_3D ( 'NONE', #23134, #2943, #650 ) ;
#31785 = PRODUCT_DEFINITION_FORMATION_WITH_SPECIFIED_SOURCE ( 'ANY', '', #19779, .NOT_KNOWN. ) ;
#31786 = ADVANCED_FACE ( 'NONE', ( #14798 ), #20028, .F. ) ;
#31787 = ORIENTED_EDGE ( 'NONE', *, *, #10627, .F. ) ;
#31788 = ORIENTED_EDGE ( 'NONE', *, *, #14679, .T. ) ;
#31789 = DIRECTION ( 'NONE',  ( -0.8746197071393926326, 0.4848096202463430537, 8.676864087101709653E-18 ) ) ;
#31790 = EDGE_CURVE ( 'NONE', #8764, #29601, #17551, .T. ) ;
#31791 = DIRECTION ( 'NONE',  ( -0.8746197071393790878, 0.4848096202463673676, 1.277302113040196197E-17 ) ) ;
#31792 = ADVANCED_FACE ( 'NONE', ( #12004 ), #22485, .F. ) ;
#31793 = DIRECTION ( 'NONE',  ( 0.000000000000000000, 0.000000000000000000, -1.000000000000000000 ) ) ;
#31794 = CARTESIAN_POINT ( 'NONE',  ( 33.46699938050302592, 31.47145308207317882, 47.04930799450050927 ) ) ;
#31795 = EDGE_CURVE ( 'NONE', #5664, #21721, #27094, .T. ) ;
#31796 = CARTESIAN_POINT ( 'NONE',  ( 48.91284552371730143, 27.43619643316631596, 46.12344667017377020 ) ) ;
#31797 = ORIENTED_EDGE ( 'NONE', *, *, #21858, .T. ) ;
#31798 = DIRECTION ( 'NONE',  ( 1.000000000000000000, 0.000000000000000000, 0.000000000000000000 ) ) ;
#31799 = EDGE_LOOP ( 'NONE', ( #277, #24104, #15875, #11924 ) ) ;
#31800 = CARTESIAN_POINT ( 'NONE',  ( -12.61912916467185042, -3.025068871688601391, -7.519726213196242348 ) ) ;
#31801 = ORIENTED_EDGE ( 'NONE', *, *, #7161, .F. ) ;
#31802 = LINE ( 'NONE', #10709, #3740 ) ;
#31803 = DIRECTION ( 'NONE',  ( -1.000000000000000000, -1.101824276508909887E-16, 0.000000000000000000 ) ) ;
#31804 = CIRCLE ( 'NONE', #3487, 12.62506659569710266 ) ;
#31805 = DIRECTION ( 'NONE',  ( -1.101824276508909887E-16, 1.000000000000000000, -0.000000000000000000 ) ) ;
#31806 = CARTESIAN_POINT ( 'NONE',  ( -40.68765130478452363, 6.801118111650202636, 39.35160066530853840 ) ) ;
#31807 = DIRECTION ( 'NONE',  ( 0.000000000000000000, -0.000000000000000000, 1.000000000000000000 ) ) ;
#31808 = CARTESIAN_POINT ( 'NONE',  ( 49.28428300279882990, 24.84787913140505111, 48.46772541801551171 ) ) ;
#31809 = CARTESIAN_POINT ( 'NONE',  ( -43.42682711710880739, 1.034448000281938285, 39.54930799450052348 ) ) ;
#31810 = DIRECTION ( 'NONE',  ( 0.4441739386572013948, 0.2110602665713099679, 0.8707256032141218460 ) ) ;
#31811 = ORIENTED_EDGE ( 'NONE', *, *, #23159, .F. ) ;
#31812 = DIRECTION ( 'NONE',  ( 0.000000000000000000, 1.000000000000000000, 0.000000000000000000 ) ) ;
#31813 = PLANE ( 'NONE',  #18216 ) ;
#31814 = DIRECTION ( 'NONE',  ( 0.2756373558169947779, -0.9612616959383200044, 0.000000000000000000 ) ) ;
#31815 = CARTESIAN_POINT ( 'NONE',  ( 47.83611419692596911, 23.04411657098542676, 46.18653938413861226 ) ) ;
#31816 = CARTESIAN_POINT ( 'NONE',  ( 21.09785597605719332, 25.76454579224781227, 35.04930799450050927 ) ) ;
#31817 = ORIENTED_EDGE ( 'NONE', *, *, #3033, .F. ) ;
#31818 = ORIENTED_EDGE ( 'NONE', *, *, #550, .F. ) ;
#31820 = EDGE_CURVE ( 'NONE', #13562, #14664, #19703, .T. ) ;
#31819 = CARTESIAN_POINT ( 'NONE',  ( -42.47434154250543514, 4.196643200812633978, 38.94930799450052206 ) ) ;
#31821 = CARTESIAN_POINT ( 'NONE',  ( 21.09992658989239089, 27.34184655352419568, 47.04930799450051637 ) ) ;
#31822 = EDGE_LOOP ( 'NONE', ( #9114, #30152, #16453, #12642 ) ) ;
#31823 = ADVANCED_FACE ( 'NONE', ( #7729 ), #29731, .F. ) ;
#31824 = ORIENTED_EDGE ( 'NONE', *, *, #15474, .F. ) ;
#31825 = DIRECTION ( 'NONE',  ( 2.779292025043186357E-18, -1.288349127009862211E-17, 1.000000000000000000 ) ) ;
#31826 = CARTESIAN_POINT ( 'NONE',  ( 49.52052953415556402, 8.310461108307681144, -12.70392589783158499 ) ) ;
#31827 = CARTESIAN_POINT ( 'NONE',  ( 8.474859994195286461, 24.59143805560860940, 47.04930799450051637 ) ) ;
#31828 = ORIENTED_EDGE ( 'NONE', *, *, #15635, .F. ) ;
#31829 = TOROIDAL_SURFACE ( 'NONE', #16106, 12.40141737965283397, 0.1249999999999992922 ) ;
#31830 = ADVANCED_FACE ( 'NONE', ( #22331 ), #25410, .T. ) ;
#31831 = DIRECTION ( 'NONE',  ( 0.9612616959383200044, 0.2756373558169954996, -1.660411357259285896E-16 ) ) ;
#31832 = EDGE_CURVE ( 'NONE', #5841, #31904, #5587, .T. ) ;
#31833 = AXIS2_PLACEMENT_3D ( 'NONE', #9381, #16436, #4294 ) ;
#31834 = SPHERICAL_SURFACE ( 'NONE', #6538, 0.1000000000000000056 ) ;
#31835 = CARTESIAN_POINT ( 'NONE',  ( 72.50786317273436055, 8.583949016299403212, 19.11078817837193711 ) ) ;
#31836 = EDGE_CURVE ( 'NONE', #15810, #30896, #13374, .T. ) ;
#31837 = ORIENTED_EDGE ( 'NONE', *, *, #256, .T. ) ;
#31838 = TOROIDAL_SURFACE ( 'NONE', #26069, 20.49999999999999645, 0.9999999999999974465 ) ;
#31839 = ORIENTED_EDGE ( 'NONE', *, *, #22990, .F. ) ;
#31840 =( NAMED_UNIT ( * ) PLANE_ANGLE_UNIT ( ) SI_UNIT ( $, .RADIAN. ) );
#31841 = VERTEX_POINT ( 'NONE', #10350 ) ;
#31842 = DIRECTION ( 'NONE',  ( 0.000000000000000000, 0.000000000000000000, 1.000000000000000000 ) ) ;
#31843 = DIRECTION ( 'NONE',  ( -1.000000000000000000, 0.000000000000000000, 0.000000000000000000 ) ) ;
#31844 = PRODUCT_DEFINITION_SHAPE ( 'NONE', 'NONE',  #32506 ) ;
#31845 = AXIS2_PLACEMENT_3D ( 'NONE', #4639, #11867, #12028 ) ;
#31846 = CARTESIAN_POINT ( 'NONE',  ( -45.71603902977910394, -5.927433539347818581, 40.25072284635503195 ) ) ;
#31847 = CARTESIAN_POINT ( 'NONE',  ( 0.000000000000000000, 0.000000000000000000, 0.000000000000000000 ) ) ;
#31848 = VERTEX_POINT ( 'NONE', #13145 ) ;
#31849 = ORIENTED_EDGE ( 'NONE', *, *, #7415, .T. ) ;
#31850 = CARTESIAN_POINT ( 'NONE',  ( 28.40365102626034144, -13.30632128221580857, -8.403770473392276230 ) ) ;
#31851 = FACE_OUTER_BOUND ( 'NONE', #2901, .T. ) ;
#31852 = AXIS2_PLACEMENT_3D ( 'NONE', #22378, #17294, #15011 ) ;
#31853 = DIRECTION ( 'NONE',  ( -0.6797146636928645957, -0.1949050434465350867, 0.7071067811865476838 ) ) ;
#31854 = ORIENTED_EDGE ( 'NONE', *, *, #27838, .F. ) ;
#31855 = CARTESIAN_POINT ( 'NONE',  ( -12.61887306221779248, -2.123693335316770181, -7.872981162211413420 ) ) ;
#31856 = CARTESIAN_POINT ( 'NONE',  ( 33.71785032049135111, 26.96664230456639899, 47.04930799450051637 ) ) ;
#31857 = EDGE_LOOP ( 'NONE', ( #31371, #9703, #3352, #686 ) ) ;
#31858 = CARTESIAN_POINT ( 'NONE',  ( 45.73035263060504718, 25.83954579807171115, 44.36855633853329550 ) ) ;
#31859 = EDGE_CURVE ( 'NONE', #28129, #26531, #4985, .T. ) ;
#31860 = LINE ( 'NONE', #29405, #10694 ) ;
#31861 = EDGE_CURVE ( 'NONE', #23543, #18622, #15280, .T. ) ;
#31862 = AXIS2_PLACEMENT_3D ( 'NONE', #26406, #8843, #1287 ) ;
#31863 = ADVANCED_FACE ( 'NONE', ( #18051 ), #261, .T. ) ;
#31864 = AXIS2_PLACEMENT_3D ( 'NONE', #31308, #8812, #6356 ) ;
#31865 = EDGE_LOOP ( 'NONE', ( #26776, #16416, #22821, #9105, #29376 ) ) ;
#31866 = AXIS2_PLACEMENT_3D ( 'NONE', #31977, #17525, #22281 ) ;
#31867 = DIRECTION ( 'NONE',  ( 1.000000000000000000, -0.000000000000000000, -0.000000000000000000 ) ) ;
#31868 = DIRECTION ( 'NONE',  ( 0.000000000000000000, 1.000000000000000000, -0.000000000000000000 ) ) ;
#31869 = CARTESIAN_POINT ( 'NONE',  ( 72.46987649561761202, 10.07216359114295834, 73.29268005255001128 ) ) ;
#31870 = CARTESIAN_POINT ( 'NONE',  ( 49.44739180854976013, 25.27786309983298807, 47.17133137409169308 ) ) ;
#31871 = VECTOR ( 'NONE', #4464, 1000.000000000000227 ) ;
#31872 = VERTEX_POINT ( 'NONE', #5431 ) ;
#31873 = DIRECTION ( 'NONE',  ( -1.101824276508909887E-16, 1.000000000000000000, -0.000000000000000000 ) ) ;
#31874 = DIRECTION ( 'NONE',  ( 1.188208965918165239E-16, 1.880121038077813132E-16, 1.000000000000000000 ) ) ;
#31875 = EDGE_CURVE ( 'NONE', #31760, #1013, #22815, .T. ) ;
#31876 = DIRECTION ( 'NONE',  ( -0.8746197071393926326, 0.4848096202463430537, 8.676864087101709653E-18 ) ) ;
#31877 = CARTESIAN_POINT ( 'NONE',  ( 44.87087493598345134, 26.65322093266652104, 48.18533415931919706 ) ) ;
#31878 = DIRECTION ( 'NONE',  ( 0.000000000000000000, 0.000000000000000000, -1.000000000000000000 ) ) ;
#31879 = CARTESIAN_POINT ( 'NONE',  ( -31.23570478744295187, -13.74047052604243646, 21.24731629327110127 ) ) ;
#31880 = CARTESIAN_POINT ( 'NONE',  ( 33.50134396954525329, 26.34164230456639899, 47.04930799450051637 ) ) ;
#31881 =( NAMED_UNIT ( * ) PLANE_ANGLE_UNIT ( ) SI_UNIT ( $, .RADIAN. ) );
#31882 = FILL_AREA_STYLE ('',( #24826 ) ) ;
#31883 = ORIENTED_EDGE ( 'NONE', *, *, #7437, .F. ) ;
#31884 = CARTESIAN_POINT ( 'NONE',  ( -35.64882101543633297, 9.925589859889724309, 52.04930799450051637 ) ) ;
#31885 = VECTOR ( 'NONE', #8546, 1000.000000000000000 ) ;
#31886 = DIRECTION ( 'NONE',  ( 0.9996573249755574819, 1.344306794811909066E-16, 0.02617694830786587365 ) ) ;
#31887 = CARTESIAN_POINT ( 'NONE',  ( -29.57057120148431650, 10.93554979939848693, 22.25697859473322637 ) ) ;
#31888 = VECTOR ( 'NONE', #28233, 1000.000000000000000 ) ;
#31889 = DIRECTION ( 'NONE',  ( 0.000000000000000000, 0.000000000000000000, 1.000000000000000000 ) ) ;
#31890 = ORIENTED_EDGE ( 'NONE', *, *, #4944, .T. ) ;
#31891 =( BOUNDED_CURVE ( )  B_SPLINE_CURVE ( 2, ( #10596, #8125, #18121, #22886, #398, #10427, #20419, #31734, #23694 ),
 .UNSPECIFIED., .F., .F. ) 
 B_SPLINE_CURVE_WITH_KNOTS ( ( 3, 2, 2, 2, 3 ),
 ( 0.1785714274101558585, 0.1904761904761904656, 0.2142857142857143016, 0.2380952380952381375, 0.2499999988387273664 ),
 .UNSPECIFIED. ) 
 CURVE ( )  GEOMETRIC_REPRESENTATION_ITEM ( )  RATIONAL_B_SPLINE_CURVE ( ( 0.9330127018922200755, 0.9330126953578157245, 1.000000000000000000, 0.8660254037844387076, 1.000000000000000000, 0.8660254037844387076, 1.000000000000000000, 0.9330127084266226500, 0.9330127018922199644 ) ) 
 REPRESENTATION_ITEM ( '' )  );
#31892 = CARTESIAN_POINT ( 'NONE',  ( 33.72499318558949710, 30.84143805560860585, 47.04930799450051637 ) ) ;
#31893 = FACE_OUTER_BOUND ( 'NONE', #1939, .T. ) ;
#31894 = CIRCLE ( 'NONE', #963, 12.27641737965288371 ) ;
#31895 = EDGE_CURVE ( 'NONE', #25630, #32279, #22981, .T. ) ;
#31896 = EDGE_LOOP ( 'NONE', ( #22241, #23876, #27518, #6027 ) ) ;
#31897 = ORIENTED_EDGE ( 'NONE', *, *, #14617, .T. ) ;
#31898 = CARTESIAN_POINT ( 'NONE',  ( -40.11553135844171436, 6.871094863070439374, 39.51608551794754476 ) ) ;
#31899 = CARTESIAN_POINT ( 'NONE',  ( -39.39739818181173803, -5.935454207752198563, 77.87546120947918382 ) ) ;
#31900 = DIRECTION ( 'NONE',  ( 0.000000000000000000, 0.000000000000000000, 1.000000000000000000 ) ) ;
#31901 = ADVANCED_FACE ( 'NONE', ( #25385 ), #3399, .F. ) ;
#31902 = TOROIDAL_SURFACE ( 'NONE', #11464, 0.8999999999999995781, 0.1000000000000000056 ) ;
#31903 = CARTESIAN_POINT ( 'NONE',  ( -36.76418579970419387, 10.14130568307076352, 57.95249952744806166 ) ) ;
#31904 = VERTEX_POINT ( 'NONE', #113 ) ;
#31905 = DIRECTION ( 'NONE',  ( -1.101824276508909887E-16, 1.000000000000000000, -0.000000000000000000 ) ) ;
#31906 = EDGE_LOOP ( 'NONE', ( #5202, #6647, #29762 ) ) ;
#31907 = EDGE_CURVE ( 'NONE', #30099, #1027, #14394, .T. ) ;
#31908 = EDGE_CURVE ( 'NONE', #15214, #25764, #25230, .T. ) ;
#31909 = VERTEX_POINT ( 'NONE', #17344 ) ;
#31910 = EDGE_CURVE ( 'NONE', #23289, #21342, #6037, .T. ) ;
#31911 = FACE_OUTER_BOUND ( 'NONE', #28548, .T. ) ;
#31912 = AXIS2_PLACEMENT_3D ( 'NONE', #4049, #12102, #2078 ) ;
#31913 = TOROIDAL_SURFACE ( 'NONE', #13071, 12.61792373059895667, 0.1249999999999982098 ) ;
#31914 = ORIENTED_EDGE ( 'NONE', *, *, #9719, .F. ) ;
#31915 = TOROIDAL_SURFACE ( 'NONE', #25097, 12.40141737965288371, 0.1249999999999996253 ) ;
#31916 = CARTESIAN_POINT ( 'NONE',  ( -30.09469955099472216, 5.197876425781705834, 77.54511166671605338 ) ) ;
#31917 = CARTESIAN_POINT ( 'NONE',  ( -38.65545646816406133, -4.281517947942904634, 80.46297774100551692 ) ) ;
#31918 = EDGE_LOOP ( 'NONE', ( #2303, #3088, #7338, #8225 ) ) ;
#31919 = CIRCLE ( 'NONE', #2592, 12.36707279061065101 ) ;
#31920 = CARTESIAN_POINT ( 'NONE',  ( 48.23388202445966755, 27.65087065737811756, 49.27628909396056400 ) ) ;
#31921 = VERTEX_POINT ( 'NONE', #275 ) ;
#31922 = DIRECTION ( 'NONE',  ( -1.000000000000000000, 0.000000000000000000, 0.000000000000000000 ) ) ;
#31923 = DIRECTION ( 'NONE',  ( -0.4848096202463430537, -0.8746197071393926326, -9.920727850371700117E-18 ) ) ;
#31924 = CARTESIAN_POINT ( 'NONE',  ( 21.09785597605719332, 13.06454579224780055, -7.694940604469596934 ) ) ;
#31925 = VERTEX_POINT ( 'NONE', #12111 ) ;
#31926 = LINE ( 'NONE', #17134, #8675 ) ;
#31927 = DIRECTION ( 'NONE',  ( -0.000000000000000000, -1.000000000000000000, -0.000000000000000000 ) ) ;
#31928 = CARTESIAN_POINT ( 'NONE',  ( 9.016997203727582288, 34.59164230456639899, 47.36565641480107303 ) ) ;
#31929 = DIRECTION ( 'NONE',  ( -1.000000000000000000, 0.000000000000000000, 0.000000000000000000 ) ) ;
#31930 = LINE ( 'NONE', #2389, #6843 ) ;
#31931 = DIRECTION ( 'NONE',  ( 1.234978253042719660E-16, -1.000000000000000000, -1.109335647967047851E-31 ) ) ;
#31932 = VERTEX_POINT ( 'NONE', #17172 ) ;
#31933 = DIRECTION ( 'NONE',  ( 1.000000000000000000, 0.000000000000000000, 0.000000000000000000 ) ) ;
#31934 = DIRECTION ( 'NONE',  ( -1.000000000000000000, 0.000000000000000000, 0.000000000000000000 ) ) ;
#31935 = EDGE_CURVE ( 'NONE', #12577, #756, #22249, .T. ) ;
#31936 = ORIENTED_EDGE ( 'NONE', *, *, #12421, .F. ) ;
#31937 = DIRECTION ( 'NONE',  ( -1.000000000000000000, 0.000000000000000000, 0.000000000000000000 ) ) ;
#31938 = AXIS2_PLACEMENT_3D ( 'NONE', #21927, #6522, #28849 ) ;
#31939 = AXIS2_PLACEMENT_3D ( 'NONE', #7975, #10277, #25521 ) ;
#31940 = ADVANCED_FACE ( 'NONE', ( #27856 ), #23821, .F. ) ;
#31941 = CARTESIAN_POINT ( 'NONE',  ( -42.68334051588269062, -0.7182646751426463583, 32.04930799450052348 ) ) ;
#31942 = EDGE_LOOP ( 'NONE', ( #20648, #19359, #13598, #914 ) ) ;
#31943 = ORIENTED_EDGE ( 'NONE', *, *, #11481, .T. ) ;
#31944 = EDGE_CURVE ( 'NONE', #5329, #3369, #4432, .T. ) ;
#31945 = VECTOR ( 'NONE', #16224, 1000.000000000000000 ) ;
#31946 = ORIENTED_EDGE ( 'NONE', *, *, #4991, .F. ) ;
#31947 = EDGE_CURVE ( 'NONE', #21115, #3553, #9968, .T. ) ;
#31948 = TOROIDAL_SURFACE ( 'NONE', #14666, 13.20178401536290913, 0.2000000000000002609 ) ;
#31949 = CARTESIAN_POINT ( 'NONE',  ( -41.93344242462055149, 13.82826554927148166, 54.56265170360538264 ) ) ;
#31950 = CIRCLE ( 'NONE', #16757, 13.23540278830031447 ) ;
#31951 = CIRCLE ( 'NONE', #26188, 94.94530576803616384 ) ;
#31952 = ORIENTED_EDGE ( 'NONE', *, *, #26307, .T. ) ;
#31953 = ORIENTED_EDGE ( 'NONE', *, *, #13950, .T. ) ;
#31954 = CARTESIAN_POINT ( 'NONE',  ( -40.11286833322907341, 2.887657226147507306, 37.04930799450052348 ) ) ;
#31955 = DIRECTION ( 'NONE',  ( 0.4848096202463673121, 0.8746197071393789768, 0.000000000000000000 ) ) ;
#31956 = FACE_OUTER_BOUND ( 'NONE', #19626, .T. ) ;
#31957 = LINE ( 'NONE', #24733, #28992 ) ;
#31958 = CARTESIAN_POINT ( 'NONE',  ( 47.20353132263855400, 29.65286309983298096, 45.01455027646041174 ) ) ;
#31959 = ORIENTED_EDGE ( 'NONE', *, *, #5362, .T. ) ;
#31960 = EDGE_LOOP ( 'NONE', ( #24858, #24719, #5830, #12434 ) ) ;
#31961 = CARTESIAN_POINT ( 'NONE',  ( -9.918530130619847895, 4.323180411458210415, -4.396266667175535048 ) ) ;
#31962 = VERTEX_POINT ( 'NONE', #10941 ) ;
#31963 = DIRECTION ( 'NONE',  ( -1.000000000000000000, 0.000000000000000000, 0.000000000000000000 ) ) ;
#31964 = CARTESIAN_POINT ( 'NONE',  ( 21.09992658989238734, 30.84164230456639544, 47.04930799450051637 ) ) ;
#31965 = CIRCLE ( 'NONE', #25153, 0.1000000000000016709 ) ;
#31966 = VECTOR ( 'NONE', #28475, 1000.000000000000227 ) ;
#31967 = CARTESIAN_POINT ( 'NONE',  ( 44.79156314060809763, 22.80400562401889530, 46.92953032342012420 ) ) ;
#31968 = DIRECTION ( 'NONE',  ( 0.7141240004913684825, -0.3958453973319465691, 0.5773502691896116312 ) ) ;
#31969 = DIRECTION ( 'NONE',  ( -1.101824276508909887E-16, 1.000000000000000000, -0.000000000000000000 ) ) ;
#31970 = CARTESIAN_POINT ( 'NONE',  ( 49.28428300279882990, 25.54787913140504685, 48.46772541801551171 ) ) ;
#31971 = TOROIDAL_SURFACE ( 'NONE', #17815, 12.40141737965282154, 0.1250000000000006939 ) ;
#31972 = CARTESIAN_POINT ( 'NONE',  ( 47.14231618896855025, 22.89977464660286444, 48.91282684219816446 ) ) ;
#31973 = DIRECTION ( 'NONE',  ( -1.101824276508909887E-16, 1.000000000000000000, -0.000000000000000000 ) ) ;
#31974 = ORIENTED_EDGE ( 'NONE', *, *, #11719, .T. ) ;
#31975 = CARTESIAN_POINT ( 'NONE',  ( -41.02113223168485234, 7.230835263863472306, 39.44930799450052206 ) ) ;
#31976 = CIRCLE ( 'NONE', #2069, 0.09999999999999792388 ) ;
#31977 = CARTESIAN_POINT ( 'NONE',  ( 21.09992658989239089, 23.59164230456639544, 47.04930799450051637 ) ) ;
#31978 = DIRECTION ( 'NONE',  ( -1.101824276508909887E-16, 1.000000000000000000, -0.000000000000000000 ) ) ;
#31979 = CARTESIAN_POINT ( 'NONE',  ( 48.68948053213853910, 22.89977464660286444, 46.07904489681320115 ) ) ;
#31980 = DIRECTION ( 'NONE',  ( -0.2155021956183748588, 0.9702957262759968060, 0.1099318300320501068 ) ) ;
#31981 = ORIENTED_EDGE ( 'NONE', *, *, #3204, .F. ) ;
#31982 = ORIENTED_EDGE ( 'NONE', *, *, #19658, .T. ) ;
#31983 = CARTESIAN_POINT ( 'NONE',  ( 21.09785597605720753, 17.16467605102632632, 47.04930799450052348 ) ) ;
#31984 = AXIS2_PLACEMENT_3D ( 'NONE', #1843, #19224, #6611 ) ;
#31985 = EDGE_CURVE ( 'NONE', #21006, #25197, #26971, .T. ) ;
#31986 = ORIENTED_EDGE ( 'NONE', *, *, #9031, .T. ) ;
#31987 = EDGE_CURVE ( 'NONE', #13785, #8280, #28016, .T. ) ;
#31988 = CIRCLE ( 'NONE', #30946, 33.50000000000000000 ) ;
#31989 = AXIS2_PLACEMENT_3D ( 'NONE', #26909, #6238, #14113 ) ;
#31990 = AXIS2_PLACEMENT_3D ( 'NONE', #18867, #13805, #28905 ) ;
#31991 = EDGE_LOOP ( 'NONE', ( #21445, #11802, #4057, #3926 ) ) ;
#31992 = CARTESIAN_POINT ( 'NONE',  ( 21.09785597605719332, -16.63545420775219696, 47.04930799450051637 ) ) ;
#31993 = AXIS2_PLACEMENT_3D ( 'NONE', #22855, #368, #15623 ) ;
#31994 = CARTESIAN_POINT ( 'NONE',  ( 47.79865503179234310, 9.702389020015065313, -12.70392589783158499 ) ) ;
#31995 = CARTESIAN_POINT ( 'NONE',  ( -40.11286833322907341, 2.887657226147507306, 35.74930799450051921 ) ) ;
#31996 = CIRCLE ( 'NONE', #5811, 13.00000000000000533 ) ;
#31997 = ORIENTED_EDGE ( 'NONE', *, *, #6526, .T. ) ;
#31998 = CARTESIAN_POINT ( 'NONE',  ( 44.59785597605720397, 14.86454579224779948, 47.04930799450052348 ) ) ;
#31999 = DIRECTION ( 'NONE',  ( -1.000000000000000000, 0.000000000000000000, 0.000000000000000000 ) ) ;
#32000 = CARTESIAN_POINT ( 'NONE',  ( 78.03121069986417524, -4.668720686625185579, 13.94775564540398172 ) ) ;
#32001 = VERTEX_POINT ( 'NONE', #30648 ) ;
#32002 = ORIENTED_EDGE ( 'NONE', *, *, #32216, .F. ) ;
#32003 = DIRECTION ( 'NONE',  ( 1.000000000000000000, 0.000000000000000000, 0.000000000000000000 ) ) ;
#32004 = VECTOR ( 'NONE', #2257, 1000.000000000000000 ) ;
#32005 = EDGE_LOOP ( 'NONE', ( #30048, #22959, #29377, #22854 ) ) ;
#32006 = CARTESIAN_POINT ( 'NONE',  ( 21.09785597605719332, 25.56454579224779167, 18.54930799450051282 ) ) ;
#32007 = DIRECTION ( 'NONE',  ( 1.000000000000000000, 0.000000000000000000, 0.000000000000000000 ) ) ;
#32008 = PLANE ( 'NONE',  #1707 ) ;
#32009 = DIRECTION ( 'NONE',  ( -0.2756373558170082672, 0.9612616959383162296, 0.000000000000000000 ) ) ;
#32010 =( NAMED_UNIT ( * ) SI_UNIT ( $, .STERADIAN. ) SOLID_ANGLE_UNIT ( ) );
#32011 = ORIENTED_EDGE ( 'NONE', *, *, #20470, .T. ) ;
#32012 = ORIENTED_EDGE ( 'NONE', *, *, #19205, .T. ) ;
#32013 = CARTESIAN_POINT ( 'NONE',  ( -40.70484894842233103, 8.274204744976163539, 59.44930799450051495 ) ) ;
#32014 = CARTESIAN_POINT ( 'NONE',  ( -40.05987053574653345, 7.506472619680471858, 35.64930799450052490 ) ) ;
#32015 = TOROIDAL_SURFACE ( 'NONE', #17861, 13.98419020052803852, 1.000000000001014744 ) ;
#32016 = DIRECTION ( 'NONE',  ( -2.779292025043186357E-18, 1.288349127009862211E-17, -1.000000000000000000 ) ) ;
#32017 = ORIENTED_EDGE ( 'NONE', *, *, #2115, .F. ) ;
#32018 = CARTESIAN_POINT ( 'NONE',  ( 21.09785597605720753, -13.56320000832927875, -8.579118024061138215 ) ) ;
#32019 = AXIS2_PLACEMENT_3D ( 'NONE', #21263, #772, #21102 ) ;
#32020 = CARTESIAN_POINT ( 'NONE',  ( 59.57376688280871235, -13.74047052604243468, 90.91442668615565026 ) ) ;
#32021 = ORIENTED_EDGE ( 'NONE', *, *, #26529, .F. ) ;
#32022 = DIRECTION ( 'NONE',  ( 0.000000000000000000, 0.000000000000000000, -1.000000000000000000 ) ) ;
#32023 = AXIS2_PLACEMENT_3D ( 'NONE', #32290, #19796, #29828 ) ;
#32024 = CARTESIAN_POINT ( 'NONE',  ( -40.60722745863126448, 9.415333058485025219, 39.40788663826321425 ) ) ;
#32025 = AXIS2_PLACEMENT_3D ( 'NONE', #11869, #24007, #21536 ) ;
#32026 = DIRECTION ( 'NONE',  ( -0.8746197071393858602, 0.4848096202463547666, 0.000000000000000000 ) ) ;
#32027 = ADVANCED_FACE ( 'NONE', ( #8637 ), #8159, .T. ) ;
#32028 = EDGE_CURVE ( 'NONE', #31626, #9845, #26452, .T. ) ;
#32029 = ADVANCED_FACE ( 'NONE', ( #20936 ), #1081, .F. ) ;
#32030 = EDGE_CURVE ( 'NONE', #4736, #5569, #12311, .T. ) ;
#32031 = CIRCLE ( 'NONE', #16273, 0.1249999999999931721 ) ;
#32032 = EDGE_LOOP ( 'NONE', ( #238, #27939, #31086, #4976 ) ) ;
#32033 = DIRECTION ( 'NONE',  ( 0.3428121700606640565, 0.6184495258776567805, -0.7071067811865473507 ) ) ;
#32034 = CYLINDRICAL_SURFACE ( 'NONE', #31178, 0.1000000000000010325 ) ;
#32035 = DIRECTION ( 'NONE',  ( 1.000000000000000000, 0.000000000000000000, 0.000000000000000000 ) ) ;
#32036 = CARTESIAN_POINT ( 'NONE',  ( 44.70507715278255745, 26.34951373492759430, 46.92503878583765697 ) ) ;
#32037 = ORIENTED_EDGE ( 'NONE', *, *, #2155, .T. ) ;
#32038 = AXIS2_PLACEMENT_3D ( 'NONE', #22235, #27164, #22394 ) ;
#32039 = CARTESIAN_POINT ( 'NONE',  ( -30.89605511857125464, 11.92558985988973497, 67.46350265493038023 ) ) ;
#32040 = DIRECTION ( 'NONE',  ( 0.000000000000000000, 0.000000000000000000, -1.000000000000000000 ) ) ;
#32041 = VECTOR ( 'NONE', #30762, 1000.000000000000000 ) ;
#32042 = CLOSED_SHELL ( 'NONE', ( #32356, #9817, #24560, #21105, #16620, #9942, #29857, #23124, #27469, #10240, #5560, #27712, #25397, #29729, #15351, #3800, #17377, #8594, #31224, #23167, #27679, #11683, #31940, #30513, #549, #27497, #24480, #6974, #10245, #8931, #19022, #5834, #25447, #7866, #24991, #8572, #10052, #4264, #4607, #8137, #22153, #32471, #9398, #21957, #16553, #4857, #6996, #21471, #9222, #13190, #30628, #17330, #16998, #1806, #1376, #16150, #32442, #6736, #12006, #26294, #18450, #27996, #14638, #15931, #25530, #18802, #15411, #9583, #27547, #26822, #30992, #27084, #29328 ) ) ;
#32043 = CARTESIAN_POINT ( 'NONE',  ( 53.59103788013077008, -5.321843574075685979, -9.729082480673143962 ) ) ;
#32044 = VECTOR ( 'NONE', #25237, 1000.000000000000000 ) ;
#32045 = DIRECTION ( 'NONE',  ( -0.8746197071393858602, 0.4848096202463547666, 0.000000000000000000 ) ) ;
#32046 = DIRECTION ( 'NONE',  ( 0.000000000000000000, 0.000000000000000000, 1.000000000000000000 ) ) ;
#32047 = CARTESIAN_POINT ( 'NONE',  ( -8.081090960560114667, -13.74047052604243646, -3.479232590077480758 ) ) ;
#32048 = LINE ( 'NONE', #22679, #21487 ) ;
#32049 = DIRECTION ( 'NONE',  ( -1.101824276508909887E-16, 1.000000000000000000, -0.000000000000000000 ) ) ;
#32050 = CARTESIAN_POINT ( 'NONE',  ( -40.61650700234910971, 6.826799243660863326, 39.53667871757248520 ) ) ;
#32051 =( NAMED_UNIT ( * ) PLANE_ANGLE_UNIT ( ) SI_UNIT ( $, .RADIAN. ) );
#32052 = ORIENTED_EDGE ( 'NONE', *, *, #9225, .F. ) ;
#32053 = EDGE_CURVE ( 'NONE', #3864, #756, #31176, .T. ) ;
#32054 = CARTESIAN_POINT ( 'NONE',  ( 45.62581776903441977, 22.92747281079970278, 46.09434135054691950 ) ) ;
#32055 = CIRCLE ( 'NONE', #8463, 2.500000000000002220 ) ;
#32056 = EDGE_CURVE ( 'NONE', #16262, #23526, #8479, .T. ) ;
#32057 = LINE ( 'NONE', #19229, #27705 ) ;
#32058 = CARTESIAN_POINT ( 'NONE',  ( 49.66977585544405827, 24.86874180309281712, 46.07579470028509405 ) ) ;
#32059 = CARTESIAN_POINT ( 'NONE',  ( 52.46240689619265396, -5.913508961333112879, 104.8323960743217782 ) ) ;
#32060 = ORIENTED_EDGE ( 'NONE', *, *, #1703, .T. ) ;
#32061 = CARTESIAN_POINT ( 'NONE',  ( -39.51359738027355206, -5.935454207752198563, 77.87546120947918382 ) ) ;
#32062 = DIRECTION ( 'NONE',  ( -0.000000000000000000, -1.000000000000000000, 0.000000000000000000 ) ) ;
#32063 = CARTESIAN_POINT ( 'NONE',  ( -40.18454328187963398, 7.548069831825862330, 60.29072935073781991 ) ) ;
#32064 = ORIENTED_EDGE ( 'NONE', *, *, #17891, .T. ) ;
#32065 = ORIENTED_EDGE ( 'NONE', *, *, #13867, .F. ) ;
#32066 = DIRECTION ( 'NONE',  ( 0.8746197071393926326, -0.4848096202463430537, -8.676864087101709653E-18 ) ) ;
#32067 = PLANE ( 'NONE',  #7319 ) ;
#32068 = CARTESIAN_POINT ( 'NONE',  ( -10.96598430569368432, -5.983766253076982622, -12.62465409255485582 ) ) ;
#32069 = DIRECTION ( 'NONE',  ( -1.101824276508909887E-16, 1.000000000000000000, -0.000000000000000000 ) ) ;
#32070 = CIRCLE ( 'NONE', #28389, 12.27641737965281798 ) ;
#32071 = ORIENTED_EDGE ( 'NONE', *, *, #16476, .T. ) ;
#32072 = CARTESIAN_POINT ( 'NONE',  ( 72.68275509767009623, 11.86918370369814113, 25.53922971596723102 ) ) ;
#32073 = CIRCLE ( 'NONE', #12135, 0.5000000000000004441 ) ;
#32074 = VERTEX_POINT ( 'NONE', #23082 ) ;
#32075 = MECHANICAL_DESIGN_GEOMETRIC_PRESENTATION_REPRESENTATION (  '', ( #8475 ), #29451 ) ;
#32076 = ADVANCED_FACE ( 'NONE', ( #30799 ), #21188, .T. ) ;
#32077 = ORIENTED_EDGE ( 'NONE', *, *, #16193, .F. ) ;
#32078 = AXIS2_PLACEMENT_3D ( 'NONE', #19803, #7515, #32299 ) ;
#32079 = EDGE_LOOP ( 'NONE', ( #11687, #20733, #9012, #24591, #28661, #12537, #25074, #10522 ) ) ;
#32080 = EDGE_CURVE ( 'NONE', #31343, #24565, #20172, .T. ) ;
#32081 = DIRECTION ( 'NONE',  ( -7.588956326749211550E-18, 4.206627182996912454E-18, -1.000000000000000000 ) ) ;
#32082 = CARTESIAN_POINT ( 'NONE',  ( -30.51040964360577235, 3.734882690806572203, 78.42680211664418266 ) ) ;
#32083 = EDGE_CURVE ( 'NONE', #28828, #32275, #13876, .T. ) ;
#32084 = ORIENTED_EDGE ( 'NONE', *, *, #3337, .F. ) ;
#32085 = CARTESIAN_POINT ( 'NONE',  ( 33.72499318558949710, 30.34184655352422411, 47.04930799450051637 ) ) ;
#32086 = ORIENTED_EDGE ( 'NONE', *, *, #123, .T. ) ;
#32087 = CARTESIAN_POINT ( 'NONE',  ( 21.09992658989239089, 24.59164230456639544, 47.04930799450051637 ) ) ;
#32088 = AXIS2_PLACEMENT_3D ( 'NONE', #17962, #20906, #7971 ) ;
#32089 =( BOUNDED_CURVE ( )  B_SPLINE_CURVE ( 3, ( #7910, #22829, #28092, #3121 ),
 .UNSPECIFIED., .F., .F. ) 
 B_SPLINE_CURVE_WITH_KNOTS ( ( 4, 4 ),
 ( 5.497787143782102426, 6.283185307179586232 ),
 .UNSPECIFIED. ) 
 CURVE ( )  GEOMETRIC_REPRESENTATION_ITEM ( )  RATIONAL_B_SPLINE_CURVE ( ( 1.000000000000000000, 0.9492530216741865701, 0.9492530216741865701, 1.000000000000000000 ) ) 
 REPRESENTATION_ITEM ( '' )  );
#32090 = DIRECTION ( 'NONE',  ( -0.2756373558169945559, 0.9612616959383202264, 0.000000000000000000 ) ) ;
#32091 = CARTESIAN_POINT ( 'NONE',  ( 21.09785597605719332, 25.18020726757345429, 47.04930799450051637 ) ) ;
#32092 = ORIENTED_EDGE ( 'NONE', *, *, #16744, .T. ) ;
#32093 = ADVANCED_FACE ( 'NONE', ( #7999 ), #28341, .T. ) ;
#32094 = CARTESIAN_POINT ( 'NONE',  ( -40.28779227465695811, 2.984619150196779813, 57.04930799450051637 ) ) ;
#32095 = LINE ( 'NONE', #4677, #26936 ) ;
#32096 = CARTESIAN_POINT ( 'NONE',  ( 21.09785597605719332, 28.56454579224779877, 47.04930799450051637 ) ) ;
#32097 = ADVANCED_FACE ( 'NONE', ( #25546, #3051 ), #604, .F. ) ;
#32098 = DIRECTION ( 'NONE',  ( -1.000000000000000000, 0.000000000000000000, 0.000000000000000000 ) ) ;
#32099 = CARTESIAN_POINT ( 'NONE',  ( -40.57832940339291383, 7.446916344587776848, 53.80788663826320573 ) ) ;
#32100 = DIRECTION ( 'NONE',  ( -1.101824276508909887E-16, 1.000000000000000000, -0.000000000000000000 ) ) ;
#32101 = EDGE_CURVE ( 'NONE', #10562, #7332, #18093, .T. ) ;
#32102 = CARTESIAN_POINT ( 'NONE',  ( 36.45249510457200870, 15.11603238453479037, 47.04930799450052348 ) ) ;
#32103 = VERTEX_POINT ( 'NONE', #13412 ) ;
#32104 = DIRECTION ( 'NONE',  ( 0.000000000000000000, -1.000000000000000000, 0.000000000000000000 ) ) ;
#32105 = FACE_OUTER_BOUND ( 'NONE', #11174, .T. ) ;
#32106 = VERTEX_POINT ( 'NONE', #23562 ) ;
#32107 = DIRECTION ( 'NONE',  ( -1.000000000000000000, 0.000000000000000000, 0.000000000000000000 ) ) ;
#32108 = DIRECTION ( 'NONE',  ( -1.101824276508909887E-16, 1.000000000000000000, -0.000000000000000000 ) ) ;
#32109 = AXIS2_PLACEMENT_3D ( 'NONE', #15260, #2462, #22803 ) ;
#32110 = VERTEX_POINT ( 'NONE', #23408 ) ;
#32111 = PRODUCT_DEFINITION_SHAPE ( 'NONE', 'NONE',  #9511 ) ;
#32112 = ORIENTED_EDGE ( 'NONE', *, *, #22217, .T. ) ;
#32113 = EDGE_CURVE ( 'NONE', #8460, #3912, #1849, .T. ) ;
#32114 = AXIS2_PLACEMENT_3D ( 'NONE', #9807, #19801, #29834 ) ;
#32115 = ORIENTED_EDGE ( 'NONE', *, *, #31538, .T. ) ;
#32116 = CIRCLE ( 'NONE', #27383, 0.9031915329475502796 ) ;
#32117 = EDGE_CURVE ( 'NONE', #6039, #8138, #32375, .T. ) ;
#32118 = DIRECTION ( 'NONE',  ( -1.101824276508909887E-16, 1.000000000000000000, -0.000000000000000000 ) ) ;
#32119 = EDGE_CURVE ( 'NONE', #5692, #13543, #11581, .T. ) ;
#32120 = ORIENTED_EDGE ( 'NONE', *, *, #7152, .F. ) ;
#32121 = ORIENTED_EDGE ( 'NONE', *, *, #2952, .F. ) ;
#32122 = DIRECTION ( 'NONE',  ( -1.224646799147353207E-16, -1.349345573449484691E-32, 1.000000000000000000 ) ) ;
#32123 = AXIS2_PLACEMENT_3D ( 'NONE', #17882, #2136, #22145 ) ;
#32124 = CARTESIAN_POINT ( 'NONE',  ( 46.58650058836976626, 22.86454579224779593, 49.02544611800051655 ) ) ;
#32125 = DIRECTION ( 'NONE',  ( -0.8746197071393840838, 0.4848096202463581528, 0.000000000000000000 ) ) ;
#32126 = AXIS2_PLACEMENT_3D ( 'NONE', #10820, #23600, #20812 ) ;
#32127 = FACE_OUTER_BOUND ( 'NONE', #20890, .T. ) ;
#32128 = ORIENTED_EDGE ( 'NONE', *, *, #15400, .T. ) ;
#32129 = DIRECTION ( 'NONE',  ( -1.000000000000000000, 0.000000000000000000, 0.000000000000000000 ) ) ;
#32130 = ORIENTED_EDGE ( 'NONE', *, *, #8252, .T. ) ;
#32131 = CARTESIAN_POINT ( 'NONE',  ( 21.09785597605720042, -16.03545420775220265, 47.04930799450051637 ) ) ;
#32132 = CARTESIAN_POINT ( 'NONE',  ( -40.47970302497626705, 7.463434137431151250, 53.64930799450051779 ) ) ;
#32133 = EDGE_CURVE ( 'NONE', #12291, #13584, #2378, .T. ) ;
#32134 = ORIENTED_EDGE ( 'NONE', *, *, #13324, .F. ) ;
#32135 = CARTESIAN_POINT ( 'NONE',  ( 21.09785597605720042, -16.73545420775220194, -31.35069200549948221 ) ) ;
#32136 = CARTESIAN_POINT ( 'NONE',  ( -37.58300281841709989, 16.01180101885526597, 36.00717268343339583 ) ) ;
#32137 = LINE ( 'NONE', #7181, #23657 ) ;
#32138 = CARTESIAN_POINT ( 'NONE',  ( -40.18454328187963398, 7.548069831825862330, 60.29072935073781991 ) ) ;
#32139 = EDGE_CURVE ( 'NONE', #649, #3624, #18589, .T. ) ;
#32140 = CARTESIAN_POINT ( 'NONE',  ( 45.46000861347822308, 24.67287913140504685, 49.57397645940629616 ) ) ;
#32141 = VECTOR ( 'NONE', #6990, 1000.000000000000227 ) ;
#32142 = VECTOR ( 'NONE', #17182, 1000.000000000000000 ) ;
#32143 = CARTESIAN_POINT ( 'NONE',  ( 46.86983284546423079, 22.95310733321322161, 48.67358610625728232 ) ) ;
#32144 = CARTESIAN_POINT ( 'NONE',  ( -41.94956971822180947, 3.905757428664830222, 48.24930799450051211 ) ) ;
#32145 = EDGE_LOOP ( 'NONE', ( #5994, #23386, #5091, #7553 ) ) ;
#32146 = CARTESIAN_POINT ( 'NONE',  ( -58.11219453028166981, -15.93545420775219945, 47.04930799450023926 ) ) ;
#32147 = LINE ( 'NONE', #27207, #25589 ) ;
#32148 = FACE_OUTER_BOUND ( 'NONE', #14477, .T. ) ;
#32149 = LINE ( 'NONE', #4246, #646 ) ;
#32150 = DIRECTION ( 'NONE',  ( 0.9612616959383188942, 0.2756373558169995519, -1.660411357259292306E-16 ) ) ;
#32151 = ORIENTED_EDGE ( 'NONE', *, *, #11756, .T. ) ;
#32152 = EDGE_LOOP ( 'NONE', ( #31714, #28006, #6991, #153 ) ) ;
#32153 = CARTESIAN_POINT ( 'NONE',  ( -42.37913764077812573, 15.23192269303852875, 35.64930799450052490 ) ) ;
#32154 = VERTEX_POINT ( 'NONE', #26348 ) ;
#32155 = AXIS2_PLACEMENT_3D ( 'NONE', #17015, #30169, #27041 ) ;
#32156 = AXIS2_PLACEMENT_3D ( 'NONE', #11292, #24074, #21283 ) ;
#32157 = TOROIDAL_SURFACE ( 'NONE', #24820, 12.40141737965286595, 0.1249999999999979183 ) ;
#32158 = AXIS2_PLACEMENT_3D ( 'NONE', #22208, #12212, #32394 ) ;
#32159 = VECTOR ( 'NONE', #22276, 1000.000000000000000 ) ;
#32160 = VERTEX_POINT ( 'NONE', #9565 ) ;
#32161 = DIRECTION ( 'NONE',  ( 0.3428121700606640565, 0.6184495258776567805, -0.7071067811865474617 ) ) ;
#32162 = CARTESIAN_POINT ( 'NONE',  ( 52.02891158707559782, -5.936746300155039791, -13.39441323401713468 ) ) ;
#32163 = ORIENTED_EDGE ( 'NONE', *, *, #14763, .T. ) ;
#32164 = CARTESIAN_POINT ( 'NONE',  ( -41.34584395867850048, 11.59800658573647247, 57.04930799450051637 ) ) ;
#32165 = DIRECTION ( 'NONE',  ( -1.101824276508909887E-16, 1.000000000000000000, -0.000000000000000000 ) ) ;
#32166 = DIRECTION ( 'NONE',  ( -1.000000000000000000, 0.000000000000000000, 0.000000000000000000 ) ) ;
#32167 = CARTESIAN_POINT ( 'NONE',  ( 49.49063479933183629, 25.21291119454915375, 47.17357720316391578 ) ) ;
#32168 = ORIENTED_EDGE ( 'NONE', *, *, #16380, .T. ) ;
#32169 = ORIENTED_EDGE ( 'NONE', *, *, #22096, .T. ) ;
#32170 = CARTESIAN_POINT ( 'NONE',  ( 21.09785597605719332, 40.56454579224780588, 47.04930799450051637 ) ) ;
#32171 = ADVANCED_FACE ( 'NONE', ( #19886, #21405, #19563, #2177, #16496, #28977 ), #11262, .T. ) ;
#32172 = ORIENTED_EDGE ( 'NONE', *, *, #7846, .F. ) ;
#32173 = CARTESIAN_POINT ( 'NONE',  ( 33.37634396954523197, 28.09164230456639544, 47.04930799450051637 ) ) ;
#32174 = DIRECTION ( 'NONE',  ( -0.000000000000000000, -1.000000000000000000, -0.000000000000000000 ) ) ;
#32175 = CARTESIAN_POINT ( 'NONE',  ( -40.68496126738437368, 6.805971067583526768, 34.76999393395801974 ) ) ;
#32176 = EDGE_CURVE ( 'NONE', #24311, #25250, #20196, .T. ) ;
#32177 = AXIS2_PLACEMENT_3D ( 'NONE', #706, #21038, #8105 ) ;
#32178 = EDGE_CURVE ( 'NONE', #13562, #10069, #3940, .T. ) ;
#32179 = CARTESIAN_POINT ( 'NONE',  ( -36.38930206846553261, 9.511667899829566508, 54.44930799450051495 ) ) ;
#32180 = CARTESIAN_POINT ( 'NONE',  ( 48.40186567930497574, 28.82957786121581378, 45.03923535223908203 ) ) ;
#32181 = DIRECTION ( 'NONE',  ( 0.3957342950827467676, -5.551115123125782702E-17, 0.9183650514339934956 ) ) ;
#32182 = EDGE_LOOP ( 'NONE', ( #22432, #9312, #13108, #29040, #5491 ) ) ;
#32183 = ORIENTED_EDGE ( 'NONE', *, *, #5669, .F. ) ;
#32184 = DIRECTION ( 'NONE',  ( -0.9612616959383206705, -0.2756373558169934457, 1.660411357259282938E-16 ) ) ;
#32185 = CARTESIAN_POINT ( 'NONE',  ( -40.18454328187963398, 7.548069831825862330, 60.54930799450051637 ) ) ;
#32186 = VECTOR ( 'NONE', #1896, 1000.000000000000000 ) ;
#32187 = DIRECTION ( 'NONE',  ( -0.000000000000000000, -1.000000000000000000, -0.000000000000000000 ) ) ;
#32188 = ORIENTED_EDGE ( 'NONE', *, *, #8767, .F. ) ;
#32189 = CARTESIAN_POINT ( 'NONE',  ( 48.94625023931840246, 27.45784706826093213, 46.10640627770149536 ) ) ;
#32190 = CARTESIAN_POINT ( 'NONE',  ( 28.71925248772582151, -13.74047052604244179, 104.8978920147615383 ) ) ;
#32191 = VERTEX_POINT ( 'NONE', #26512 ) ;
#32192 = CARTESIAN_POINT ( 'NONE',  ( 75.39785597605720113, -5.098646251524523443, 47.04930799450051637 ) ) ;
#32193 = CARTESIAN_POINT ( 'NONE',  ( 8.474859994195282908, 38.56284415653841791, 47.04930799450051637 ) ) ;
#32194 = DIRECTION ( 'NONE',  ( 0.1949050434465247061, -0.6797146636928672603, 0.7071067811865480168 ) ) ;
#32195 = ORIENTED_EDGE ( 'NONE', *, *, #1149, .T. ) ;
#32196 = AXIS2_PLACEMENT_3D ( 'NONE', #26618, #14156, #24156 ) ;
#32197 = ORIENTED_EDGE ( 'NONE', *, *, #17217, .T. ) ;
#32198 = DIRECTION ( 'NONE',  ( -0.000000000000000000, -1.000000000000000000, 0.000000000000000000 ) ) ;
#32199 = LINE ( 'NONE', #9715, #15039 ) ;
#32201 = CARTESIAN_POINT ( 'NONE',  ( -40.70484894842233103, 8.274204744976163539, 54.54930799450051637 ) ) ;
#32200 = CIRCLE ( 'NONE', #8623, 2.500000000000003553 ) ;
#32202 = CIRCLE ( 'NONE', #18044, 16.99999999999999289 ) ;
#32203 = VERTEX_POINT ( 'NONE', #29921 ) ;
#32204 = DIRECTION ( 'NONE',  ( 1.000000000000000000, 0.000000000000000000, 0.000000000000000000 ) ) ;
#32205 = CARTESIAN_POINT ( 'NONE',  ( -43.69495677161796010, 1.169528900831203311, 53.64930799450051779 ) ) ;
#32206 = CARTESIAN_POINT ( 'NONE',  ( 51.70051226388650178, 5.005525289648587339, -4.203416302359093137 ) ) ;
#32207 = EDGE_CURVE ( 'NONE', #28202, #19596, #24658, .T. ) ;
#32208 = DIRECTION ( 'NONE',  ( 0.000000000000000000, -0.000000000000000000, -1.000000000000000000 ) ) ;
#32209 = FACE_OUTER_BOUND ( 'NONE', #8804, .T. ) ;
#32210 = DIRECTION ( 'NONE',  ( -0.8746197071393890798, 0.4848096202463489934, 8.676864087101777446E-18 ) ) ;
#32211 = EDGE_CURVE ( 'NONE', #1157, #8655, #3420, .T. ) ;
#32212 = FACE_OUTER_BOUND ( 'NONE', #21126, .T. ) ;
#32214 = ADVANCED_FACE ( 'NONE', ( #7264 ), #22187, .F. ) ;
#32213 = PLANE ( 'NONE',  #12073 ) ;
#32215 = ADVANCED_FACE ( 'NONE', ( #4632 ), #9710, .T. ) ;
#32216 = EDGE_CURVE ( 'NONE', #23287, #13496, #24924, .T. ) ;
#32217 = DIRECTION ( 'NONE',  ( -1.000000000000000000, 0.000000000000000000, 0.000000000000000000 ) ) ;
#32218 = LINE ( 'NONE', #30086, #26819 ) ;
#32219 = EDGE_CURVE ( 'NONE', #14793, #12758, #5516, .T. ) ;
#32220 = VERTEX_POINT ( 'NONE', #17261 ) ;
#32221 = VERTEX_POINT ( 'NONE', #28817 ) ;
#32222 = FACE_OUTER_BOUND ( 'NONE', #32285, .T. ) ;
#32223 = CARTESIAN_POINT ( 'NONE',  ( -40.38645765092156381, 8.586711236632284638, 34.59301614167199546 ) ) ;
#32224 = CARTESIAN_POINT ( 'NONE',  ( -30.48931983364116149, 3.805300331231239230, 15.71226580949866936 ) ) ;
#32225 = DIRECTION ( 'NONE',  ( -2.779292025043186357E-18, 1.288349127009862211E-17, -1.000000000000000000 ) ) ;
#32226 = TOROIDAL_SURFACE ( 'NONE', #29071, 29.50000000000000355, 2.000000000000001776 ) ;
#32227 = ORIENTED_EDGE ( 'NONE', *, *, #26425, .T. ) ;
#32228 = CARTESIAN_POINT ( 'NONE',  ( 21.09992658989239089, 23.84164230456639544, 47.04930799450051637 ) ) ;
#32229 = DIRECTION ( 'NONE',  ( 0.000000000000000000, 0.000000000000000000, 1.000000000000000000 ) ) ;
#32230 = CARTESIAN_POINT ( 'NONE',  ( 42.60075171692322726, 11.88159288520707868, -4.533495379785729362 ) ) ;
#32231 = ORIENTED_EDGE ( 'NONE', *, *, #26111, .T. ) ;
#32232 = VERTEX_POINT ( 'NONE', #12360 ) ;
#32234 = TOROIDAL_SURFACE ( 'NONE', #2357, 46.75000000000000000, 1.290569415042097656 ) ;
#32233 = CARTESIAN_POINT ( 'NONE',  ( 21.09785597605719332, 25.56454579224780232, -29.66074251183834676 ) ) ;
#32235 = CARTESIAN_POINT ( 'NONE',  ( 49.49063479933183629, 29.49951373492758933, 47.17357720316391578 ) ) ;
#32236 = AXIS2_PLACEMENT_3D ( 'NONE', #11409, #5688, #30797 ) ;
#32237 = AXIS2_PLACEMENT_3D ( 'NONE', #16018, #8313, #30488 ) ;
#32238 = DIRECTION ( 'NONE',  ( -0.000000000000000000, -1.000000000000000000, -0.000000000000000000 ) ) ;
#32239 = CARTESIAN_POINT ( 'NONE',  ( -39.44404620663942751, -5.935468836302990603, 77.98403960728234097 ) ) ;
#32240 = AXIS2_PLACEMENT_3D ( 'NONE', #25896, #461, #16043 ) ;
#32241 = CARTESIAN_POINT ( 'NONE',  ( -40.08841711228579641, 7.575633567407562552, 60.44930799450051495 ) ) ;
#32242 = VERTEX_POINT ( 'NONE', #6328 ) ;
#32243 = ORIENTED_EDGE ( 'NONE', *, *, #21401, .T. ) ;
#32244 = DIRECTION ( 'NONE',  ( -1.000000000000000000, -1.101824276508909887E-16, 0.000000000000000000 ) ) ;
#32245 = EDGE_CURVE ( 'NONE', #18805, #1639, #9885, .T. ) ;
#32246 = ORIENTED_EDGE ( 'NONE', *, *, #5846, .T. ) ;
#32247 = DIRECTION ( 'NONE',  ( -1.101824276508909887E-16, 1.000000000000000000, -0.000000000000000000 ) ) ;
#32248 = DIRECTION ( 'NONE',  ( -1.101824276508909887E-16, 1.000000000000000000, -0.000000000000000000 ) ) ;
#32249 = CIRCLE ( 'NONE', #10235, 12.36707279061065279 ) ;
#32250 = CIRCLE ( 'NONE', #12884, 12.62506659569710266 ) ;
#32251 = TOROIDAL_SURFACE ( 'NONE', #11817, 55.72393233686778302, 0.09999999999999760469 ) ;
#32252 = ORIENTED_EDGE ( 'NONE', *, *, #9040, .F. ) ;
#32253 = DIRECTION ( 'NONE',  ( -1.224646799147353207E-16, -1.349345573449484691E-32, 1.000000000000000000 ) ) ;
#32254 = VERTEX_POINT ( 'NONE', #18946 ) ;
#32255 = AXIS2_PLACEMENT_3D ( 'NONE', #6396, #3936, #27060 ) ;
#32256 = DIRECTION ( 'NONE',  ( 0.000000000000000000, 0.000000000000000000, -1.000000000000000000 ) ) ;
#32257 = EDGE_CURVE ( 'NONE', #6406, #19298, #24042, .T. ) ;
#32258 = CARTESIAN_POINT ( 'NONE',  ( 8.732853799281734553, 38.56284415653841791, 47.04930799450051637 ) ) ;
#32259 = ADVANCED_FACE ( 'NONE', ( #24208 ), #14528, .F. ) ;
#32260 = CARTESIAN_POINT ( 'NONE',  ( 21.09785597605719332, -6.314304012688826795, 47.04930799450051637 ) ) ;
#32261 = ORIENTED_EDGE ( 'NONE', *, *, #18554, .T. ) ;
#32262 = DIRECTION ( 'NONE',  ( 0.000000000000000000, 0.000000000000000000, -1.000000000000000000 ) ) ;
#32263 = CARTESIAN_POINT ( 'NONE',  ( 47.09785597605719687, 25.16454579224780019, 47.04930799450078638 ) ) ;
#32264 = CARTESIAN_POINT ( 'NONE',  ( -9.955189926603260631, -5.936918531481698125, -13.56792535344213313 ) ) ;
#32265 = DIRECTION ( 'NONE',  ( 0.000000000000000000, -0.7071067811865383579, -0.7071067811865566766 ) ) ;
#32266 = CARTESIAN_POINT ( 'NONE',  ( 21.09785597605719332, 13.06454579224780055, 47.04930799450051637 ) ) ;
#32267 = ORIENTED_EDGE ( 'NONE', *, *, #1929, .T. ) ;
#32268 = DIRECTION ( 'NONE',  ( 0.000000000000000000, 0.000000000000000000, -1.000000000000000000 ) ) ;
#32269 = DIRECTION ( 'NONE',  ( 0.000000000000000000, 1.000000000000000000, 0.000000000000000000 ) ) ;
#32270 = ORIENTED_EDGE ( 'NONE', *, *, #4625, .T. ) ;
#32271 = FACE_OUTER_BOUND ( 'NONE', #16946, .T. ) ;
#32272 = DIRECTION ( 'NONE',  ( -0.5319835227803600963, 0.2110602665713099124, 0.8200287161831868454 ) ) ;
#32273 = ORIENTED_EDGE ( 'NONE', *, *, #18477, .T. ) ;
#32274 = CONICAL_SURFACE ( 'NONE', #822, 40.18714373493281755, 0.6632251157578421541 ) ;
#32275 = VERTEX_POINT ( 'NONE', #29960 ) ;
#32276 = AXIS2_PLACEMENT_3D ( 'NONE', #4763, #30042, #22466 ) ;
#32277 = AXIS2_PLACEMENT_3D ( 'NONE', #9891, #20371, #27287 ) ;
#32278 = ADVANCED_FACE ( 'NONE', ( #19439 ), #9188, .F. ) ;
#32279 = VERTEX_POINT ( 'NONE', #19600 ) ;
#32280 = EDGE_CURVE ( 'NONE', #7700, #18486, #27546, .T. ) ;
#32281 = EDGE_CURVE ( 'NONE', #25889, #23946, #28057, .T. ) ;
#32282 = AXIS2_PLACEMENT_3D ( 'NONE', #23150, #667, #10700 ) ;
#32283 = DIRECTION ( 'NONE',  ( 1.188208965918165239E-16, 1.880121038077813132E-16, 1.000000000000000000 ) ) ;
#32284 = EDGE_LOOP ( 'NONE', ( #5435, #15885, #21085, #8786 ) ) ;
#32285 = EDGE_LOOP ( 'NONE', ( #11521, #2509, #27173, #4580 ) ) ;
#32286 = CARTESIAN_POINT ( 'NONE',  ( 75.54028429221254726, -2.844921901652561758, 13.31754327619664480 ) ) ;
#32287 = PLANE ( 'NONE',  #8367 ) ;
#32288 = DIRECTION ( 'NONE',  ( 0.000000000000000000, 0.7071067811865474617, 0.7071067811865474617 ) ) ;
#32289 = CARTESIAN_POINT ( 'NONE',  ( -36.37788479535792163, 9.471851136684824368, 54.54930799450051637 ) ) ;
#32290 = CARTESIAN_POINT ( 'NONE',  ( 21.09785597605720042, -16.03545420775220265, 47.04930799450051637 ) ) ;
#32291 = EDGE_CURVE ( 'NONE', #6807, #30857, #16514, .T. ) ;
#32292 = EDGE_LOOP ( 'NONE', ( #7754, #2457, #19422, #4495 ) ) ;
#32293 = DIRECTION ( 'NONE',  ( 0.000000000000000000, 0.000000000000000000, -1.000000000000000000 ) ) ;
#32294 = ORIENTED_EDGE ( 'NONE', *, *, #23110, .F. ) ;
#32295 = CARTESIAN_POINT ( 'NONE',  ( -31.01960144644215944, 5.215771264367748294, 16.56563741377133070 ) ) ;
#32297 = DIRECTION ( 'NONE',  ( -1.000000000000000000, -1.101824276508909887E-16, 0.000000000000000000 ) ) ;
#32296 = TOROIDAL_SURFACE ( 'NONE', #9230, 12.40141737965280733, 0.1250000000000013878 ) ;
#32298 = EDGE_LOOP ( 'NONE', ( #12754, #24431, #2723, #885 ) ) ;
#32299 = DIRECTION ( 'NONE',  ( 0.2756373558170082672, -0.9612616959383162296, 0.000000000000000000 ) ) ;
#32300 = LINE ( 'NONE', #30002, #32004 ) ;
#32301 = CARTESIAN_POINT ( 'NONE',  ( 52.18940074495291270, -5.936209625872266749, 107.6147842478074494 ) ) ;
#32302 = DIRECTION ( 'NONE',  ( 0.000000000000000000, 0.000000000000000000, -1.000000000000000000 ) ) ;
#32303 = DIRECTION ( 'NONE',  ( -1.101824276508909887E-16, 1.000000000000000000, -0.000000000000000000 ) ) ;
#32304 = CARTESIAN_POINT ( 'NONE',  ( 45.79384627280941089, 26.37957786121582160, 49.05938063676249072 ) ) ;
#32305 = DIRECTION ( 'NONE',  ( -0.000000000000000000, -1.000000000000000000, 0.000000000000000000 ) ) ;
#32306 = DIRECTION ( 'NONE',  ( 0.000000000000000000, 0.000000000000000000, -1.000000000000000000 ) ) ;
#32307 = ORIENTED_EDGE ( 'NONE', *, *, #32473, .T. ) ;
#32308 = CARTESIAN_POINT ( 'NONE',  ( 47.12478250753322584, 29.59809144869074160, 44.98302815556229461 ) ) ;
#32309 = FACE_OUTER_BOUND ( 'NONE', #26682, .T. ) ;
#32310 = ORIENTED_EDGE ( 'NONE', *, *, #8639, .F. ) ;
#32311 = TOROIDAL_SURFACE ( 'NONE', #18668, 46.75000000000000000, 1.290569415042097656 ) ;
#32312 = CARTESIAN_POINT ( 'NONE',  ( 21.09785597605720042, 11.92558985988973497, 103.7075660656323635 ) ) ;
#32313 = CARTESIAN_POINT ( 'NONE',  ( -42.38687957179150345, 4.148162238788004608, 58.24930799450051921 ) ) ;
#32314 = VERTEX_POINT ( 'NONE', #1722 ) ;
#32315 = EDGE_CURVE ( 'NONE', #2732, #29138, #4674, .T. ) ;
#32316 = ORIENTED_EDGE ( 'NONE', *, *, #1709, .T. ) ;
#32317 = CARTESIAN_POINT ( 'NONE',  ( 33.71785032049133690, 28.96664230456639899, 47.04930799450051637 ) ) ;
#32318 = B_SPLINE_CURVE_WITH_KNOTS ( 'NONE', 3,
 ( #32061, #12205, #26480, #26805, #1524, #19234, #29264, #1857, #9742, #17106, #6780, #19408, #4321, #29436, #14338, #3993, #24010, #6946, #14013, #4151, #21538, #31577, #9082, #19074, #29109, #7278, #15467, #23009, #27782, #15311, #25324, #7762, #10559, #5466 ),
 .UNSPECIFIED., .F., .F.,
 ( 4, 3, 3, 3, 3, 3, 3, 3, 3, 3, 3, 4 ),
 ( 0.000000000000000000, 2.818012925147974601E-05, 4.462336330430042420E-05, 5.702956313105841864E-05, 6.695137021320823726E-05, 7.690940289137861662E-05, 8.645711199579805470E-05, 0.0001018866409727163031, 0.0001271972541734457814, 0.0001703223122919903497, 0.0002159547541428134365, 0.0002238713945714089373 ),
 .UNSPECIFIED. ) ;
#32319 = EDGE_CURVE ( 'NONE', #6712, #30456, #22798, .T. ) ;
#32320 = ORIENTED_EDGE ( 'NONE', *, *, #27901, .T. ) ;
#32321 = CIRCLE ( 'NONE', #345, 13.20165371409683885 ) ;
#32322 = EDGE_CURVE ( 'NONE', #17291, #5246, #17498, .T. ) ;
#32323 = EDGE_CURVE ( 'NONE', #9250, #31904, #26991, .T. ) ;
#32324 = ORIENTED_EDGE ( 'NONE', *, *, #16298, .F. ) ;
#32325 = CARTESIAN_POINT ( 'NONE',  ( 8.732853799281725671, 25.97145308207318593, 47.04930799450051637 ) ) ;
#32326 = DIRECTION ( 'NONE',  ( -1.000000000000000000, 0.000000000000000000, 0.000000000000000000 ) ) ;
#32327 = AXIS2_PLACEMENT_3D ( 'NONE', #24968, #26942, #27594 ) ;
#32328 = ORIENTED_EDGE ( 'NONE', *, *, #12798, .T. ) ;
#32329 = SURFACE_STYLE_FILL_AREA ( #30518 ) ;
#32330 = DIRECTION ( 'NONE',  ( 0.4848096202463461624, 0.8746197071393907452, 9.920727850371670843E-18 ) ) ;
#32331 = LINE ( 'NONE', #9839, #15362 ) ;
#32332 = CARTESIAN_POINT ( 'NONE',  ( 47.20353132263855400, 29.60956182964376637, 45.01455027646041174 ) ) ;
#32333 = ORIENTED_EDGE ( 'NONE', *, *, #29023, .F. ) ;
#32334 = ORIENTED_EDGE ( 'NONE', *, *, #28799, .F. ) ;
#32335 = DIRECTION ( 'NONE',  ( -0.000000000000000000, -1.000000000000000000, -0.000000000000000000 ) ) ;
#32336 = ORIENTED_EDGE ( 'NONE', *, *, #17114, .F. ) ;
#32337 = DIRECTION ( 'NONE',  ( -1.101824276508909887E-16, 1.000000000000000000, -0.000000000000000000 ) ) ;
#32338 = CARTESIAN_POINT ( 'NONE',  ( -15.90214402394279958, 14.86454579224779948, 47.04930799450052348 ) ) ;
#32339 = DIRECTION ( 'NONE',  ( -1.101824276508909887E-16, 1.000000000000000000, -0.000000000000000000 ) ) ;
#32340 = CARTESIAN_POINT ( 'NONE',  ( 52.38208384728245193, -5.903366343041437148, -12.28331011554775465 ) ) ;
#32341 = CARTESIAN_POINT ( 'NONE',  ( 46.00908685603033632, 28.24624452788248874, 44.91496614357595263 ) ) ;
#32342 = CONTEXT_DEPENDENT_SHAPE_REPRESENTATION ( #14131, #27411 ) ;
#32343 = ORIENTED_EDGE ( 'NONE', *, *, #9964, .F. ) ;
#32344 = VERTEX_POINT ( 'NONE', #9274 ) ;
#32345 = DIRECTION ( 'NONE',  ( -1.101824276508909887E-16, 1.000000000000000000, -0.000000000000000000 ) ) ;
#32346 = CIRCLE ( 'NONE', #4024, 0.1000000000000018235 ) ;
#32347 = CARTESIAN_POINT ( 'NONE',  ( 44.87087493598345134, 28.87587066347688847, 48.18533415931919706 ) ) ;
#32348 = DIRECTION ( 'NONE',  ( 0.8746197071393926326, -0.4848096202463430537, -8.676864087101709653E-18 ) ) ;
#32349 = ORIENTED_EDGE ( 'NONE', *, *, #28398, .F. ) ;
#32350 = CARTESIAN_POINT ( 'NONE',  ( 45.79384627280941089, 28.56618040159425931, 49.05938063676249072 ) ) ;
#32351 = FACE_OUTER_BOUND ( 'NONE', #25436, .T. ) ;
#32352 = EDGE_CURVE ( 'NONE', #28041, #29304, #13908, .T. ) ;
#32353 = EDGE_LOOP ( 'NONE', ( #2474, #18283, #3421, #3785 ) ) ;
#32354 = FACE_OUTER_BOUND ( 'NONE', #28740, .T. ) ;
#32355 = CARTESIAN_POINT ( 'NONE',  ( 47.23302798462060537, 25.78121246473837758, 44.44659793406428605 ) ) ;
#32356 = ADVANCED_FACE ( 'NONE', ( #16814 ), #32251, .T. ) ;
#32357 = EDGE_CURVE ( 'NONE', #23803, #19744, #8145, .T. ) ;
#32358 = VERTEX_POINT ( 'NONE', #4352 ) ;
#32359 = EDGE_CURVE ( 'NONE', #2697, #27609, #6917, .T. ) ;
#32360 = ORIENTED_EDGE ( 'NONE', *, *, #13867, .T. ) ;
#32361 = CARTESIAN_POINT ( 'NONE',  ( 21.09785597605719687, 30.56454579224779522, 78.34930799450049221 ) ) ;
#32362 = AXIS2_PLACEMENT_3D ( 'NONE', #16099, #31056, #30578 ) ;
#32363 = CARTESIAN_POINT ( 'NONE',  ( 73.03464857846923053, 11.56016961077985350, 70.20130221674578763 ) ) ;
#32364 = FACE_OUTER_BOUND ( 'NONE', #12331, .T. ) ;
#32365 = ORIENTED_EDGE ( 'NONE', *, *, #27085, .T. ) ;
#32366 = VECTOR ( 'NONE', #1520, 1000.000000000000227 ) ;
#32367 = FACE_OUTER_BOUND ( 'NONE', #13618, .T. ) ;
#32368 = FACE_OUTER_BOUND ( 'NONE', #26350, .T. ) ;
#32369 = CARTESIAN_POINT ( 'NONE',  ( 48.14727188781975542, 19.96454579224779380, 49.10650501410607660 ) ) ;
#32370 = DIRECTION ( 'NONE',  ( 0.000000000000000000, 1.000000000000000000, -0.000000000000000000 ) ) ;
#32371 = CARTESIAN_POINT ( 'NONE',  ( -40.51565501380215295, 9.065589196111961456, 57.04930799450051637 ) ) ;
#32372 = DIRECTION ( 'NONE',  ( -0.1540342867254180514, 0.6907746437949934259, 0.7064728091037132396 ) ) ;
#32373 = CARTESIAN_POINT ( 'NONE',  ( 47.70546624744041253, 14.98691807112498964, 47.08086432685907852 ) ) ;
#32374 = B_SPLINE_SURFACE_WITH_KNOTS ( 'NONE', 3, 1, ( 
 ( #14899, #24409 ),
 ( #1920, #29672 ),
 ( #2256, #32459 ),
 ( #9971, #15059 ) ),
 .UNSPECIFIED., .F., .F., .F.,
 ( 4, 4 ),
 ( 2, 2 ),
 ( 0.1800733115436725096, 0.1889470565094412691 ),
 ( 0.000000000000000000, 1.000000000000000000 ),
 .UNSPECIFIED. ) ;
#32375 = LINE ( 'NONE', #21252, #22284 ) ;
#32376 = SURFACE_SIDE_STYLE ('',( #22999 ) ) ;
#32377 = ORIENTED_EDGE ( 'NONE', *, *, #25819, .F. ) ;
#32378 = ORIENTED_EDGE ( 'NONE', *, *, #4828, .F. ) ;
#32379 = DIRECTION ( 'NONE',  ( 0.000000000000000000, 0.000000000000000000, 1.000000000000000000 ) ) ;
#32380 = CARTESIAN_POINT ( 'NONE',  ( 21.09785597605719332, 25.56454579224779877, 21.04930799450051282 ) ) ;
#32381 = DIRECTION ( 'NONE',  ( -1.224646799147353207E-16, -1.349345573449484691E-32, 1.000000000000000000 ) ) ;
#32382 = CARTESIAN_POINT ( 'NONE',  ( 49.19517401419062708, 27.00920399681022843, 48.40991706654173754 ) ) ;
#32383 = ORIENTED_EDGE ( 'NONE', *, *, #21822, .F. ) ;
#32384 = DIRECTION ( 'NONE',  ( -1.101824276508909887E-16, 1.000000000000000000, -0.000000000000000000 ) ) ;
#32385 = LINE ( 'NONE', #7763, #17937 ) ;
#32386 = CARTESIAN_POINT ( 'NONE',  ( 42.05571303064796496, 11.92558985988973141, -4.731146760523925465 ) ) ;
#32387 = ORIENTED_EDGE ( 'NONE', *, *, #26569, .F. ) ;
#32388 = ORIENTED_EDGE ( 'NONE', *, *, #32053, .F. ) ;
#32389 = LINE ( 'NONE', #9904, #23603 ) ;
#32390 = CARTESIAN_POINT ( 'NONE',  ( 48.35473289974373756, 22.86454579224779948, 45.11188864597615833 ) ) ;
#32391 = CIRCLE ( 'NONE', #31348, 13.20165371409683885 ) ;
#32392 = DIRECTION ( 'NONE',  ( -0.000000000000000000, -1.000000000000000000, -0.000000000000000000 ) ) ;
#32393 = AXIS2_PLACEMENT_3D ( 'NONE', #7028, #31978, #6873 ) ;
#32394 = DIRECTION ( 'NONE',  ( -1.000000000000000000, 0.000000000000000000, 0.000000000000000000 ) ) ;
#32395 = CARTESIAN_POINT ( 'NONE',  ( 46.05267182906204226, 29.39183878387655824, 49.07307072161059835 ) ) ;
#32396 = CIRCLE ( 'NONE', #2517, 1.300000000000002487 ) ;
#32397 = EDGE_LOOP ( 'NONE', ( #17702, #29380 ) ) ;
#32398 = B_SPLINE_CURVE_WITH_KNOTS ( 'NONE', 3,
 ( #30202, #12484, #29880, #32340, #10181, #9850, #25110, #25274 ),
 .UNSPECIFIED., .F., .F.,
 ( 4, 2, 2, 4 ),
 ( 1.734723475976807094E-17, 0.0004427811193176344959, 0.0008855622386352516445, 0.001771124477270482039 ),
 .UNSPECIFIED. ) ;
#32399 = EDGE_CURVE ( 'NONE', #30019, #2146, #14961, .T. ) ;
#32400 = ORIENTED_EDGE ( 'NONE', *, *, #26202, .T. ) ;
#32401 = ADVANCED_FACE ( 'NONE', ( #25189 ), #7637, .T. ) ;
#32402 = EDGE_CURVE ( 'NONE', #10039, #6352, #17028, .T. ) ;
#32403 = EDGE_CURVE ( 'NONE', #10702, #3113, #31730, .T. ) ;
#32404 = CARTESIAN_POINT ( 'NONE',  ( -40.51045226066063520, 7.589116544599140646, 53.87859731638185679 ) ) ;
#32405 = EDGE_CURVE ( 'NONE', #20217, #5246, #23208, .T. ) ;
#32406 = ORIENTED_EDGE ( 'NONE', *, *, #22751, .T. ) ;
#32407 = CARTESIAN_POINT ( 'NONE',  ( -40.14060284811700541, 7.788019651925919717, 34.54930799450052348 ) ) ;
#32408 = CARTESIAN_POINT ( 'NONE',  ( 8.732853799281734553, 38.56284415653841791, 47.04930799450051637 ) ) ;
#32409 = AXIS2_PLACEMENT_3D ( 'NONE', #23826, #25810, #6271 ) ;
#32410 = AXIS2_PLACEMENT_3D ( 'NONE', #11098, #28488, #25535 ) ;
#32411 = ORIENTED_EDGE ( 'NONE', *, *, #1968, .T. ) ;
#32412 = FACE_OUTER_BOUND ( 'NONE', #14579, .T. ) ;
#32413 = ORIENTED_EDGE ( 'NONE', *, *, #26413, .F. ) ;
#32414 = TOROIDAL_SURFACE ( 'NONE', #31354, 54.10000000000000142, 0.1999999999999994282 ) ;
#32415 = FACE_OUTER_BOUND ( 'NONE', #6707, .T. ) ;
#32416 = VECTOR ( 'NONE', #6029, 1000.000000000000114 ) ;
#32417 = CARTESIAN_POINT ( 'NONE',  ( 8.732853799281734553, 29.97145308207317527, 47.04930799450051637 ) ) ;
#32418 = CARTESIAN_POINT ( 'NONE',  ( -40.09211399732166115, 9.667069410243957606, 34.64930799450051779 ) ) ;
#32419 = ORIENTED_EDGE ( 'NONE', *, *, #6149, .T. ) ;
#32420 = FACE_OUTER_BOUND ( 'NONE', #1163, .T. ) ;
#32421 = CARTESIAN_POINT ( 'NONE',  ( -9.880269303432738681, -5.935454207752202116, -13.48461434800281289 ) ) ;
#32422 = DIRECTION ( 'NONE',  ( -1.000000000000000000, 0.000000000000000000, 0.000000000000000000 ) ) ;
#32423 = FACE_OUTER_BOUND ( 'NONE', #5986, .T. ) ;
#32424 = AXIS2_PLACEMENT_3D ( 'NONE', #12183, #15291, #24815 ) ;
#32425 = CARTESIAN_POINT ( 'NONE',  ( 47.09785597605719687, 30.56454579224779522, 49.54930799450078638 ) ) ;
#32426 = ORIENTED_EDGE ( 'NONE', *, *, #8345, .F. ) ;
#32427 = DIRECTION ( 'NONE',  ( -0.9612616959383200044, -0.2756373558169954996, 1.660411357259285896E-16 ) ) ;
#32428 = ORIENTED_EDGE ( 'NONE', *, *, #25793, .T. ) ;
#32430 = EDGE_CURVE ( 'NONE', #22442, #8660, #10418, .T. ) ;
#32429 = DIRECTION ( 'NONE',  ( -1.000000000000000000, -1.101824276508909887E-16, 0.000000000000000000 ) ) ;
#32431 = CARTESIAN_POINT ( 'NONE',  ( 21.09785597605719332, -19.93545420775220123, 131.3493079945005491 ) ) ;
#32432 = ORIENTED_EDGE ( 'NONE', *, *, #7599, .F. ) ;
#32433 = DIRECTION ( 'NONE',  ( 0.000000000000000000, 0.000000000000000000, 1.000000000000000000 ) ) ;
#32434 = ORIENTED_EDGE ( 'NONE', *, *, #19134, .T. ) ;
#32435 = PRODUCT_DEFINITION_CONTEXT ( 'detailed design', #9095, 'design' ) ;
#32436 = AXIS2_PLACEMENT_3D ( 'NONE', #21239, #31272, #6317 ) ;
#32437 = CIRCLE ( 'NONE', #8826, 12.62506659569710266 ) ;
#32438 = ORIENTED_EDGE ( 'NONE', *, *, #4106, .F. ) ;
#32439 = CIRCLE ( 'NONE', #16155, 0.09999999999999795164 ) ;
#32440 = ADVANCED_FACE ( 'NONE', ( #8116 ), #25427, .T. ) ;
#32441 = EDGE_CURVE ( 'NONE', #490, #24509, #24407, .T. ) ;
#32442 = ADVANCED_FACE ( 'NONE', ( #10588 ), #25977, .F. ) ;
#32443 = CIRCLE ( 'NONE', #26654, 12.27641737965287128 ) ;
#32444 = EDGE_CURVE ( 'NONE', #22288, #7112, #1872, .T. ) ;
#32445 = CIRCLE ( 'NONE', #31382, 2.923537884824412014 ) ;
#32446 = DIRECTION ( 'NONE',  ( -0.000000000000000000, -1.000000000000000000, 0.000000000000000000 ) ) ;
#32447 = ORIENTED_EDGE ( 'NONE', *, *, #9790, .F. ) ;
#32448 = ORIENTED_EDGE ( 'NONE', *, *, #6836, .T. ) ;
#32449 = DIRECTION ( 'NONE',  ( 0.6184495258776571136, -0.3428121700606572286, 0.7071067811865504593 ) ) ;
#32450 = CARTESIAN_POINT ( 'NONE',  ( 21.09785597605719332, -12.82881809906321458, 47.04930799450051637 ) ) ;
#32451 = DIRECTION ( 'NONE',  ( 0.000000000000000000, -0.1908089953765421121, -0.9816271834476645308 ) ) ;
#32452 = FACE_OUTER_BOUND ( 'NONE', #22363, .T. ) ;
#32453 = ORIENTED_EDGE ( 'NONE', *, *, #30185, .F. ) ;
#32454 = CARTESIAN_POINT ( 'NONE',  ( -10.65234575671300021, -5.769399297529553827, 104.5301199837775812 ) ) ;
#32455 = VERTEX_POINT ( 'NONE', #22722 ) ;
#32456 = DIRECTION ( 'NONE',  ( -1.000000000000000000, 0.000000000000000000, 0.000000000000000000 ) ) ;
#32457 = CIRCLE ( 'NONE', #11474, 12.62506659569710266 ) ;
#32458 = ORIENTED_EDGE ( 'NONE', *, *, #2984, .F. ) ;
#32459 = CARTESIAN_POINT ( 'NONE',  ( 81.54161849434414933, -5.937394935145312580, 77.97850100859398026 ) ) ;
#32460 = CARTESIAN_POINT ( 'NONE',  ( -41.52218637998915085, 11.15499190493234671, 37.04930799450052348 ) ) ;
#32461 = VECTOR ( 'NONE', #5027, 1000.000000000000114 ) ;
#32462 = DIRECTION ( 'NONE',  ( 0.000000000000000000, -0.000000000000000000, -1.000000000000000000 ) ) ;
#32463 = CARTESIAN_POINT ( 'NONE',  ( 21.09785597605719332, 30.56454579224779522, 47.04930799450051637 ) ) ;
#32464 = CARTESIAN_POINT ( 'NONE',  ( 21.09992658989239089, 26.84143805560860940, 47.04930799450051637 ) ) ;
#32465 = CARTESIAN_POINT ( 'NONE',  ( 47.20547626766766314, 26.08791119454915730, 44.97710074790751378 ) ) ;
#32466 = DIRECTION ( 'NONE',  ( -0.8746197071393926326, 0.4848096202463430537, 8.676864087101709653E-18 ) ) ;
#32467 = DIRECTION ( 'NONE',  ( -1.101824276508909887E-16, 1.000000000000000000, -0.000000000000000000 ) ) ;
#32468 = VERTEX_POINT ( 'NONE', #15338 ) ;
#32469 = FACE_OUTER_BOUND ( 'NONE', #14809, .T. ) ;
#32471 = ADVANCED_FACE ( 'NONE', ( #18112, #389 ), #25349, .F. ) ;
#32470 = CARTESIAN_POINT ( 'NONE',  ( -40.28136326135769707, 8.248516754564388265, 54.59072935073782418 ) ) ;
#32472 = ORIENTED_EDGE ( 'NONE', *, *, #20670, .T. ) ;
#32473 = EDGE_CURVE ( 'NONE', #18486, #31589, #5644, .T. ) ;
#32474 = AXIS2_PLACEMENT_3D ( 'NONE', #17719, #20508, #28069 ) ;
#32475 = DIRECTION ( 'NONE',  ( 0.8746197071393926326, -0.4848096202463430537, -8.676864087101709653E-18 ) ) ;
#32476 = ORIENTED_EDGE ( 'NONE', *, *, #15450, .T. ) ;
#32477 = ORIENTED_EDGE ( 'NONE', *, *, #5846, .F. ) ;
#32478 = DIRECTION ( 'NONE',  ( 0.000000000000000000, 0.000000000000000000, -1.000000000000000000 ) ) ;
#32479 = ORIENTED_EDGE ( 'NONE', *, *, #4567, .F. ) ;
#32480 = EDGE_CURVE ( 'NONE', #6910, #25250, #3170, .T. ) ;
#32481 = CIRCLE ( 'NONE', #30374, 19.18998195308981636 ) ;
#32482 = AXIS2_PLACEMENT_3D ( 'NONE', #28312, #5832, #12906 ) ;
#32483 = VERTEX_POINT ( 'NONE', #27491 ) ;
#32484 = CARTESIAN_POINT ( 'NONE',  ( 45.40326095744675428, 22.93807716476589675, 47.12319401418537268 ) ) ;
#32485 = AXIS2_PLACEMENT_3D ( 'NONE', #17072, #4603, #27089 ) ;
#32486 = AXIS2_PLACEMENT_3D ( 'NONE', #13859, #31743, #26488 ) ;
#32487 = ORIENTED_EDGE ( 'NONE', *, *, #16517, .T. ) ;
#32488 = CARTESIAN_POINT ( 'NONE',  ( 21.09785597605719332, -13.74048473023143835, 105.2732083928529221 ) ) ;
#32489 = AXIS2_PLACEMENT_3D ( 'NONE', #31021, #16069, #21144 ) ;
#32490 = CARTESIAN_POINT ( 'NONE',  ( -40.80097511801616150, 8.246641009394465982, 54.54930799450051637 ) ) ;
#32491 = CARTESIAN_POINT ( 'NONE',  ( 21.09785597605719687, 2.299431449832689545, 47.04930799450051637 ) ) ;
#32492 = EDGE_CURVE ( 'NONE', #19917, #23906, #15021, .T. ) ;
#32493 = CARTESIAN_POINT ( 'NONE',  ( 45.28286642839709231, 29.14289516297709071, 47.97516931882780966 ) ) ;
#32494 = VECTOR ( 'NONE', #19078, 1000.000000000000000 ) ;
#32495 = EDGE_LOOP ( 'NONE', ( #23512, #919, #25871, #4014 ) ) ;
#32496 = ORIENTED_EDGE ( 'NONE', *, *, #22252, .F. ) ;
#32497 = DIRECTION ( 'NONE',  ( 0.000000000000000000, -1.000000000000000000, -0.000000000000000000 ) ) ;
#32498 = NEXT_ASSEMBLY_USAGE_OCCURRENCE ( 'NAUO1', ' ', ' ', #17544, #8108, $ ) ;
#32499 = NEXT_ASSEMBLY_USAGE_OCCURRENCE ( 'NAUO2', ' ', ' ', #17544, #25954, $ ) ;
#32500 = NEXT_ASSEMBLY_USAGE_OCCURRENCE ( 'NAUO3', ' ', ' ', #17544, #27968, $ ) ;
#32501 = NEXT_ASSEMBLY_USAGE_OCCURRENCE ( 'NAUO4', ' ', ' ', #17544, #8511, $ ) ;
#32502 = NEXT_ASSEMBLY_USAGE_OCCURRENCE ( 'NAUO5', ' ', ' ', #17544, #31780, $ ) ;
#32503 = NEXT_ASSEMBLY_USAGE_OCCURRENCE ( 'NAUO6', ' ', ' ', #17544, #9511, $ ) ;
#32504 = NEXT_ASSEMBLY_USAGE_OCCURRENCE ( 'NAUO7', ' ', ' ', #17544, #8905, $ ) ;
#32505 = NEXT_ASSEMBLY_USAGE_OCCURRENCE ( 'NAUO8', ' ', ' ', #17544, #18711, $ ) ;
#32506 = NEXT_ASSEMBLY_USAGE_OCCURRENCE ( 'NAUO9', ' ', ' ', #17544, #18711, $ ) ;
#32507 = NEXT_ASSEMBLY_USAGE_OCCURRENCE ( 'NAUO10', ' ', ' ', #17544, #18711, $ ) ;
#32508 = NEXT_ASSEMBLY_USAGE_OCCURRENCE ( 'NAUO11', ' ', ' ', #17544, #18711, $ ) ;
#32509=COLOUR_RGB('Dark Blue',0.08,0.2,0.34);
#32510=FILL_AREA_STYLE_COLOUR('',#32509);
#32511=FILL_AREA_STYLE('',(#32510));
#32512=SURFACE_STYLE_FILL_AREA(#32511);
#32513=SURFACE_SIDE_STYLE('',(#32512));
#32514=SURFACE_STYLE_USAGE(.BOTH.,#32513);
#32515=PRESENTATION_STYLE_ASSIGNMENT((#32514));
#32516=COLOUR_RGB('Light Blue',0.38,0.62,0.78);
#32517=FILL_AREA_STYLE_COLOUR('',#32516);
#32518=FILL_AREA_STYLE('',(#32517));
#32519=SURFACE_STYLE_FILL_AREA(#32518);
#32520=SURFACE_SIDE_STYLE('',(#32519));
#32521=SURFACE_STYLE_USAGE(.BOTH.,#32520);
#32522=PRESENTATION_STYLE_ASSIGNMENT((#32521));
#32523=COLOUR_RGB('Sky Blue',0.24,0.69,0.87);
#32524=FILL_AREA_STYLE_COLOUR('',#32523);
#32525=FILL_AREA_STYLE('',(#32524));
#32526=SURFACE_STYLE_FILL_AREA(#32525);
#32527=SURFACE_SIDE_STYLE('',(#32526));
#32528=SURFACE_STYLE_USAGE(.BOTH.,#32527);
#32529=PRESENTATION_STYLE_ASSIGNMENT((#32528));
#32530=COLOUR_RGB('Grey',0.48,0.52,0.57);
#32531=FILL_AREA_STYLE_COLOUR('',#32530);
#32532=FILL_AREA_STYLE('',(#32531));
#32533=SURFACE_STYLE_FILL_AREA(#32532);
#32534=SURFACE_SIDE_STYLE('',(#32533));
#32535=SURFACE_STYLE_USAGE(.BOTH.,#32534);
#32536=PRESENTATION_STYLE_ASSIGNMENT((#32535));
#32537=COLOUR_RGB('Black',0.12,0.14,0.17);
#32538=FILL_AREA_STYLE_COLOUR('',#32537);
#32539=FILL_AREA_STYLE('',(#32538));
#32540=SURFACE_STYLE_FILL_AREA(#32539);
#32541=SURFACE_SIDE_STYLE('',(#32540));
#32542=SURFACE_STYLE_USAGE(.BOTH.,#32541);
#32543=PRESENTATION_STYLE_ASSIGNMENT((#32542));
#32544=COLOUR_RGB('Off White',0.89,0.88,0.83);
#32545=FILL_AREA_STYLE_COLOUR('',#32544);
#32546=FILL_AREA_STYLE('',(#32545));
#32547=SURFACE_STYLE_FILL_AREA(#32546);
#32548=SURFACE_SIDE_STYLE('',(#32547));
#32549=SURFACE_STYLE_USAGE(.BOTH.,#32548);
#32550=PRESENTATION_STYLE_ASSIGNMENT((#32549));
ENDSEC;
END-ISO-10303-21;
